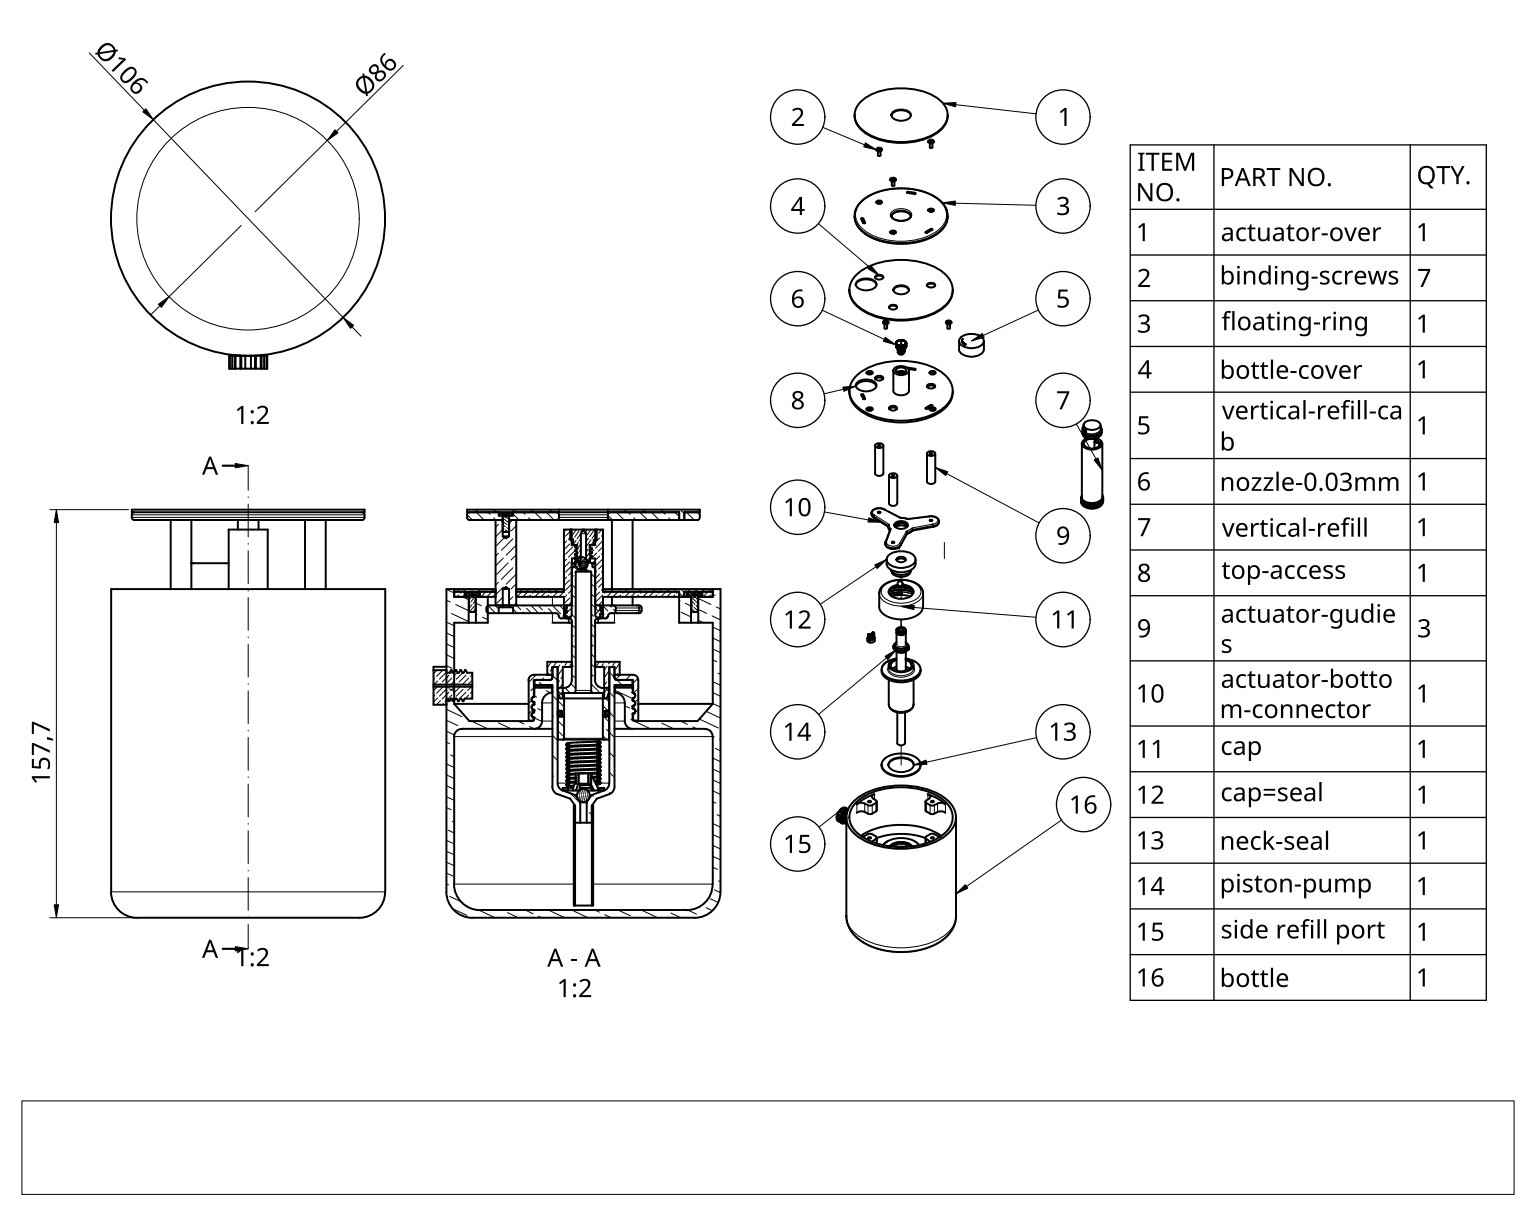
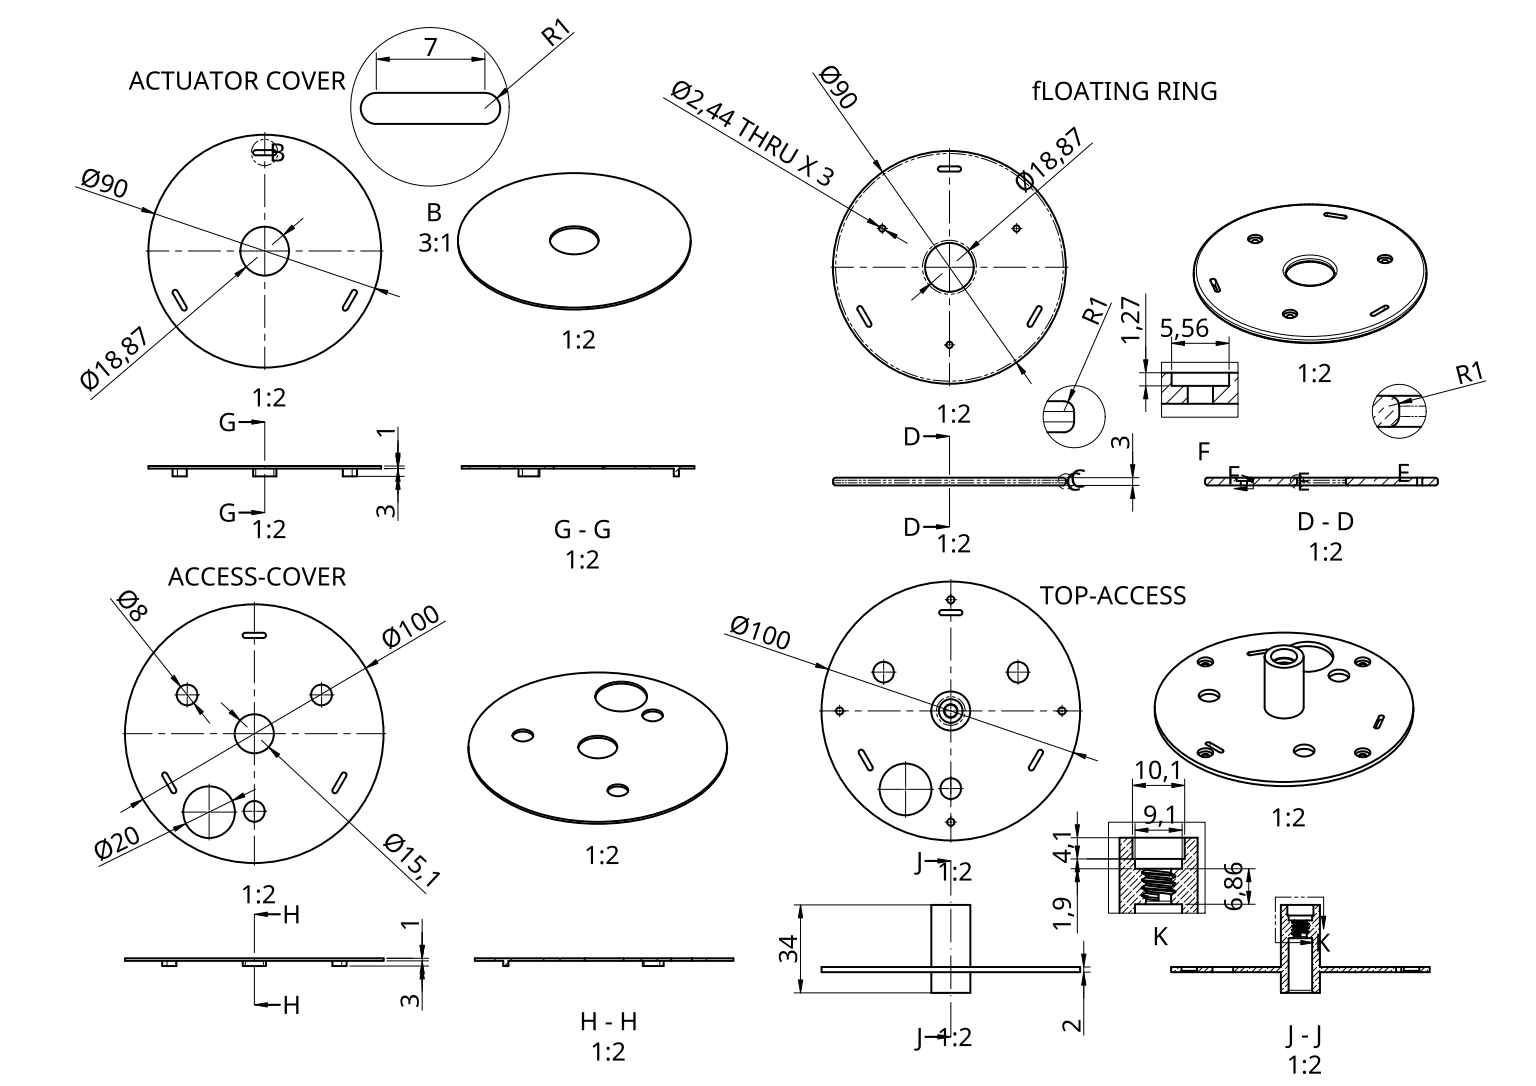
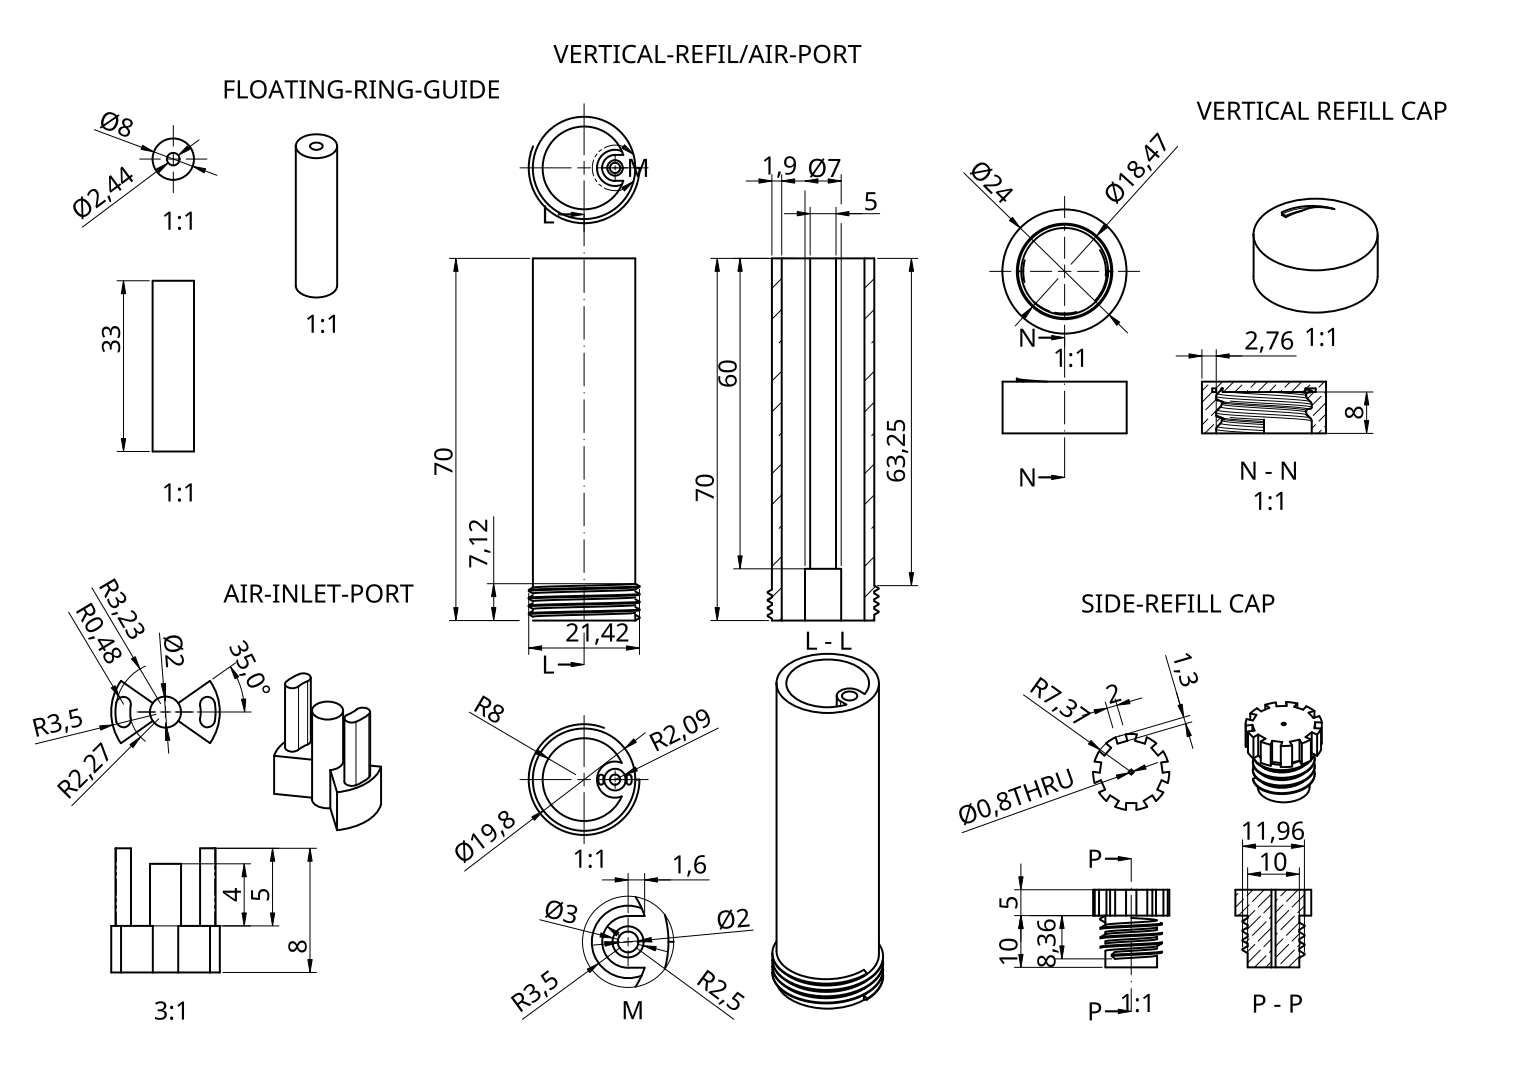
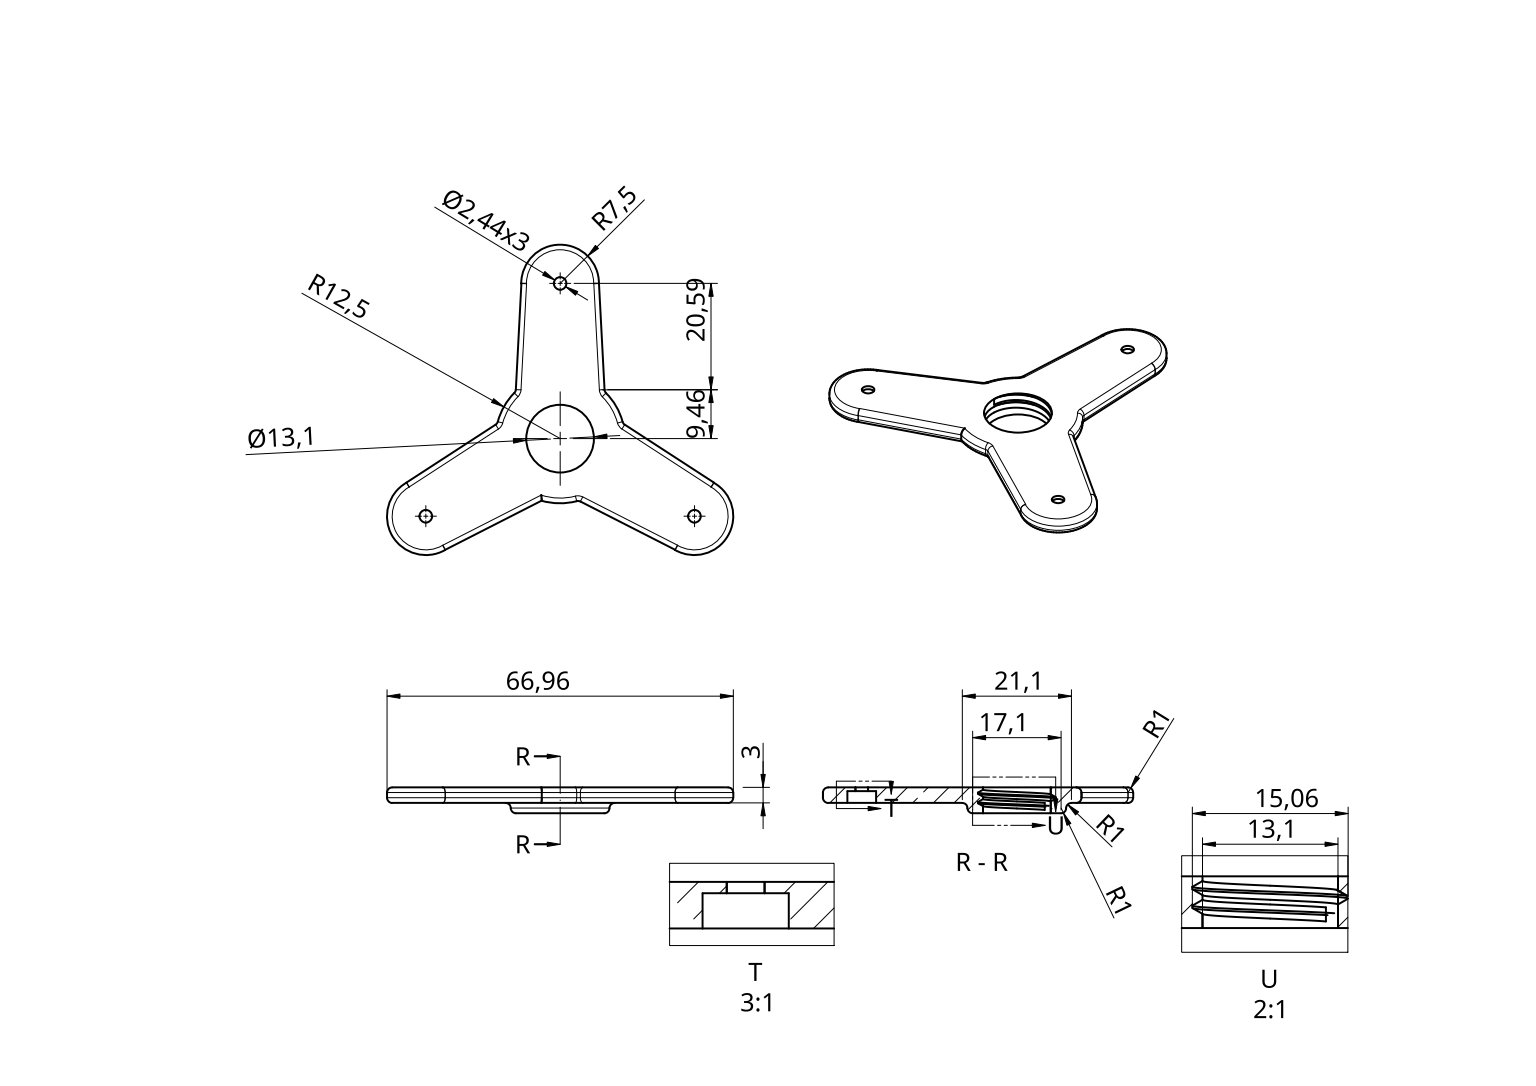
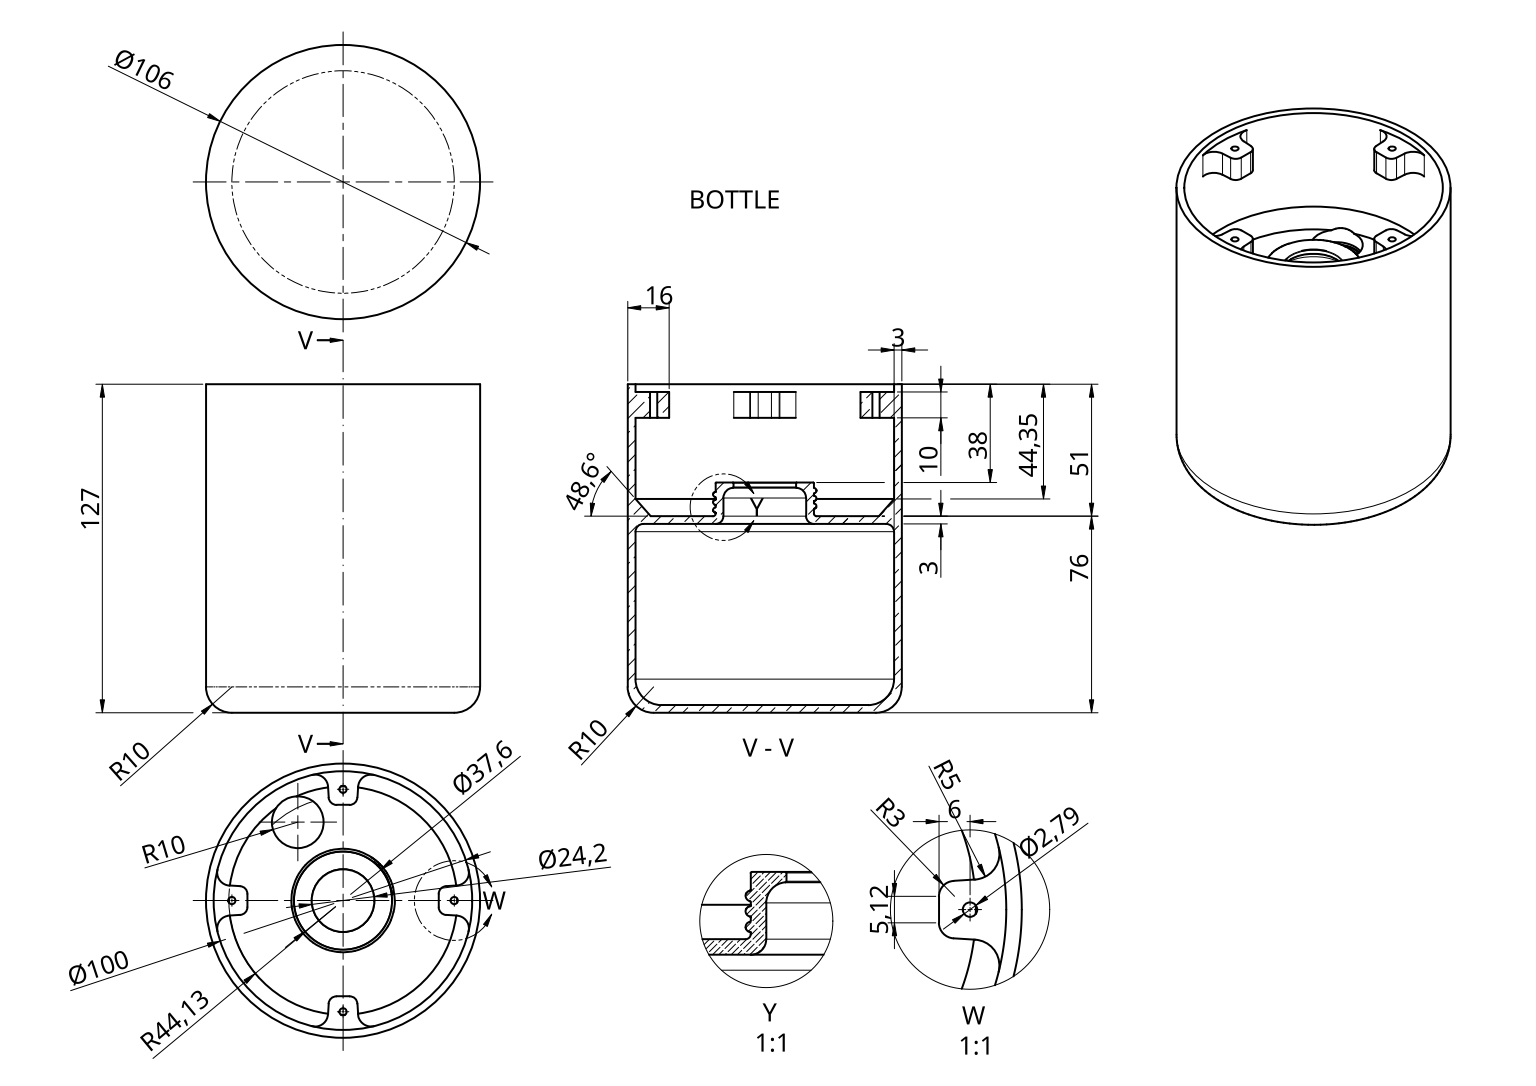
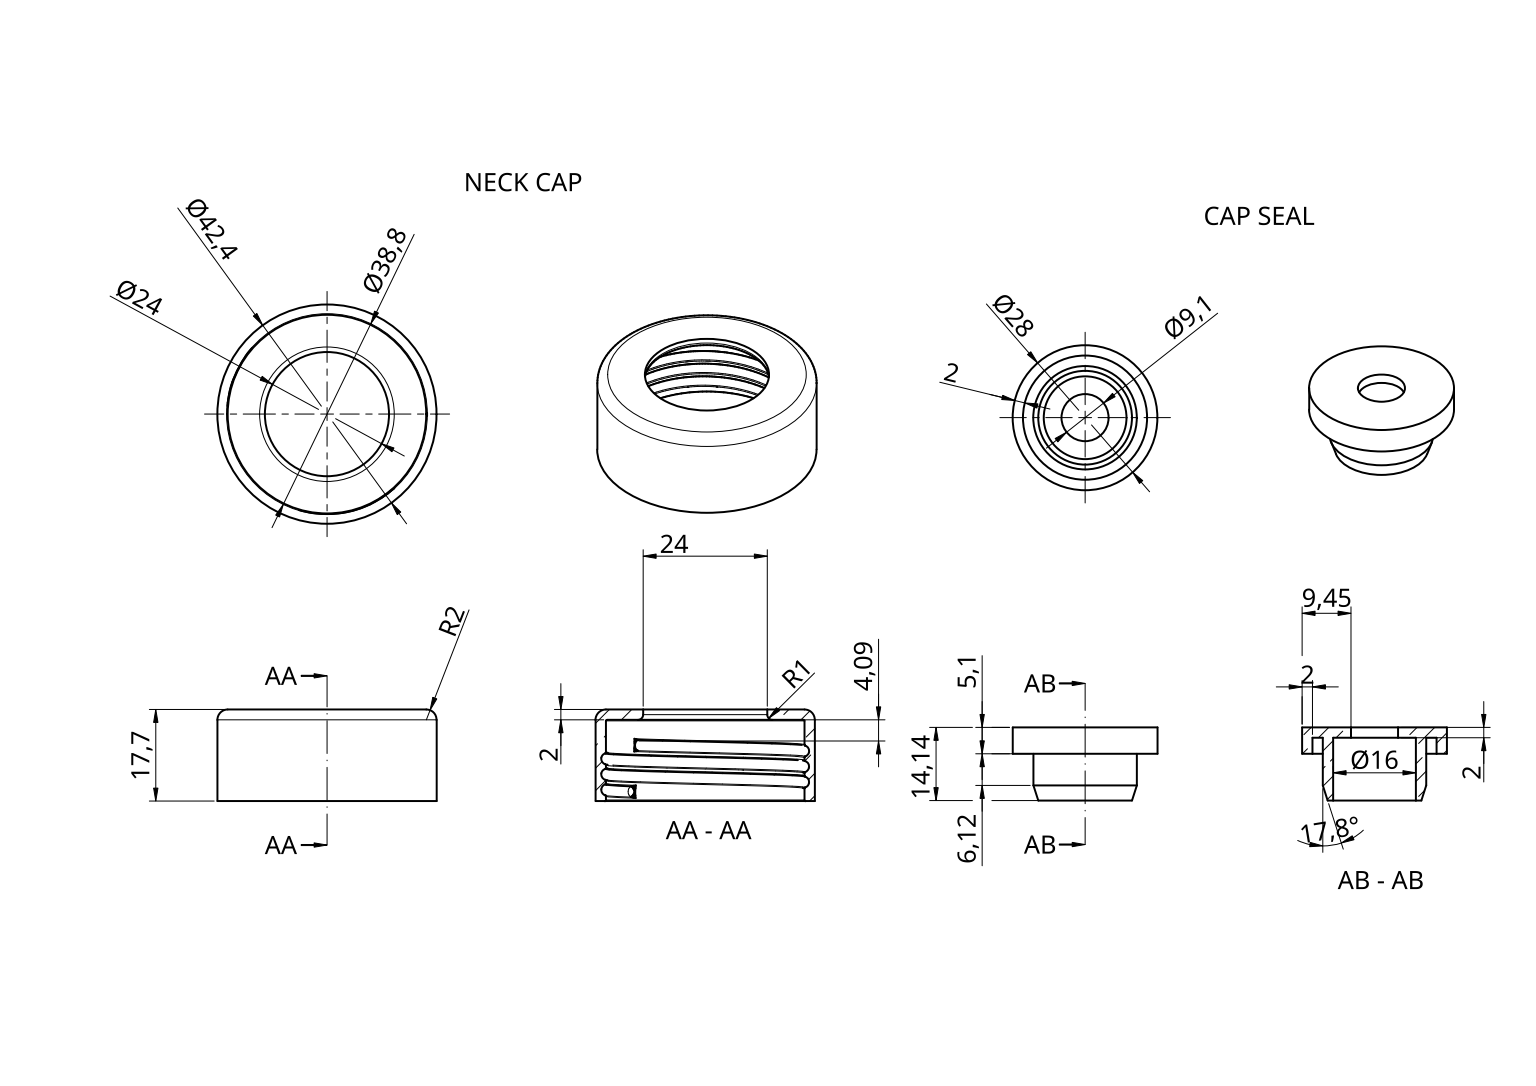
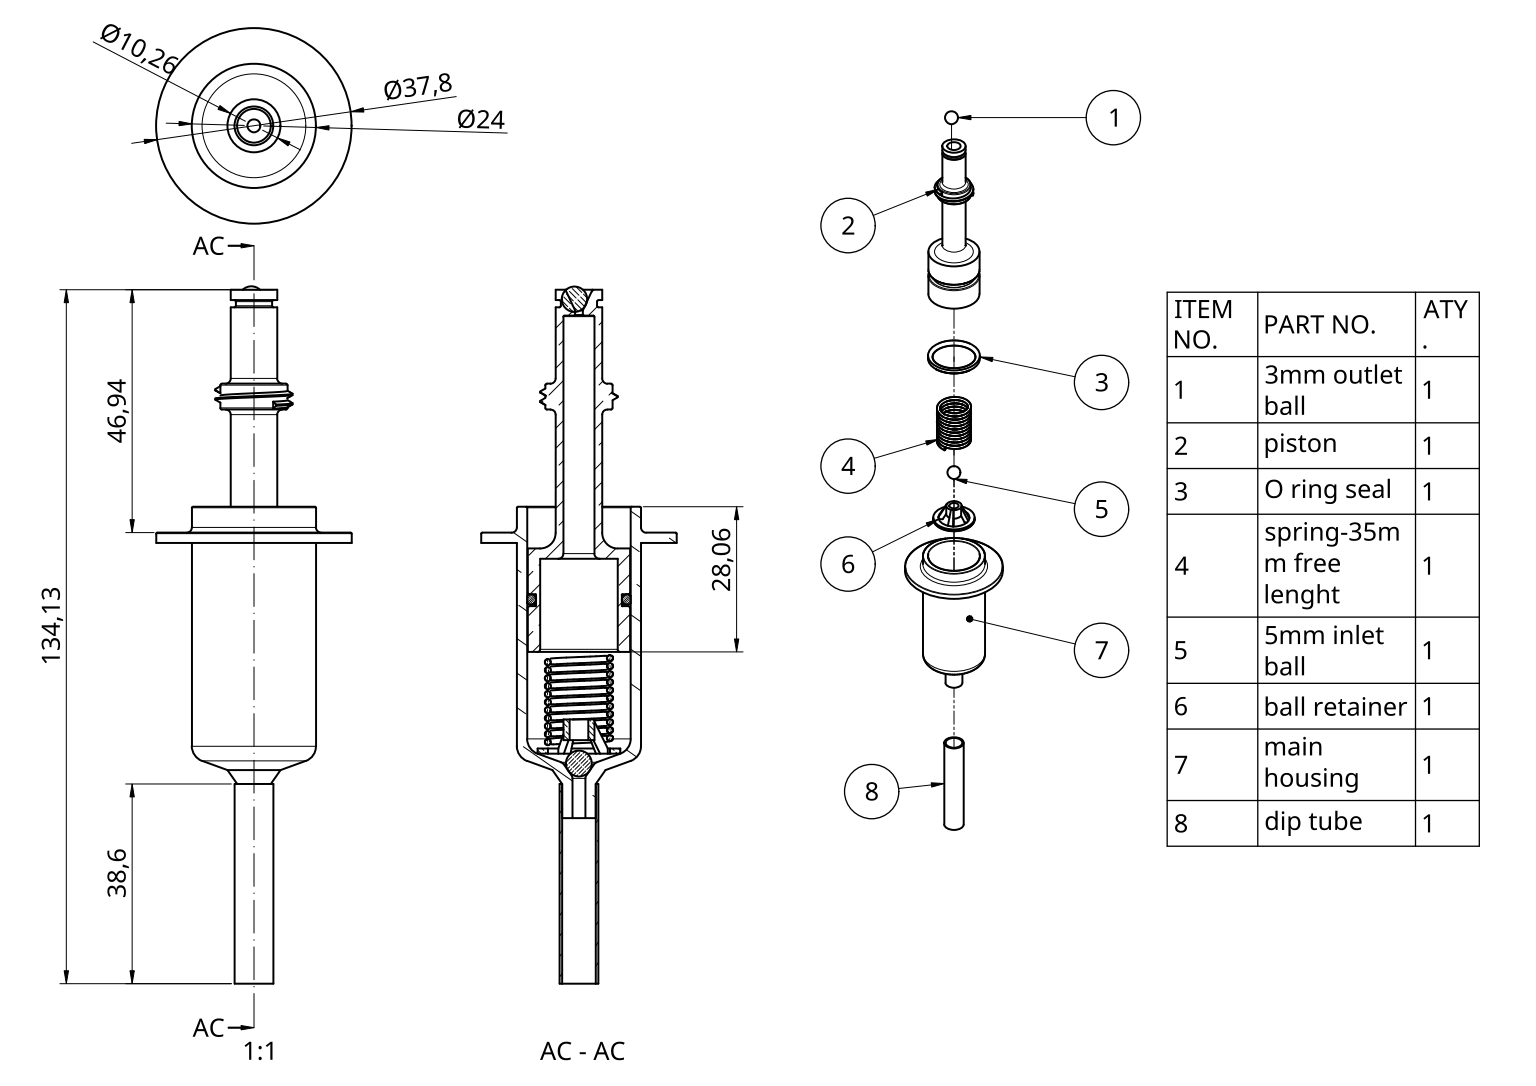
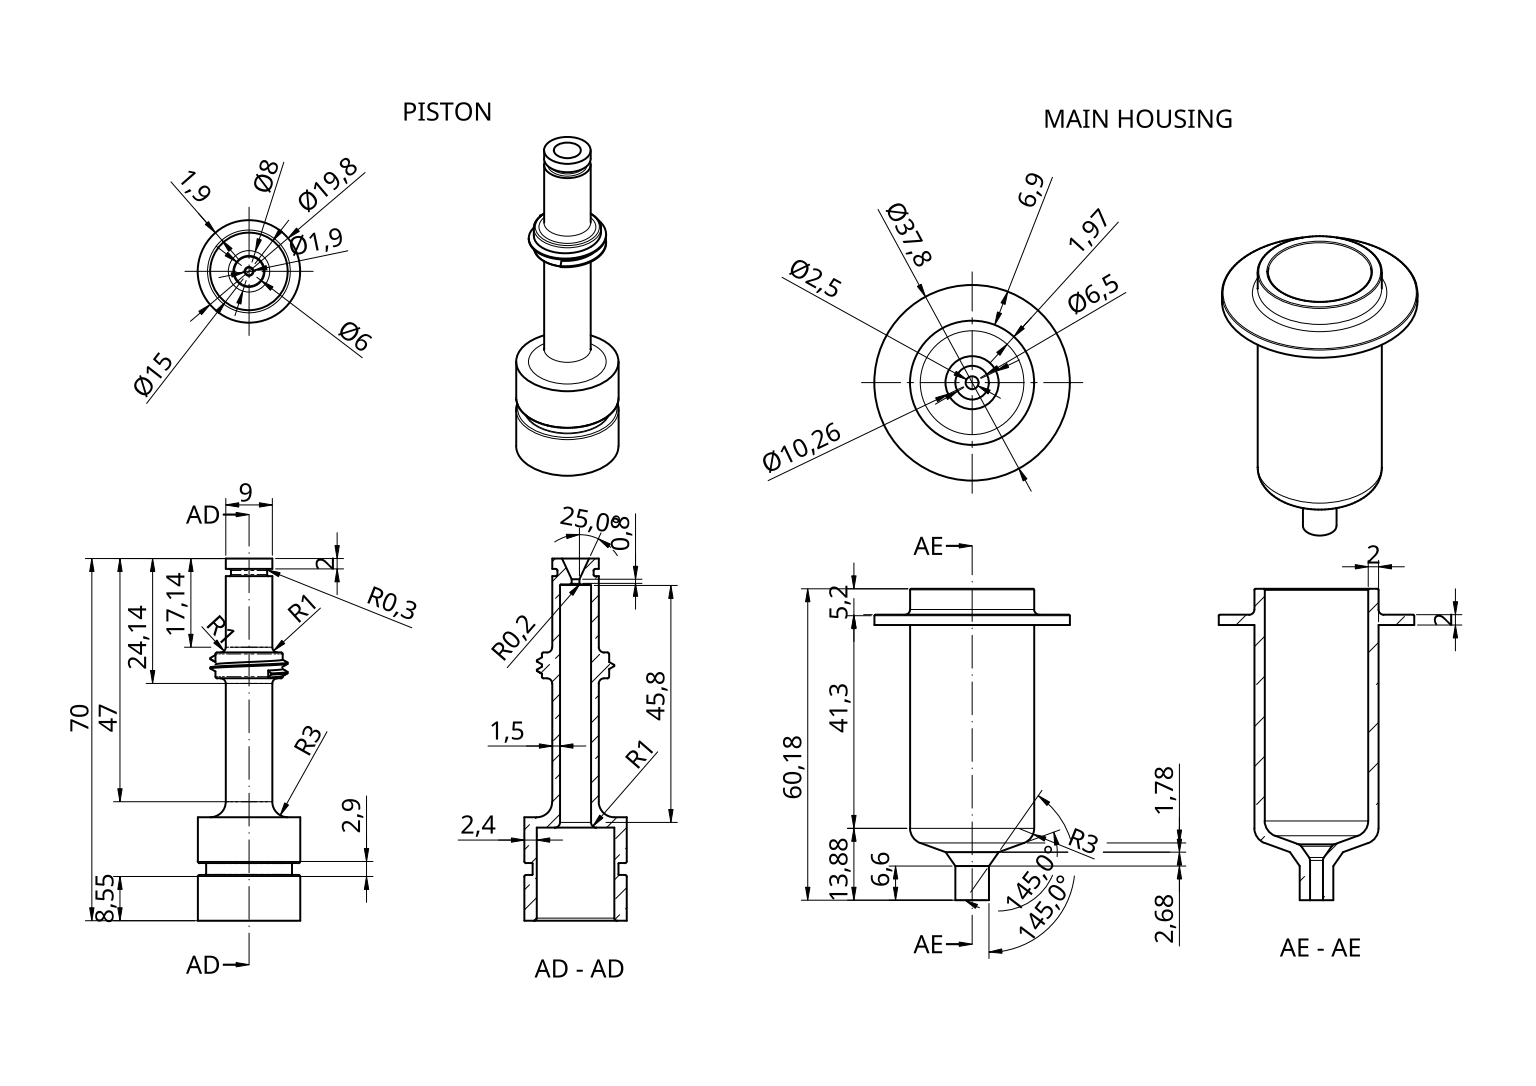
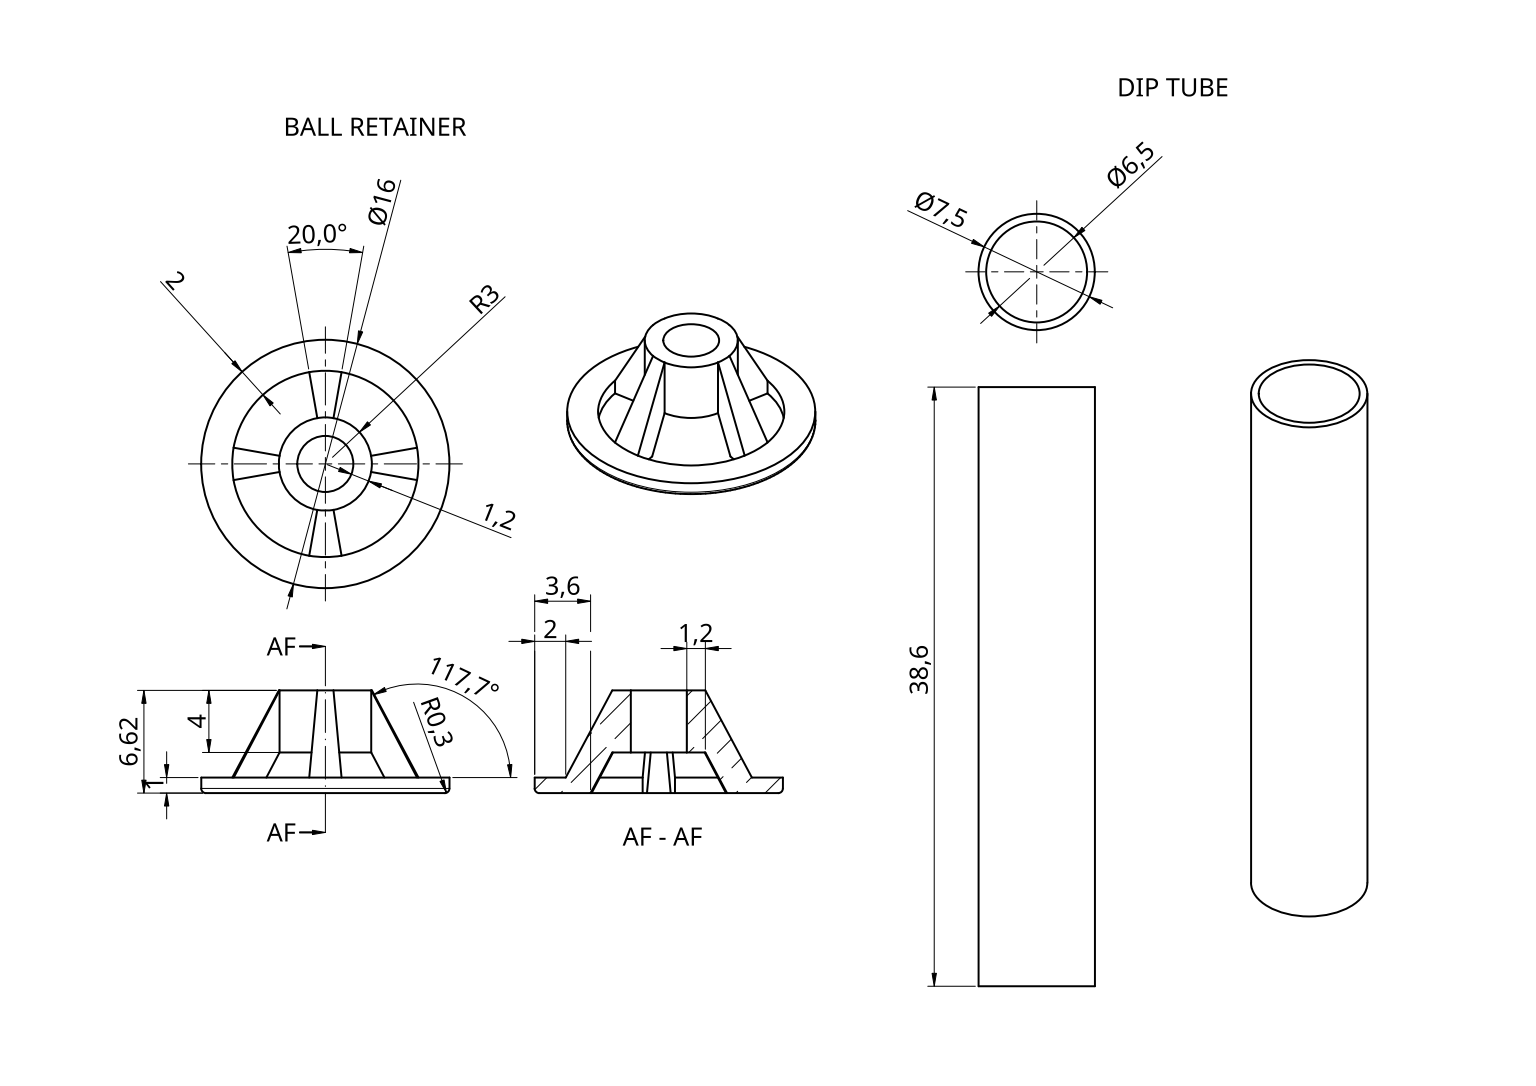
ISO-10303-21;
HEADER;
/* Generated by software containing ST-Developer
 * from STEP Tools, Inc. (www.steptools.com) 
 */
/* OPTION: using custom renumber hook */

FILE_DESCRIPTION(
/* description */ ('STEP AP242 Edition 2', 'CAx-IF Rec.Pracs.---Representation and Presentation of Product Manufa
cturing Information (PMI)---4.0---2014-10-13', 'CAx-IF Rec.Pracs.---3D Tessellated Geometry---0.4---2014-09-14', '2;1', 'CAx-IF Rec.Pracs.---User Defined Attributes---1.5---2016-08-15'),
/* implementation_level */ '2;1');

FILE_NAME(
/* name */ 'MAS-690',
/* time_stamp */ '2026-10-08T12:15:07Z',
/* author */ (''),
/* organization */ (''),
/* preprocessor_version */ 'ST-DEVELOPER v20',
/* originating_system */ 'ONSHAPE BY PTC INC, 1.221',
/* authorisation */ '  ');

FILE_SCHEMA (('AP242_MANAGED_MODEL_BASED_3D_ENGINEERING_MIM_LF { 1 0 10303 442 3 1 4 }'));
ENDSEC;

DATA;
#10=VERTEX_LOOP('',#7790);
#11=VERTEX_LOOP('',#7792);
#12=VERTEX_LOOP('',#8212);
#13=VERTEX_LOOP('',#8257);
#14=SPHERICAL_SURFACE('',#14256,0.00614054579032417);
#15=SPHERICAL_SURFACE('',#14380,0.001);
#16=SPHERICAL_SURFACE('',#14697,0.0015);
#17=SPHERICAL_SURFACE('',#14761,0.0025);
#18=SPHERICAL_SURFACE('',#15260,0.00100018366552404);
#19=SPHERICAL_SURFACE('',#15261,0.00100013782554506);
#20=SPHERICAL_SURFACE('',#15265,0.00100018686855117);
#21=CONICAL_SURFACE('',#13956,0.00075,0.436332312998577);
#22=CONICAL_SURFACE('',#14259,0.0026416,0.0872664625997183);
#23=CONICAL_SURFACE('',#14271,0.0012192,1.02974425867665);
#24=CONICAL_SURFACE('',#14272,0.0012192,1.02974425867665);
#25=CONICAL_SURFACE('',#14292,0.00906043638285393,0.310735335419369);
#26=CONICAL_SURFACE('',#14356,0.00512938524157182,1.22173047639604);
#27=CONICAL_SURFACE('',#14358,0.00325,0.610865238198018);
#28=CONICAL_SURFACE('',#14363,0.00312938524157182,0.610865238198019);
#29=CONICAL_SURFACE('',#14366,0.008,1.22173047639604);
#30=CONICAL_SURFACE('',#14962,0.05,0.723351005491207);
#31=CONICAL_SURFACE('',#15183,0.001,0.34906585039887);
#32=CONICAL_SURFACE('',#15246,0.003,0.49057568292852);
#33=CONICAL_SURFACE('',#15247,0.003,0.49057568292852);
#34=CONICAL_SURFACE('',#15248,0.003,0.49057568292852);
#35=CONICAL_SURFACE('',#15249,0.006,0.490575682928521);
#36=CONICAL_SURFACE('',#15250,0.006,0.490575682928521);
#37=CONICAL_SURFACE('',#15251,0.006,0.490575682928521);
#38=CONICAL_SURFACE('',#15253,0.006,0.490575682928521);
#39=CONICAL_SURFACE('',#15257,0.003,0.49057568292852);
#40=B_SPLINE_SURFACE_WITH_KNOTS('',3,3,((#20040,#20041,#20042,#20043,#20044,
#20045,#20046,#20047,#20048,#20049,#20050,#20051,#20052,#20053,#20054,#20055,
#20056,#20057,#20058,#20059,#20060,#20061,#20062,#20063,#20064,#20065,#20066,
#20067,#20068,#20069,#20070,#20071,#20072,#20073,#20074,#20075,#20076,#20077,
#20078,#20079,#20080,#20081,#20082,#20083,#20084,#20085,#20086,#20087,#20088,
#20089,#20090,#20091,#20092,#20093,#20094,#20095),(#20096,#20097,#20098,
#20099,#20100,#20101,#20102,#20103,#20104,#20105,#20106,#20107,#20108,#20109,
#20110,#20111,#20112,#20113,#20114,#20115,#20116,#20117,#20118,#20119,#20120,
#20121,#20122,#20123,#20124,#20125,#20126,#20127,#20128,#20129,#20130,#20131,
#20132,#20133,#20134,#20135,#20136,#20137,#20138,#20139,#20140,#20141,#20142,
#20143,#20144,#20145,#20146,#20147,#20148,#20149,#20150,#20151),(#20152,
#20153,#20154,#20155,#20156,#20157,#20158,#20159,#20160,#20161,#20162,#20163,
#20164,#20165,#20166,#20167,#20168,#20169,#20170,#20171,#20172,#20173,#20174,
#20175,#20176,#20177,#20178,#20179,#20180,#20181,#20182,#20183,#20184,#20185,
#20186,#20187,#20188,#20189,#20190,#20191,#20192,#20193,#20194,#20195,#20196,
#20197,#20198,#20199,#20200,#20201,#20202,#20203,#20204,#20205,#20206,#20207),
(#20208,#20209,#20210,#20211,#20212,#20213,#20214,#20215,#20216,#20217,
#20218,#20219,#20220,#20221,#20222,#20223,#20224,#20225,#20226,#20227,#20228,
#20229,#20230,#20231,#20232,#20233,#20234,#20235,#20236,#20237,#20238,#20239,
#20240,#20241,#20242,#20243,#20244,#20245,#20246,#20247,#20248,#20249,#20250,
#20251,#20252,#20253,#20254,#20255,#20256,#20257,#20258,#20259,#20260,#20261,
#20262,#20263)),.UNSPECIFIED.,.F.,.F.,.F.,(4,4),(4,2,2,2,2,2,2,2,2,2,2,
2,2,2,2,2,2,2,2,2,2,2,2,2,2,2,2,4),(0.,1.),(0.,0.05198235199969,0.077973527999535,
0.10396470399938,0.129955879999225,0.15594705599907,0.181938231998915,0.20792940799876,
0.233920583998605,0.25991175999845,0.285902935998295,0.31189411199814,0.337885287997985,
0.36387646399783,0.389867639997675,0.41585881599752,0.441849991997365,0.46784116799721,
0.493832343997055,0.5198235199969,0.57180587199659,0.62378822399628,0.67577057599597,
0.72775292799566,0.77973527999535,0.805726455995195,0.818722043995117,0.83171763199504),
 .UNSPECIFIED.);
#41=B_SPLINE_SURFACE_WITH_KNOTS('',3,3,((#20582,#20583,#20584,#20585,#20586,
#20587,#20588,#20589,#20590,#20591,#20592,#20593,#20594,#20595,#20596,#20597,
#20598,#20599,#20600,#20601,#20602,#20603,#20604,#20605,#20606,#20607,#20608,
#20609,#20610,#20611,#20612,#20613,#20614,#20615),(#20616,#20617,#20618,
#20619,#20620,#20621,#20622,#20623,#20624,#20625,#20626,#20627,#20628,#20629,
#20630,#20631,#20632,#20633,#20634,#20635,#20636,#20637,#20638,#20639,#20640,
#20641,#20642,#20643,#20644,#20645,#20646,#20647,#20648,#20649),(#20650,
#20651,#20652,#20653,#20654,#20655,#20656,#20657,#20658,#20659,#20660,#20661,
#20662,#20663,#20664,#20665,#20666,#20667,#20668,#20669,#20670,#20671,#20672,
#20673,#20674,#20675,#20676,#20677,#20678,#20679,#20680,#20681,#20682,#20683),
(#20684,#20685,#20686,#20687,#20688,#20689,#20690,#20691,#20692,#20693,
#20694,#20695,#20696,#20697,#20698,#20699,#20700,#20701,#20702,#20703,#20704,
#20705,#20706,#20707,#20708,#20709,#20710,#20711,#20712,#20713,#20714,#20715,
#20716,#20717),(#20718,#20719,#20720,#20721,#20722,#20723,#20724,#20725,
#20726,#20727,#20728,#20729,#20730,#20731,#20732,#20733,#20734,#20735,#20736,
#20737,#20738,#20739,#20740,#20741,#20742,#20743,#20744,#20745,#20746,#20747,
#20748,#20749,#20750,#20751),(#20752,#20753,#20754,#20755,#20756,#20757,
#20758,#20759,#20760,#20761,#20762,#20763,#20764,#20765,#20766,#20767,#20768,
#20769,#20770,#20771,#20772,#20773,#20774,#20775,#20776,#20777,#20778,#20779,
#20780,#20781,#20782,#20783,#20784,#20785),(#20786,#20787,#20788,#20789,
#20790,#20791,#20792,#20793,#20794,#20795,#20796,#20797,#20798,#20799,#20800,
#20801,#20802,#20803,#20804,#20805,#20806,#20807,#20808,#20809,#20810,#20811,
#20812,#20813,#20814,#20815,#20816,#20817,#20818,#20819),(#20820,#20821,
#20822,#20823,#20824,#20825,#20826,#20827,#20828,#20829,#20830,#20831,#20832,
#20833,#20834,#20835,#20836,#20837,#20838,#20839,#20840,#20841,#20842,#20843,
#20844,#20845,#20846,#20847,#20848,#20849,#20850,#20851,#20852,#20853),
(#20854,#20855,#20856,#20857,#20858,#20859,#20860,#20861,#20862,#20863,
#20864,#20865,#20866,#20867,#20868,#20869,#20870,#20871,#20872,#20873,#20874,
#20875,#20876,#20877,#20878,#20879,#20880,#20881,#20882,#20883,#20884,#20885,
#20886,#20887),(#20888,#20889,#20890,#20891,#20892,#20893,#20894,#20895,
#20896,#20897,#20898,#20899,#20900,#20901,#20902,#20903,#20904,#20905,#20906,
#20907,#20908,#20909,#20910,#20911,#20912,#20913,#20914,#20915,#20916,#20917,
#20918,#20919,#20920,#20921),(#20922,#20923,#20924,#20925,#20926,#20927,
#20928,#20929,#20930,#20931,#20932,#20933,#20934,#20935,#20936,#20937,#20938,
#20939,#20940,#20941,#20942,#20943,#20944,#20945,#20946,#20947,#20948,#20949,
#20950,#20951,#20952,#20953,#20954,#20955),(#20956,#20957,#20958,#20959,
#20960,#20961,#20962,#20963,#20964,#20965,#20966,#20967,#20968,#20969,#20970,
#20971,#20972,#20973,#20974,#20975,#20976,#20977,#20978,#20979,#20980,#20981,
#20982,#20983,#20984,#20985,#20986,#20987,#20988,#20989),(#20990,#20991,
#20992,#20993,#20994,#20995,#20996,#20997,#20998,#20999,#21000,#21001,#21002,
#21003,#21004,#21005,#21006,#21007,#21008,#21009,#21010,#21011,#21012,#21013,
#21014,#21015,#21016,#21017,#21018,#21019,#21020,#21021,#21022,#21023),
(#21024,#21025,#21026,#21027,#21028,#21029,#21030,#21031,#21032,#21033,
#21034,#21035,#21036,#21037,#21038,#21039,#21040,#21041,#21042,#21043,#21044,
#21045,#21046,#21047,#21048,#21049,#21050,#21051,#21052,#21053,#21054,#21055,
#21056,#21057)),.UNSPECIFIED.,.F.,.F.,.F.,(4,2,2,2,2,2,4),(4,2,2,2,2,2,
2,2,2,2,2,2,2,2,2,2,4),(0.496999950768087,0.5,0.625,0.75,0.875,1.,1.00300004881078),
(-0.00600030525376163,0.0450000000000826,0.110000000000075,0.175000000000067,
0.24000000000006,0.305000000000052,0.370000000000045,0.435000000000037,
0.500000000000029,0.565000000000022,0.630000000000014,0.695,0.76,0.824999999999991,
0.889999999999984,0.954999999999976,1.00600015524748),.UNSPECIFIED.);
#42=B_SPLINE_SURFACE_WITH_KNOTS('',3,3,((#21089,#21090,#21091,#21092,#21093,
#21094,#21095,#21096,#21097,#21098,#21099,#21100,#21101,#21102,#21103,#21104,
#21105,#21106,#21107,#21108,#21109,#21110,#21111,#21112,#21113,#21114,#21115,
#21116,#21117,#21118,#21119,#21120,#21121,#21122),(#21123,#21124,#21125,
#21126,#21127,#21128,#21129,#21130,#21131,#21132,#21133,#21134,#21135,#21136,
#21137,#21138,#21139,#21140,#21141,#21142,#21143,#21144,#21145,#21146,#21147,
#21148,#21149,#21150,#21151,#21152,#21153,#21154,#21155,#21156),(#21157,
#21158,#21159,#21160,#21161,#21162,#21163,#21164,#21165,#21166,#21167,#21168,
#21169,#21170,#21171,#21172,#21173,#21174,#21175,#21176,#21177,#21178,#21179,
#21180,#21181,#21182,#21183,#21184,#21185,#21186,#21187,#21188,#21189,#21190),
(#21191,#21192,#21193,#21194,#21195,#21196,#21197,#21198,#21199,#21200,
#21201,#21202,#21203,#21204,#21205,#21206,#21207,#21208,#21209,#21210,#21211,
#21212,#21213,#21214,#21215,#21216,#21217,#21218,#21219,#21220,#21221,#21222,
#21223,#21224),(#21225,#21226,#21227,#21228,#21229,#21230,#21231,#21232,
#21233,#21234,#21235,#21236,#21237,#21238,#21239,#21240,#21241,#21242,#21243,
#21244,#21245,#21246,#21247,#21248,#21249,#21250,#21251,#21252,#21253,#21254,
#21255,#21256,#21257,#21258),(#21259,#21260,#21261,#21262,#21263,#21264,
#21265,#21266,#21267,#21268,#21269,#21270,#21271,#21272,#21273,#21274,#21275,
#21276,#21277,#21278,#21279,#21280,#21281,#21282,#21283,#21284,#21285,#21286,
#21287,#21288,#21289,#21290,#21291,#21292),(#21293,#21294,#21295,#21296,
#21297,#21298,#21299,#21300,#21301,#21302,#21303,#21304,#21305,#21306,#21307,
#21308,#21309,#21310,#21311,#21312,#21313,#21314,#21315,#21316,#21317,#21318,
#21319,#21320,#21321,#21322,#21323,#21324,#21325,#21326),(#21327,#21328,
#21329,#21330,#21331,#21332,#21333,#21334,#21335,#21336,#21337,#21338,#21339,
#21340,#21341,#21342,#21343,#21344,#21345,#21346,#21347,#21348,#21349,#21350,
#21351,#21352,#21353,#21354,#21355,#21356,#21357,#21358,#21359,#21360),
(#21361,#21362,#21363,#21364,#21365,#21366,#21367,#21368,#21369,#21370,
#21371,#21372,#21373,#21374,#21375,#21376,#21377,#21378,#21379,#21380,#21381,
#21382,#21383,#21384,#21385,#21386,#21387,#21388,#21389,#21390,#21391,#21392,
#21393,#21394),(#21395,#21396,#21397,#21398,#21399,#21400,#21401,#21402,
#21403,#21404,#21405,#21406,#21407,#21408,#21409,#21410,#21411,#21412,#21413,
#21414,#21415,#21416,#21417,#21418,#21419,#21420,#21421,#21422,#21423,#21424,
#21425,#21426,#21427,#21428),(#21429,#21430,#21431,#21432,#21433,#21434,
#21435,#21436,#21437,#21438,#21439,#21440,#21441,#21442,#21443,#21444,#21445,
#21446,#21447,#21448,#21449,#21450,#21451,#21452,#21453,#21454,#21455,#21456,
#21457,#21458,#21459,#21460,#21461,#21462),(#21463,#21464,#21465,#21466,
#21467,#21468,#21469,#21470,#21471,#21472,#21473,#21474,#21475,#21476,#21477,
#21478,#21479,#21480,#21481,#21482,#21483,#21484,#21485,#21486,#21487,#21488,
#21489,#21490,#21491,#21492,#21493,#21494,#21495,#21496),(#21497,#21498,
#21499,#21500,#21501,#21502,#21503,#21504,#21505,#21506,#21507,#21508,#21509,
#21510,#21511,#21512,#21513,#21514,#21515,#21516,#21517,#21518,#21519,#21520,
#21521,#21522,#21523,#21524,#21525,#21526,#21527,#21528,#21529,#21530),
(#21531,#21532,#21533,#21534,#21535,#21536,#21537,#21538,#21539,#21540,
#21541,#21542,#21543,#21544,#21545,#21546,#21547,#21548,#21549,#21550,#21551,
#21552,#21553,#21554,#21555,#21556,#21557,#21558,#21559,#21560,#21561,#21562,
#21563,#21564)),.UNSPECIFIED.,.F.,.F.,.F.,(4,2,2,2,2,2,4),(4,2,2,2,2,2,
2,2,2,2,2,2,2,2,2,2,4),(-0.00024497105823581,0.,0.125,0.25,0.375,0.5,0.500244971058236),
(-1.90758107793014E-7,0.0450000000000825,0.110000000000075,0.175000000000067,
0.240000000000059,0.305000000000052,0.370000000000044,0.435000000000037,
0.500000000000029,0.565000000000021,0.630000000000014,0.695,0.76,0.824999999999991,
0.889999999999983,0.954999999999975,1.00000029951007),.UNSPECIFIED.);
#43=B_SPLINE_SURFACE_WITH_KNOTS('',3,3,((#21676,#21677,#21678,#21679,#21680,
#21681,#21682,#21683,#21684,#21685,#21686,#21687,#21688,#21689,#21690,#21691,
#21692,#21693,#21694,#21695,#21696,#21697,#21698,#21699,#21700,#21701,#21702,
#21703,#21704,#21705,#21706,#21707,#21708,#21709),(#21710,#21711,#21712,
#21713,#21714,#21715,#21716,#21717,#21718,#21719,#21720,#21721,#21722,#21723,
#21724,#21725,#21726,#21727,#21728,#21729,#21730,#21731,#21732,#21733,#21734,
#21735,#21736,#21737,#21738,#21739,#21740,#21741,#21742,#21743),(#21744,
#21745,#21746,#21747,#21748,#21749,#21750,#21751,#21752,#21753,#21754,#21755,
#21756,#21757,#21758,#21759,#21760,#21761,#21762,#21763,#21764,#21765,#21766,
#21767,#21768,#21769,#21770,#21771,#21772,#21773,#21774,#21775,#21776,#21777),
(#21778,#21779,#21780,#21781,#21782,#21783,#21784,#21785,#21786,#21787,
#21788,#21789,#21790,#21791,#21792,#21793,#21794,#21795,#21796,#21797,#21798,
#21799,#21800,#21801,#21802,#21803,#21804,#21805,#21806,#21807,#21808,#21809,
#21810,#21811),(#21812,#21813,#21814,#21815,#21816,#21817,#21818,#21819,
#21820,#21821,#21822,#21823,#21824,#21825,#21826,#21827,#21828,#21829,#21830,
#21831,#21832,#21833,#21834,#21835,#21836,#21837,#21838,#21839,#21840,#21841,
#21842,#21843,#21844,#21845),(#21846,#21847,#21848,#21849,#21850,#21851,
#21852,#21853,#21854,#21855,#21856,#21857,#21858,#21859,#21860,#21861,#21862,
#21863,#21864,#21865,#21866,#21867,#21868,#21869,#21870,#21871,#21872,#21873,
#21874,#21875,#21876,#21877,#21878,#21879),(#21880,#21881,#21882,#21883,
#21884,#21885,#21886,#21887,#21888,#21889,#21890,#21891,#21892,#21893,#21894,
#21895,#21896,#21897,#21898,#21899,#21900,#21901,#21902,#21903,#21904,#21905,
#21906,#21907,#21908,#21909,#21910,#21911,#21912,#21913),(#21914,#21915,
#21916,#21917,#21918,#21919,#21920,#21921,#21922,#21923,#21924,#21925,#21926,
#21927,#21928,#21929,#21930,#21931,#21932,#21933,#21934,#21935,#21936,#21937,
#21938,#21939,#21940,#21941,#21942,#21943,#21944,#21945,#21946,#21947),
(#21948,#21949,#21950,#21951,#21952,#21953,#21954,#21955,#21956,#21957,
#21958,#21959,#21960,#21961,#21962,#21963,#21964,#21965,#21966,#21967,#21968,
#21969,#21970,#21971,#21972,#21973,#21974,#21975,#21976,#21977,#21978,#21979,
#21980,#21981),(#21982,#21983,#21984,#21985,#21986,#21987,#21988,#21989,
#21990,#21991,#21992,#21993,#21994,#21995,#21996,#21997,#21998,#21999,#22000,
#22001,#22002,#22003,#22004,#22005,#22006,#22007,#22008,#22009,#22010,#22011,
#22012,#22013,#22014,#22015),(#22016,#22017,#22018,#22019,#22020,#22021,
#22022,#22023,#22024,#22025,#22026,#22027,#22028,#22029,#22030,#22031,#22032,
#22033,#22034,#22035,#22036,#22037,#22038,#22039,#22040,#22041,#22042,#22043,
#22044,#22045,#22046,#22047,#22048,#22049),(#22050,#22051,#22052,#22053,
#22054,#22055,#22056,#22057,#22058,#22059,#22060,#22061,#22062,#22063,#22064,
#22065,#22066,#22067,#22068,#22069,#22070,#22071,#22072,#22073,#22074,#22075,
#22076,#22077,#22078,#22079,#22080,#22081,#22082,#22083),(#22084,#22085,
#22086,#22087,#22088,#22089,#22090,#22091,#22092,#22093,#22094,#22095,#22096,
#22097,#22098,#22099,#22100,#22101,#22102,#22103,#22104,#22105,#22106,#22107,
#22108,#22109,#22110,#22111,#22112,#22113,#22114,#22115,#22116,#22117),
(#22118,#22119,#22120,#22121,#22122,#22123,#22124,#22125,#22126,#22127,
#22128,#22129,#22130,#22131,#22132,#22133,#22134,#22135,#22136,#22137,#22138,
#22139,#22140,#22141,#22142,#22143,#22144,#22145,#22146,#22147,#22148,#22149,
#22150,#22151),(#22152,#22153,#22154,#22155,#22156,#22157,#22158,#22159,
#22160,#22161,#22162,#22163,#22164,#22165,#22166,#22167,#22168,#22169,#22170,
#22171,#22172,#22173,#22174,#22175,#22176,#22177,#22178,#22179,#22180,#22181,
#22182,#22183,#22184,#22185),(#22186,#22187,#22188,#22189,#22190,#22191,
#22192,#22193,#22194,#22195,#22196,#22197,#22198,#22199,#22200,#22201,#22202,
#22203,#22204,#22205,#22206,#22207,#22208,#22209,#22210,#22211,#22212,#22213,
#22214,#22215,#22216,#22217,#22218,#22219)),.UNSPECIFIED.,.F.,.F.,.F.,(4,
2,2,2,2,2,2,4),(4,2,2,2,2,2,2,2,2,2,2,2,2,2,2,2,4),(0.499748503678476,0.5,
0.6,0.7,0.8,0.9,1.,1.00025149632152),(-1.92698650980853E-7,0.0450000000000825,
0.110000000000075,0.175000000000067,0.240000000000059,0.305000000000052,
0.370000000000044,0.435000000000037,0.500000000000029,0.565000000000021,
0.630000000000013,0.695,0.76,0.82499999999999,0.889999999999983,0.954999999999975,
1.00000029951007),.UNSPECIFIED.);
#44=B_SPLINE_SURFACE_WITH_KNOTS('',3,3,((#22251,#22252,#22253,#22254,#22255,
#22256,#22257,#22258,#22259,#22260,#22261,#22262,#22263,#22264,#22265,#22266,
#22267,#22268,#22269,#22270,#22271,#22272,#22273,#22274,#22275,#22276,#22277,
#22278,#22279,#22280,#22281,#22282,#22283,#22284),(#22285,#22286,#22287,
#22288,#22289,#22290,#22291,#22292,#22293,#22294,#22295,#22296,#22297,#22298,
#22299,#22300,#22301,#22302,#22303,#22304,#22305,#22306,#22307,#22308,#22309,
#22310,#22311,#22312,#22313,#22314,#22315,#22316,#22317,#22318),(#22319,
#22320,#22321,#22322,#22323,#22324,#22325,#22326,#22327,#22328,#22329,#22330,
#22331,#22332,#22333,#22334,#22335,#22336,#22337,#22338,#22339,#22340,#22341,
#22342,#22343,#22344,#22345,#22346,#22347,#22348,#22349,#22350,#22351,#22352),
(#22353,#22354,#22355,#22356,#22357,#22358,#22359,#22360,#22361,#22362,
#22363,#22364,#22365,#22366,#22367,#22368,#22369,#22370,#22371,#22372,#22373,
#22374,#22375,#22376,#22377,#22378,#22379,#22380,#22381,#22382,#22383,#22384,
#22385,#22386),(#22387,#22388,#22389,#22390,#22391,#22392,#22393,#22394,
#22395,#22396,#22397,#22398,#22399,#22400,#22401,#22402,#22403,#22404,#22405,
#22406,#22407,#22408,#22409,#22410,#22411,#22412,#22413,#22414,#22415,#22416,
#22417,#22418,#22419,#22420),(#22421,#22422,#22423,#22424,#22425,#22426,
#22427,#22428,#22429,#22430,#22431,#22432,#22433,#22434,#22435,#22436,#22437,
#22438,#22439,#22440,#22441,#22442,#22443,#22444,#22445,#22446,#22447,#22448,
#22449,#22450,#22451,#22452,#22453,#22454),(#22455,#22456,#22457,#22458,
#22459,#22460,#22461,#22462,#22463,#22464,#22465,#22466,#22467,#22468,#22469,
#22470,#22471,#22472,#22473,#22474,#22475,#22476,#22477,#22478,#22479,#22480,
#22481,#22482,#22483,#22484,#22485,#22486,#22487,#22488),(#22489,#22490,
#22491,#22492,#22493,#22494,#22495,#22496,#22497,#22498,#22499,#22500,#22501,
#22502,#22503,#22504,#22505,#22506,#22507,#22508,#22509,#22510,#22511,#22512,
#22513,#22514,#22515,#22516,#22517,#22518,#22519,#22520,#22521,#22522),
(#22523,#22524,#22525,#22526,#22527,#22528,#22529,#22530,#22531,#22532,
#22533,#22534,#22535,#22536,#22537,#22538,#22539,#22540,#22541,#22542,#22543,
#22544,#22545,#22546,#22547,#22548,#22549,#22550,#22551,#22552,#22553,#22554,
#22555,#22556),(#22557,#22558,#22559,#22560,#22561,#22562,#22563,#22564,
#22565,#22566,#22567,#22568,#22569,#22570,#22571,#22572,#22573,#22574,#22575,
#22576,#22577,#22578,#22579,#22580,#22581,#22582,#22583,#22584,#22585,#22586,
#22587,#22588,#22589,#22590),(#22591,#22592,#22593,#22594,#22595,#22596,
#22597,#22598,#22599,#22600,#22601,#22602,#22603,#22604,#22605,#22606,#22607,
#22608,#22609,#22610,#22611,#22612,#22613,#22614,#22615,#22616,#22617,#22618,
#22619,#22620,#22621,#22622,#22623,#22624),(#22625,#22626,#22627,#22628,
#22629,#22630,#22631,#22632,#22633,#22634,#22635,#22636,#22637,#22638,#22639,
#22640,#22641,#22642,#22643,#22644,#22645,#22646,#22647,#22648,#22649,#22650,
#22651,#22652,#22653,#22654,#22655,#22656,#22657,#22658),(#22659,#22660,
#22661,#22662,#22663,#22664,#22665,#22666,#22667,#22668,#22669,#22670,#22671,
#22672,#22673,#22674,#22675,#22676,#22677,#22678,#22679,#22680,#22681,#22682,
#22683,#22684,#22685,#22686,#22687,#22688,#22689,#22690,#22691,#22692),
(#22693,#22694,#22695,#22696,#22697,#22698,#22699,#22700,#22701,#22702,
#22703,#22704,#22705,#22706,#22707,#22708,#22709,#22710,#22711,#22712,#22713,
#22714,#22715,#22716,#22717,#22718,#22719,#22720,#22721,#22722,#22723,#22724,
#22725,#22726)),.UNSPECIFIED.,.F.,.F.,.F.,(4,2,2,2,2,2,4),(4,2,2,2,2,2,
2,2,2,2,2,2,2,2,2,2,4),(0.487638113642685,0.5,0.625,0.75,0.875,1.,1.01236188635731),
(9.7389676693069,10.1395200046188,10.5400723399307,10.9406246752426,11.3411770105545,
11.7417293458665,12.1422816811784,12.5428340164903,12.9433863518022,13.3439386871141,
13.744491022426,14.1450433577379,14.5455956930498,14.9461480283618,15.3467003636736,
15.7472526989856,16.1478050342975),.UNSPECIFIED.);
#45=B_SPLINE_SURFACE_WITH_KNOTS('',3,3,((#22758,#22759,#22760,#22761,#22762,
#22763,#22764,#22765,#22766,#22767,#22768,#22769,#22770,#22771,#22772,#22773,
#22774,#22775,#22776,#22777,#22778,#22779,#22780,#22781,#22782,#22783,#22784,
#22785,#22786,#22787,#22788,#22789,#22790,#22791),(#22792,#22793,#22794,
#22795,#22796,#22797,#22798,#22799,#22800,#22801,#22802,#22803,#22804,#22805,
#22806,#22807,#22808,#22809,#22810,#22811,#22812,#22813,#22814,#22815,#22816,
#22817,#22818,#22819,#22820,#22821,#22822,#22823,#22824,#22825),(#22826,
#22827,#22828,#22829,#22830,#22831,#22832,#22833,#22834,#22835,#22836,#22837,
#22838,#22839,#22840,#22841,#22842,#22843,#22844,#22845,#22846,#22847,#22848,
#22849,#22850,#22851,#22852,#22853,#22854,#22855,#22856,#22857,#22858,#22859),
(#22860,#22861,#22862,#22863,#22864,#22865,#22866,#22867,#22868,#22869,
#22870,#22871,#22872,#22873,#22874,#22875,#22876,#22877,#22878,#22879,#22880,
#22881,#22882,#22883,#22884,#22885,#22886,#22887,#22888,#22889,#22890,#22891,
#22892,#22893),(#22894,#22895,#22896,#22897,#22898,#22899,#22900,#22901,
#22902,#22903,#22904,#22905,#22906,#22907,#22908,#22909,#22910,#22911,#22912,
#22913,#22914,#22915,#22916,#22917,#22918,#22919,#22920,#22921,#22922,#22923,
#22924,#22925,#22926,#22927),(#22928,#22929,#22930,#22931,#22932,#22933,
#22934,#22935,#22936,#22937,#22938,#22939,#22940,#22941,#22942,#22943,#22944,
#22945,#22946,#22947,#22948,#22949,#22950,#22951,#22952,#22953,#22954,#22955,
#22956,#22957,#22958,#22959,#22960,#22961),(#22962,#22963,#22964,#22965,
#22966,#22967,#22968,#22969,#22970,#22971,#22972,#22973,#22974,#22975,#22976,
#22977,#22978,#22979,#22980,#22981,#22982,#22983,#22984,#22985,#22986,#22987,
#22988,#22989,#22990,#22991,#22992,#22993,#22994,#22995),(#22996,#22997,
#22998,#22999,#23000,#23001,#23002,#23003,#23004,#23005,#23006,#23007,#23008,
#23009,#23010,#23011,#23012,#23013,#23014,#23015,#23016,#23017,#23018,#23019,
#23020,#23021,#23022,#23023,#23024,#23025,#23026,#23027,#23028,#23029),
(#23030,#23031,#23032,#23033,#23034,#23035,#23036,#23037,#23038,#23039,
#23040,#23041,#23042,#23043,#23044,#23045,#23046,#23047,#23048,#23049,#23050,
#23051,#23052,#23053,#23054,#23055,#23056,#23057,#23058,#23059,#23060,#23061,
#23062,#23063),(#23064,#23065,#23066,#23067,#23068,#23069,#23070,#23071,
#23072,#23073,#23074,#23075,#23076,#23077,#23078,#23079,#23080,#23081,#23082,
#23083,#23084,#23085,#23086,#23087,#23088,#23089,#23090,#23091,#23092,#23093,
#23094,#23095,#23096,#23097),(#23098,#23099,#23100,#23101,#23102,#23103,
#23104,#23105,#23106,#23107,#23108,#23109,#23110,#23111,#23112,#23113,#23114,
#23115,#23116,#23117,#23118,#23119,#23120,#23121,#23122,#23123,#23124,#23125,
#23126,#23127,#23128,#23129,#23130,#23131),(#23132,#23133,#23134,#23135,
#23136,#23137,#23138,#23139,#23140,#23141,#23142,#23143,#23144,#23145,#23146,
#23147,#23148,#23149,#23150,#23151,#23152,#23153,#23154,#23155,#23156,#23157,
#23158,#23159,#23160,#23161,#23162,#23163,#23164,#23165),(#23166,#23167,
#23168,#23169,#23170,#23171,#23172,#23173,#23174,#23175,#23176,#23177,#23178,
#23179,#23180,#23181,#23182,#23183,#23184,#23185,#23186,#23187,#23188,#23189,
#23190,#23191,#23192,#23193,#23194,#23195,#23196,#23197,#23198,#23199),
(#23200,#23201,#23202,#23203,#23204,#23205,#23206,#23207,#23208,#23209,
#23210,#23211,#23212,#23213,#23214,#23215,#23216,#23217,#23218,#23219,#23220,
#23221,#23222,#23223,#23224,#23225,#23226,#23227,#23228,#23229,#23230,#23231,
#23232,#23233)),.UNSPECIFIED.,.F.,.F.,.F.,(4,2,2,2,2,2,4),(4,2,2,2,2,2,
2,2,2,2,2,2,2,2,2,2,4),(-0.0123618863573116,0.,0.125,0.25,0.375,0.5,0.512361886357312),
(9.7389676693069,10.1395200046188,10.5400723399307,10.9406246752426,11.3411770105545,
11.7417293458665,12.1422816811784,12.5428340164903,12.9433863518022,13.3439386871141,
13.744491022426,14.1450433577379,14.5455956930498,14.9461480283618,15.3467003636736,
15.7472526989856,16.1478050342975),.UNSPECIFIED.);
#46=B_SPLINE_SURFACE_WITH_KNOTS('',3,3,((#23241,#23242,#23243,#23244,#23245,
#23246,#23247,#23248,#23249,#23250,#23251,#23252,#23253,#23254,#23255,#23256,
#23257,#23258,#23259,#23260,#23261,#23262,#23263,#23264,#23265,#23266,#23267,
#23268,#23269,#23270,#23271,#23272,#23273,#23274),(#23275,#23276,#23277,
#23278,#23279,#23280,#23281,#23282,#23283,#23284,#23285,#23286,#23287,#23288,
#23289,#23290,#23291,#23292,#23293,#23294,#23295,#23296,#23297,#23298,#23299,
#23300,#23301,#23302,#23303,#23304,#23305,#23306,#23307,#23308),(#23309,
#23310,#23311,#23312,#23313,#23314,#23315,#23316,#23317,#23318,#23319,#23320,
#23321,#23322,#23323,#23324,#23325,#23326,#23327,#23328,#23329,#23330,#23331,
#23332,#23333,#23334,#23335,#23336,#23337,#23338,#23339,#23340,#23341,#23342),
(#23343,#23344,#23345,#23346,#23347,#23348,#23349,#23350,#23351,#23352,
#23353,#23354,#23355,#23356,#23357,#23358,#23359,#23360,#23361,#23362,#23363,
#23364,#23365,#23366,#23367,#23368,#23369,#23370,#23371,#23372,#23373,#23374,
#23375,#23376),(#23377,#23378,#23379,#23380,#23381,#23382,#23383,#23384,
#23385,#23386,#23387,#23388,#23389,#23390,#23391,#23392,#23393,#23394,#23395,
#23396,#23397,#23398,#23399,#23400,#23401,#23402,#23403,#23404,#23405,#23406,
#23407,#23408,#23409,#23410),(#23411,#23412,#23413,#23414,#23415,#23416,
#23417,#23418,#23419,#23420,#23421,#23422,#23423,#23424,#23425,#23426,#23427,
#23428,#23429,#23430,#23431,#23432,#23433,#23434,#23435,#23436,#23437,#23438,
#23439,#23440,#23441,#23442,#23443,#23444),(#23445,#23446,#23447,#23448,
#23449,#23450,#23451,#23452,#23453,#23454,#23455,#23456,#23457,#23458,#23459,
#23460,#23461,#23462,#23463,#23464,#23465,#23466,#23467,#23468,#23469,#23470,
#23471,#23472,#23473,#23474,#23475,#23476,#23477,#23478),(#23479,#23480,
#23481,#23482,#23483,#23484,#23485,#23486,#23487,#23488,#23489,#23490,#23491,
#23492,#23493,#23494,#23495,#23496,#23497,#23498,#23499,#23500,#23501,#23502,
#23503,#23504,#23505,#23506,#23507,#23508,#23509,#23510,#23511,#23512),
(#23513,#23514,#23515,#23516,#23517,#23518,#23519,#23520,#23521,#23522,
#23523,#23524,#23525,#23526,#23527,#23528,#23529,#23530,#23531,#23532,#23533,
#23534,#23535,#23536,#23537,#23538,#23539,#23540,#23541,#23542,#23543,#23544,
#23545,#23546),(#23547,#23548,#23549,#23550,#23551,#23552,#23553,#23554,
#23555,#23556,#23557,#23558,#23559,#23560,#23561,#23562,#23563,#23564,#23565,
#23566,#23567,#23568,#23569,#23570,#23571,#23572,#23573,#23574,#23575,#23576,
#23577,#23578,#23579,#23580),(#23581,#23582,#23583,#23584,#23585,#23586,
#23587,#23588,#23589,#23590,#23591,#23592,#23593,#23594,#23595,#23596,#23597,
#23598,#23599,#23600,#23601,#23602,#23603,#23604,#23605,#23606,#23607,#23608,
#23609,#23610,#23611,#23612,#23613,#23614),(#23615,#23616,#23617,#23618,
#23619,#23620,#23621,#23622,#23623,#23624,#23625,#23626,#23627,#23628,#23629,
#23630,#23631,#23632,#23633,#23634,#23635,#23636,#23637,#23638,#23639,#23640,
#23641,#23642,#23643,#23644,#23645,#23646,#23647,#23648),(#23649,#23650,
#23651,#23652,#23653,#23654,#23655,#23656,#23657,#23658,#23659,#23660,#23661,
#23662,#23663,#23664,#23665,#23666,#23667,#23668,#23669,#23670,#23671,#23672,
#23673,#23674,#23675,#23676,#23677,#23678,#23679,#23680,#23681,#23682),
(#23683,#23684,#23685,#23686,#23687,#23688,#23689,#23690,#23691,#23692,
#23693,#23694,#23695,#23696,#23697,#23698,#23699,#23700,#23701,#23702,#23703,
#23704,#23705,#23706,#23707,#23708,#23709,#23710,#23711,#23712,#23713,#23714,
#23715,#23716),(#23717,#23718,#23719,#23720,#23721,#23722,#23723,#23724,
#23725,#23726,#23727,#23728,#23729,#23730,#23731,#23732,#23733,#23734,#23735,
#23736,#23737,#23738,#23739,#23740,#23741,#23742,#23743,#23744,#23745,#23746,
#23747,#23748,#23749,#23750),(#23751,#23752,#23753,#23754,#23755,#23756,
#23757,#23758,#23759,#23760,#23761,#23762,#23763,#23764,#23765,#23766,#23767,
#23768,#23769,#23770,#23771,#23772,#23773,#23774,#23775,#23776,#23777,#23778,
#23779,#23780,#23781,#23782,#23783,#23784)),.UNSPECIFIED.,.F.,.F.,.F.,(4,
2,2,2,2,2,2,4),(4,2,2,2,2,2,2,2,2,2,2,2,2,2,2,2,4),(-0.00300004903652835,
0.,0.1,0.2,0.3,0.4,0.5,0.50300004884616),(-0.00600030454937093,0.0450000000000826,
0.110000000000075,0.175000000000067,0.240000000000059,0.305000000000052,
0.370000000000045,0.435000000000037,0.500000000000029,0.565000000000022,
0.630000000000014,0.695,0.76,0.824999999999991,0.889999999999984,0.954999999999976,
1.00600015484898),.UNSPECIFIED.);
#47=B_SPLINE_SURFACE_WITH_KNOTS('',3,3,((#23792,#23793,#23794,#23795,#23796,
#23797,#23798,#23799,#23800,#23801,#23802,#23803,#23804,#23805,#23806,#23807,
#23808,#23809,#23810,#23811,#23812,#23813,#23814,#23815,#23816,#23817,#23818,
#23819,#23820,#23821,#23822,#23823,#23824,#23825),(#23826,#23827,#23828,
#23829,#23830,#23831,#23832,#23833,#23834,#23835,#23836,#23837,#23838,#23839,
#23840,#23841,#23842,#23843,#23844,#23845,#23846,#23847,#23848,#23849,#23850,
#23851,#23852,#23853,#23854,#23855,#23856,#23857,#23858,#23859),(#23860,
#23861,#23862,#23863,#23864,#23865,#23866,#23867,#23868,#23869,#23870,#23871,
#23872,#23873,#23874,#23875,#23876,#23877,#23878,#23879,#23880,#23881,#23882,
#23883,#23884,#23885,#23886,#23887,#23888,#23889,#23890,#23891,#23892,#23893),
(#23894,#23895,#23896,#23897,#23898,#23899,#23900,#23901,#23902,#23903,
#23904,#23905,#23906,#23907,#23908,#23909,#23910,#23911,#23912,#23913,#23914,
#23915,#23916,#23917,#23918,#23919,#23920,#23921,#23922,#23923,#23924,#23925,
#23926,#23927),(#23928,#23929,#23930,#23931,#23932,#23933,#23934,#23935,
#23936,#23937,#23938,#23939,#23940,#23941,#23942,#23943,#23944,#23945,#23946,
#23947,#23948,#23949,#23950,#23951,#23952,#23953,#23954,#23955,#23956,#23957,
#23958,#23959,#23960,#23961),(#23962,#23963,#23964,#23965,#23966,#23967,
#23968,#23969,#23970,#23971,#23972,#23973,#23974,#23975,#23976,#23977,#23978,
#23979,#23980,#23981,#23982,#23983,#23984,#23985,#23986,#23987,#23988,#23989,
#23990,#23991,#23992,#23993,#23994,#23995),(#23996,#23997,#23998,#23999,
#24000,#24001,#24002,#24003,#24004,#24005,#24006,#24007,#24008,#24009,#24010,
#24011,#24012,#24013,#24014,#24015,#24016,#24017,#24018,#24019,#24020,#24021,
#24022,#24023,#24024,#24025,#24026,#24027,#24028,#24029),(#24030,#24031,
#24032,#24033,#24034,#24035,#24036,#24037,#24038,#24039,#24040,#24041,#24042,
#24043,#24044,#24045,#24046,#24047,#24048,#24049,#24050,#24051,#24052,#24053,
#24054,#24055,#24056,#24057,#24058,#24059,#24060,#24061,#24062,#24063),
(#24064,#24065,#24066,#24067,#24068,#24069,#24070,#24071,#24072,#24073,
#24074,#24075,#24076,#24077,#24078,#24079,#24080,#24081,#24082,#24083,#24084,
#24085,#24086,#24087,#24088,#24089,#24090,#24091,#24092,#24093,#24094,#24095,
#24096,#24097),(#24098,#24099,#24100,#24101,#24102,#24103,#24104,#24105,
#24106,#24107,#24108,#24109,#24110,#24111,#24112,#24113,#24114,#24115,#24116,
#24117,#24118,#24119,#24120,#24121,#24122,#24123,#24124,#24125,#24126,#24127,
#24128,#24129,#24130,#24131),(#24132,#24133,#24134,#24135,#24136,#24137,
#24138,#24139,#24140,#24141,#24142,#24143,#24144,#24145,#24146,#24147,#24148,
#24149,#24150,#24151,#24152,#24153,#24154,#24155,#24156,#24157,#24158,#24159,
#24160,#24161,#24162,#24163,#24164,#24165),(#24166,#24167,#24168,#24169,
#24170,#24171,#24172,#24173,#24174,#24175,#24176,#24177,#24178,#24179,#24180,
#24181,#24182,#24183,#24184,#24185,#24186,#24187,#24188,#24189,#24190,#24191,
#24192,#24193,#24194,#24195,#24196,#24197,#24198,#24199),(#24200,#24201,
#24202,#24203,#24204,#24205,#24206,#24207,#24208,#24209,#24210,#24211,#24212,
#24213,#24214,#24215,#24216,#24217,#24218,#24219,#24220,#24221,#24222,#24223,
#24224,#24225,#24226,#24227,#24228,#24229,#24230,#24231,#24232,#24233),
(#24234,#24235,#24236,#24237,#24238,#24239,#24240,#24241,#24242,#24243,
#24244,#24245,#24246,#24247,#24248,#24249,#24250,#24251,#24252,#24253,#24254,
#24255,#24256,#24257,#24258,#24259,#24260,#24261,#24262,#24263,#24264,#24265,
#24266,#24267),(#24268,#24269,#24270,#24271,#24272,#24273,#24274,#24275,
#24276,#24277,#24278,#24279,#24280,#24281,#24282,#24283,#24284,#24285,#24286,
#24287,#24288,#24289,#24290,#24291,#24292,#24293,#24294,#24295,#24296,#24297,
#24298,#24299,#24300,#24301),(#24302,#24303,#24304,#24305,#24306,#24307,
#24308,#24309,#24310,#24311,#24312,#24313,#24314,#24315,#24316,#24317,#24318,
#24319,#24320,#24321,#24322,#24323,#24324,#24325,#24326,#24327,#24328,#24329,
#24330,#24331,#24332,#24333,#24334,#24335)),.UNSPECIFIED.,.F.,.F.,.F.,(4,
2,2,2,2,2,2,4),(4,2,2,2,2,2,2,2,2,2,2,2,2,2,2,2,4),(0.48765503023554,0.5,
0.6,0.7,0.8,0.9,1.,1.01234496976446),(9.7389676693069,10.1395200046188,
10.5400723399307,10.9406246752427,11.3411770105546,11.7417293458665,12.1422816811784,
12.5428340164903,12.9433863518023,13.3439386871142,13.7444910224261,14.145043357738,
14.5455956930499,14.9461480283619,15.3467003636738,15.7472526989857,16.1478050342977),
 .UNSPECIFIED.);
#48=B_SPLINE_SURFACE_WITH_KNOTS('',3,3,((#24367,#24368,#24369,#24370,#24371,
#24372,#24373,#24374,#24375,#24376,#24377,#24378,#24379,#24380,#24381,#24382,
#24383,#24384,#24385,#24386,#24387,#24388,#24389,#24390,#24391,#24392,#24393,
#24394,#24395,#24396,#24397,#24398,#24399,#24400),(#24401,#24402,#24403,
#24404,#24405,#24406,#24407,#24408,#24409,#24410,#24411,#24412,#24413,#24414,
#24415,#24416,#24417,#24418,#24419,#24420,#24421,#24422,#24423,#24424,#24425,
#24426,#24427,#24428,#24429,#24430,#24431,#24432,#24433,#24434),(#24435,
#24436,#24437,#24438,#24439,#24440,#24441,#24442,#24443,#24444,#24445,#24446,
#24447,#24448,#24449,#24450,#24451,#24452,#24453,#24454,#24455,#24456,#24457,
#24458,#24459,#24460,#24461,#24462,#24463,#24464,#24465,#24466,#24467,#24468),
(#24469,#24470,#24471,#24472,#24473,#24474,#24475,#24476,#24477,#24478,
#24479,#24480,#24481,#24482,#24483,#24484,#24485,#24486,#24487,#24488,#24489,
#24490,#24491,#24492,#24493,#24494,#24495,#24496,#24497,#24498,#24499,#24500,
#24501,#24502),(#24503,#24504,#24505,#24506,#24507,#24508,#24509,#24510,
#24511,#24512,#24513,#24514,#24515,#24516,#24517,#24518,#24519,#24520,#24521,
#24522,#24523,#24524,#24525,#24526,#24527,#24528,#24529,#24530,#24531,#24532,
#24533,#24534,#24535,#24536),(#24537,#24538,#24539,#24540,#24541,#24542,
#24543,#24544,#24545,#24546,#24547,#24548,#24549,#24550,#24551,#24552,#24553,
#24554,#24555,#24556,#24557,#24558,#24559,#24560,#24561,#24562,#24563,#24564,
#24565,#24566,#24567,#24568,#24569,#24570),(#24571,#24572,#24573,#24574,
#24575,#24576,#24577,#24578,#24579,#24580,#24581,#24582,#24583,#24584,#24585,
#24586,#24587,#24588,#24589,#24590,#24591,#24592,#24593,#24594,#24595,#24596,
#24597,#24598,#24599,#24600,#24601,#24602,#24603,#24604),(#24605,#24606,
#24607,#24608,#24609,#24610,#24611,#24612,#24613,#24614,#24615,#24616,#24617,
#24618,#24619,#24620,#24621,#24622,#24623,#24624,#24625,#24626,#24627,#24628,
#24629,#24630,#24631,#24632,#24633,#24634,#24635,#24636,#24637,#24638),
(#24639,#24640,#24641,#24642,#24643,#24644,#24645,#24646,#24647,#24648,
#24649,#24650,#24651,#24652,#24653,#24654,#24655,#24656,#24657,#24658,#24659,
#24660,#24661,#24662,#24663,#24664,#24665,#24666,#24667,#24668,#24669,#24670,
#24671,#24672),(#24673,#24674,#24675,#24676,#24677,#24678,#24679,#24680,
#24681,#24682,#24683,#24684,#24685,#24686,#24687,#24688,#24689,#24690,#24691,
#24692,#24693,#24694,#24695,#24696,#24697,#24698,#24699,#24700,#24701,#24702,
#24703,#24704,#24705,#24706),(#24707,#24708,#24709,#24710,#24711,#24712,
#24713,#24714,#24715,#24716,#24717,#24718,#24719,#24720,#24721,#24722,#24723,
#24724,#24725,#24726,#24727,#24728,#24729,#24730,#24731,#24732,#24733,#24734,
#24735,#24736,#24737,#24738,#24739,#24740),(#24741,#24742,#24743,#24744,
#24745,#24746,#24747,#24748,#24749,#24750,#24751,#24752,#24753,#24754,#24755,
#24756,#24757,#24758,#24759,#24760,#24761,#24762,#24763,#24764,#24765,#24766,
#24767,#24768,#24769,#24770,#24771,#24772,#24773,#24774),(#24775,#24776,
#24777,#24778,#24779,#24780,#24781,#24782,#24783,#24784,#24785,#24786,#24787,
#24788,#24789,#24790,#24791,#24792,#24793,#24794,#24795,#24796,#24797,#24798,
#24799,#24800,#24801,#24802,#24803,#24804,#24805,#24806,#24807,#24808),
(#24809,#24810,#24811,#24812,#24813,#24814,#24815,#24816,#24817,#24818,
#24819,#24820,#24821,#24822,#24823,#24824,#24825,#24826,#24827,#24828,#24829,
#24830,#24831,#24832,#24833,#24834,#24835,#24836,#24837,#24838,#24839,#24840,
#24841,#24842)),.UNSPECIFIED.,.F.,.F.,.F.,(4,2,2,2,2,2,4),(4,2,2,2,2,2,
2,2,2,2,2,2,2,2,2,2,4),(0.496998870686259,0.5,0.625,0.75,0.875,1.,1.0030011270394),
(-0.00600170187786821,0.045,0.11,0.175,0.24,0.305,0.37,0.435,0.5,0.565,
0.63,0.695,0.76,0.825,0.89,0.955,1.00600177391382),.UNSPECIFIED.);
#49=B_SPLINE_SURFACE_WITH_KNOTS('',3,3,((#24890,#24891,#24892,#24893,#24894,
#24895,#24896,#24897,#24898,#24899,#24900,#24901,#24902,#24903,#24904,#24905,
#24906,#24907,#24908,#24909,#24910,#24911,#24912,#24913,#24914,#24915,#24916,
#24917,#24918,#24919,#24920,#24921,#24922,#24923),(#24924,#24925,#24926,
#24927,#24928,#24929,#24930,#24931,#24932,#24933,#24934,#24935,#24936,#24937,
#24938,#24939,#24940,#24941,#24942,#24943,#24944,#24945,#24946,#24947,#24948,
#24949,#24950,#24951,#24952,#24953,#24954,#24955,#24956,#24957),(#24958,
#24959,#24960,#24961,#24962,#24963,#24964,#24965,#24966,#24967,#24968,#24969,
#24970,#24971,#24972,#24973,#24974,#24975,#24976,#24977,#24978,#24979,#24980,
#24981,#24982,#24983,#24984,#24985,#24986,#24987,#24988,#24989,#24990,#24991),
(#24992,#24993,#24994,#24995,#24996,#24997,#24998,#24999,#25000,#25001,
#25002,#25003,#25004,#25005,#25006,#25007,#25008,#25009,#25010,#25011,#25012,
#25013,#25014,#25015,#25016,#25017,#25018,#25019,#25020,#25021,#25022,#25023,
#25024,#25025),(#25026,#25027,#25028,#25029,#25030,#25031,#25032,#25033,
#25034,#25035,#25036,#25037,#25038,#25039,#25040,#25041,#25042,#25043,#25044,
#25045,#25046,#25047,#25048,#25049,#25050,#25051,#25052,#25053,#25054,#25055,
#25056,#25057,#25058,#25059),(#25060,#25061,#25062,#25063,#25064,#25065,
#25066,#25067,#25068,#25069,#25070,#25071,#25072,#25073,#25074,#25075,#25076,
#25077,#25078,#25079,#25080,#25081,#25082,#25083,#25084,#25085,#25086,#25087,
#25088,#25089,#25090,#25091,#25092,#25093),(#25094,#25095,#25096,#25097,
#25098,#25099,#25100,#25101,#25102,#25103,#25104,#25105,#25106,#25107,#25108,
#25109,#25110,#25111,#25112,#25113,#25114,#25115,#25116,#25117,#25118,#25119,
#25120,#25121,#25122,#25123,#25124,#25125,#25126,#25127),(#25128,#25129,
#25130,#25131,#25132,#25133,#25134,#25135,#25136,#25137,#25138,#25139,#25140,
#25141,#25142,#25143,#25144,#25145,#25146,#25147,#25148,#25149,#25150,#25151,
#25152,#25153,#25154,#25155,#25156,#25157,#25158,#25159,#25160,#25161),
(#25162,#25163,#25164,#25165,#25166,#25167,#25168,#25169,#25170,#25171,
#25172,#25173,#25174,#25175,#25176,#25177,#25178,#25179,#25180,#25181,#25182,
#25183,#25184,#25185,#25186,#25187,#25188,#25189,#25190,#25191,#25192,#25193,
#25194,#25195),(#25196,#25197,#25198,#25199,#25200,#25201,#25202,#25203,
#25204,#25205,#25206,#25207,#25208,#25209,#25210,#25211,#25212,#25213,#25214,
#25215,#25216,#25217,#25218,#25219,#25220,#25221,#25222,#25223,#25224,#25225,
#25226,#25227,#25228,#25229),(#25230,#25231,#25232,#25233,#25234,#25235,
#25236,#25237,#25238,#25239,#25240,#25241,#25242,#25243,#25244,#25245,#25246,
#25247,#25248,#25249,#25250,#25251,#25252,#25253,#25254,#25255,#25256,#25257,
#25258,#25259,#25260,#25261,#25262,#25263),(#25264,#25265,#25266,#25267,
#25268,#25269,#25270,#25271,#25272,#25273,#25274,#25275,#25276,#25277,#25278,
#25279,#25280,#25281,#25282,#25283,#25284,#25285,#25286,#25287,#25288,#25289,
#25290,#25291,#25292,#25293,#25294,#25295,#25296,#25297),(#25298,#25299,
#25300,#25301,#25302,#25303,#25304,#25305,#25306,#25307,#25308,#25309,#25310,
#25311,#25312,#25313,#25314,#25315,#25316,#25317,#25318,#25319,#25320,#25321,
#25322,#25323,#25324,#25325,#25326,#25327,#25328,#25329,#25330,#25331),
(#25332,#25333,#25334,#25335,#25336,#25337,#25338,#25339,#25340,#25341,
#25342,#25343,#25344,#25345,#25346,#25347,#25348,#25349,#25350,#25351,#25352,
#25353,#25354,#25355,#25356,#25357,#25358,#25359,#25360,#25361,#25362,#25363,
#25364,#25365)),.UNSPECIFIED.,.F.,.F.,.F.,(4,2,2,2,2,2,4),(4,2,2,2,2,2,
2,2,2,2,2,2,2,2,2,2,4),(-0.0030068551580675,0.,0.125,0.25,0.375,0.5,0.503006855154615),
(-0.00600170280327224,0.045,0.11,0.175,0.24,0.305,0.37,0.435,0.5,0.565,
0.63,0.695,0.76,0.825,0.89,0.955,1.00000190754036),.UNSPECIFIED.);
#50=B_SPLINE_SURFACE_WITH_KNOTS('',3,3,((#25373,#25374,#25375,#25376,#25377,
#25378,#25379,#25380,#25381,#25382,#25383,#25384,#25385,#25386,#25387,#25388,
#25389,#25390,#25391,#25392,#25393,#25394,#25395,#25396,#25397,#25398,#25399,
#25400,#25401,#25402,#25403,#25404,#25405,#25406),(#25407,#25408,#25409,
#25410,#25411,#25412,#25413,#25414,#25415,#25416,#25417,#25418,#25419,#25420,
#25421,#25422,#25423,#25424,#25425,#25426,#25427,#25428,#25429,#25430,#25431,
#25432,#25433,#25434,#25435,#25436,#25437,#25438,#25439,#25440),(#25441,
#25442,#25443,#25444,#25445,#25446,#25447,#25448,#25449,#25450,#25451,#25452,
#25453,#25454,#25455,#25456,#25457,#25458,#25459,#25460,#25461,#25462,#25463,
#25464,#25465,#25466,#25467,#25468,#25469,#25470,#25471,#25472,#25473,#25474),
(#25475,#25476,#25477,#25478,#25479,#25480,#25481,#25482,#25483,#25484,
#25485,#25486,#25487,#25488,#25489,#25490,#25491,#25492,#25493,#25494,#25495,
#25496,#25497,#25498,#25499,#25500,#25501,#25502,#25503,#25504,#25505,#25506,
#25507,#25508),(#25509,#25510,#25511,#25512,#25513,#25514,#25515,#25516,
#25517,#25518,#25519,#25520,#25521,#25522,#25523,#25524,#25525,#25526,#25527,
#25528,#25529,#25530,#25531,#25532,#25533,#25534,#25535,#25536,#25537,#25538,
#25539,#25540,#25541,#25542),(#25543,#25544,#25545,#25546,#25547,#25548,
#25549,#25550,#25551,#25552,#25553,#25554,#25555,#25556,#25557,#25558,#25559,
#25560,#25561,#25562,#25563,#25564,#25565,#25566,#25567,#25568,#25569,#25570,
#25571,#25572,#25573,#25574,#25575,#25576),(#25577,#25578,#25579,#25580,
#25581,#25582,#25583,#25584,#25585,#25586,#25587,#25588,#25589,#25590,#25591,
#25592,#25593,#25594,#25595,#25596,#25597,#25598,#25599,#25600,#25601,#25602,
#25603,#25604,#25605,#25606,#25607,#25608,#25609,#25610),(#25611,#25612,
#25613,#25614,#25615,#25616,#25617,#25618,#25619,#25620,#25621,#25622,#25623,
#25624,#25625,#25626,#25627,#25628,#25629,#25630,#25631,#25632,#25633,#25634,
#25635,#25636,#25637,#25638,#25639,#25640,#25641,#25642,#25643,#25644),
(#25645,#25646,#25647,#25648,#25649,#25650,#25651,#25652,#25653,#25654,
#25655,#25656,#25657,#25658,#25659,#25660,#25661,#25662,#25663,#25664,#25665,
#25666,#25667,#25668,#25669,#25670,#25671,#25672,#25673,#25674,#25675,#25676,
#25677,#25678),(#25679,#25680,#25681,#25682,#25683,#25684,#25685,#25686,
#25687,#25688,#25689,#25690,#25691,#25692,#25693,#25694,#25695,#25696,#25697,
#25698,#25699,#25700,#25701,#25702,#25703,#25704,#25705,#25706,#25707,#25708,
#25709,#25710,#25711,#25712),(#25713,#25714,#25715,#25716,#25717,#25718,
#25719,#25720,#25721,#25722,#25723,#25724,#25725,#25726,#25727,#25728,#25729,
#25730,#25731,#25732,#25733,#25734,#25735,#25736,#25737,#25738,#25739,#25740,
#25741,#25742,#25743,#25744,#25745,#25746),(#25747,#25748,#25749,#25750,
#25751,#25752,#25753,#25754,#25755,#25756,#25757,#25758,#25759,#25760,#25761,
#25762,#25763,#25764,#25765,#25766,#25767,#25768,#25769,#25770,#25771,#25772,
#25773,#25774,#25775,#25776,#25777,#25778,#25779,#25780),(#25781,#25782,
#25783,#25784,#25785,#25786,#25787,#25788,#25789,#25790,#25791,#25792,#25793,
#25794,#25795,#25796,#25797,#25798,#25799,#25800,#25801,#25802,#25803,#25804,
#25805,#25806,#25807,#25808,#25809,#25810,#25811,#25812,#25813,#25814),
(#25815,#25816,#25817,#25818,#25819,#25820,#25821,#25822,#25823,#25824,
#25825,#25826,#25827,#25828,#25829,#25830,#25831,#25832,#25833,#25834,#25835,
#25836,#25837,#25838,#25839,#25840,#25841,#25842,#25843,#25844,#25845,#25846,
#25847,#25848),(#25849,#25850,#25851,#25852,#25853,#25854,#25855,#25856,
#25857,#25858,#25859,#25860,#25861,#25862,#25863,#25864,#25865,#25866,#25867,
#25868,#25869,#25870,#25871,#25872,#25873,#25874,#25875,#25876,#25877,#25878,
#25879,#25880,#25881,#25882),(#25883,#25884,#25885,#25886,#25887,#25888,
#25889,#25890,#25891,#25892,#25893,#25894,#25895,#25896,#25897,#25898,#25899,
#25900,#25901,#25902,#25903,#25904,#25905,#25906,#25907,#25908,#25909,#25910,
#25911,#25912,#25913,#25914,#25915,#25916)),.UNSPECIFIED.,.F.,.F.,.F.,(4,
2,2,2,2,2,2,4),(4,2,2,2,2,2,2,2,2,2,2,2,2,2,2,2,4),(-0.0123449697644626,
0.,0.1,0.2,0.3,0.4,0.5,0.512344969764463),(9.7389676693069,10.1395200046188,
10.5400723399307,10.9406246752427,11.3411770105546,11.7417293458665,12.1422816811784,
12.5428340164903,12.9433863518023,13.3439386871142,13.7444910224261,14.145043357738,
14.5455956930499,14.9461480283619,15.3467003636738,15.7472526989857,16.1478050342977),
 .UNSPECIFIED.);
#51=B_SPLINE_SURFACE_WITH_KNOTS('',3,3,((#25924,#25925,#25926,#25927,#25928,
#25929,#25930,#25931,#25932,#25933,#25934,#25935,#25936,#25937,#25938,#25939,
#25940,#25941,#25942,#25943,#25944,#25945,#25946,#25947,#25948,#25949,#25950,
#25951,#25952,#25953,#25954,#25955,#25956,#25957),(#25958,#25959,#25960,
#25961,#25962,#25963,#25964,#25965,#25966,#25967,#25968,#25969,#25970,#25971,
#25972,#25973,#25974,#25975,#25976,#25977,#25978,#25979,#25980,#25981,#25982,
#25983,#25984,#25985,#25986,#25987,#25988,#25989,#25990,#25991),(#25992,
#25993,#25994,#25995,#25996,#25997,#25998,#25999,#26000,#26001,#26002,#26003,
#26004,#26005,#26006,#26007,#26008,#26009,#26010,#26011,#26012,#26013,#26014,
#26015,#26016,#26017,#26018,#26019,#26020,#26021,#26022,#26023,#26024,#26025),
(#26026,#26027,#26028,#26029,#26030,#26031,#26032,#26033,#26034,#26035,
#26036,#26037,#26038,#26039,#26040,#26041,#26042,#26043,#26044,#26045,#26046,
#26047,#26048,#26049,#26050,#26051,#26052,#26053,#26054,#26055,#26056,#26057,
#26058,#26059),(#26060,#26061,#26062,#26063,#26064,#26065,#26066,#26067,
#26068,#26069,#26070,#26071,#26072,#26073,#26074,#26075,#26076,#26077,#26078,
#26079,#26080,#26081,#26082,#26083,#26084,#26085,#26086,#26087,#26088,#26089,
#26090,#26091,#26092,#26093),(#26094,#26095,#26096,#26097,#26098,#26099,
#26100,#26101,#26102,#26103,#26104,#26105,#26106,#26107,#26108,#26109,#26110,
#26111,#26112,#26113,#26114,#26115,#26116,#26117,#26118,#26119,#26120,#26121,
#26122,#26123,#26124,#26125,#26126,#26127),(#26128,#26129,#26130,#26131,
#26132,#26133,#26134,#26135,#26136,#26137,#26138,#26139,#26140,#26141,#26142,
#26143,#26144,#26145,#26146,#26147,#26148,#26149,#26150,#26151,#26152,#26153,
#26154,#26155,#26156,#26157,#26158,#26159,#26160,#26161),(#26162,#26163,
#26164,#26165,#26166,#26167,#26168,#26169,#26170,#26171,#26172,#26173,#26174,
#26175,#26176,#26177,#26178,#26179,#26180,#26181,#26182,#26183,#26184,#26185,
#26186,#26187,#26188,#26189,#26190,#26191,#26192,#26193,#26194,#26195),
(#26196,#26197,#26198,#26199,#26200,#26201,#26202,#26203,#26204,#26205,
#26206,#26207,#26208,#26209,#26210,#26211,#26212,#26213,#26214,#26215,#26216,
#26217,#26218,#26219,#26220,#26221,#26222,#26223,#26224,#26225,#26226,#26227,
#26228,#26229),(#26230,#26231,#26232,#26233,#26234,#26235,#26236,#26237,
#26238,#26239,#26240,#26241,#26242,#26243,#26244,#26245,#26246,#26247,#26248,
#26249,#26250,#26251,#26252,#26253,#26254,#26255,#26256,#26257,#26258,#26259,
#26260,#26261,#26262,#26263),(#26264,#26265,#26266,#26267,#26268,#26269,
#26270,#26271,#26272,#26273,#26274,#26275,#26276,#26277,#26278,#26279,#26280,
#26281,#26282,#26283,#26284,#26285,#26286,#26287,#26288,#26289,#26290,#26291,
#26292,#26293,#26294,#26295,#26296,#26297),(#26298,#26299,#26300,#26301,
#26302,#26303,#26304,#26305,#26306,#26307,#26308,#26309,#26310,#26311,#26312,
#26313,#26314,#26315,#26316,#26317,#26318,#26319,#26320,#26321,#26322,#26323,
#26324,#26325,#26326,#26327,#26328,#26329,#26330,#26331),(#26332,#26333,
#26334,#26335,#26336,#26337,#26338,#26339,#26340,#26341,#26342,#26343,#26344,
#26345,#26346,#26347,#26348,#26349,#26350,#26351,#26352,#26353,#26354,#26355,
#26356,#26357,#26358,#26359,#26360,#26361,#26362,#26363,#26364,#26365),
(#26366,#26367,#26368,#26369,#26370,#26371,#26372,#26373,#26374,#26375,
#26376,#26377,#26378,#26379,#26380,#26381,#26382,#26383,#26384,#26385,#26386,
#26387,#26388,#26389,#26390,#26391,#26392,#26393,#26394,#26395,#26396,#26397,
#26398,#26399),(#26400,#26401,#26402,#26403,#26404,#26405,#26406,#26407,
#26408,#26409,#26410,#26411,#26412,#26413,#26414,#26415,#26416,#26417,#26418,
#26419,#26420,#26421,#26422,#26423,#26424,#26425,#26426,#26427,#26428,#26429,
#26430,#26431,#26432,#26433),(#26434,#26435,#26436,#26437,#26438,#26439,
#26440,#26441,#26442,#26443,#26444,#26445,#26446,#26447,#26448,#26449,#26450,
#26451,#26452,#26453,#26454,#26455,#26456,#26457,#26458,#26459,#26460,#26461,
#26462,#26463,#26464,#26465,#26466,#26467)),.UNSPECIFIED.,.F.,.F.,.F.,(4,
2,2,2,2,2,2,4),(4,2,2,2,2,2,2,2,2,2,2,2,2,2,2,2,4),(0.496997718705871,0.5000000000048,
0.6,0.7,0.8,0.9,0.999999999995041,1.00300228129556),(-0.00600176935748849,
0.0449995022183333,0.109999536098761,0.174999569979189,0.239999603859616,
0.304999637740044,0.369999671620471,0.434999705500899,0.499999739381326,
0.564999773261754,0.629999807142181,0.694999841022609,0.759999874903037,
0.824999908783464,0.889999942663892,0.954999976544319,1.0000018983327),
 .UNSPECIFIED.);
#52=B_SPLINE_SURFACE_WITH_KNOTS('',3,3,((#26506,#26507,#26508,#26509,#26510,
#26511,#26512,#26513,#26514,#26515,#26516,#26517,#26518,#26519,#26520,#26521,
#26522,#26523,#26524,#26525,#26526,#26527,#26528,#26529,#26530,#26531,#26532,
#26533,#26534,#26535,#26536,#26537,#26538,#26539),(#26540,#26541,#26542,
#26543,#26544,#26545,#26546,#26547,#26548,#26549,#26550,#26551,#26552,#26553,
#26554,#26555,#26556,#26557,#26558,#26559,#26560,#26561,#26562,#26563,#26564,
#26565,#26566,#26567,#26568,#26569,#26570,#26571,#26572,#26573),(#26574,
#26575,#26576,#26577,#26578,#26579,#26580,#26581,#26582,#26583,#26584,#26585,
#26586,#26587,#26588,#26589,#26590,#26591,#26592,#26593,#26594,#26595,#26596,
#26597,#26598,#26599,#26600,#26601,#26602,#26603,#26604,#26605,#26606,#26607),
(#26608,#26609,#26610,#26611,#26612,#26613,#26614,#26615,#26616,#26617,
#26618,#26619,#26620,#26621,#26622,#26623,#26624,#26625,#26626,#26627,#26628,
#26629,#26630,#26631,#26632,#26633,#26634,#26635,#26636,#26637,#26638,#26639,
#26640,#26641),(#26642,#26643,#26644,#26645,#26646,#26647,#26648,#26649,
#26650,#26651,#26652,#26653,#26654,#26655,#26656,#26657,#26658,#26659,#26660,
#26661,#26662,#26663,#26664,#26665,#26666,#26667,#26668,#26669,#26670,#26671,
#26672,#26673,#26674,#26675),(#26676,#26677,#26678,#26679,#26680,#26681,
#26682,#26683,#26684,#26685,#26686,#26687,#26688,#26689,#26690,#26691,#26692,
#26693,#26694,#26695,#26696,#26697,#26698,#26699,#26700,#26701,#26702,#26703,
#26704,#26705,#26706,#26707,#26708,#26709),(#26710,#26711,#26712,#26713,
#26714,#26715,#26716,#26717,#26718,#26719,#26720,#26721,#26722,#26723,#26724,
#26725,#26726,#26727,#26728,#26729,#26730,#26731,#26732,#26733,#26734,#26735,
#26736,#26737,#26738,#26739,#26740,#26741,#26742,#26743),(#26744,#26745,
#26746,#26747,#26748,#26749,#26750,#26751,#26752,#26753,#26754,#26755,#26756,
#26757,#26758,#26759,#26760,#26761,#26762,#26763,#26764,#26765,#26766,#26767,
#26768,#26769,#26770,#26771,#26772,#26773,#26774,#26775,#26776,#26777),
(#26778,#26779,#26780,#26781,#26782,#26783,#26784,#26785,#26786,#26787,
#26788,#26789,#26790,#26791,#26792,#26793,#26794,#26795,#26796,#26797,#26798,
#26799,#26800,#26801,#26802,#26803,#26804,#26805,#26806,#26807,#26808,#26809,
#26810,#26811),(#26812,#26813,#26814,#26815,#26816,#26817,#26818,#26819,
#26820,#26821,#26822,#26823,#26824,#26825,#26826,#26827,#26828,#26829,#26830,
#26831,#26832,#26833,#26834,#26835,#26836,#26837,#26838,#26839,#26840,#26841,
#26842,#26843,#26844,#26845),(#26846,#26847,#26848,#26849,#26850,#26851,
#26852,#26853,#26854,#26855,#26856,#26857,#26858,#26859,#26860,#26861,#26862,
#26863,#26864,#26865,#26866,#26867,#26868,#26869,#26870,#26871,#26872,#26873,
#26874,#26875,#26876,#26877,#26878,#26879),(#26880,#26881,#26882,#26883,
#26884,#26885,#26886,#26887,#26888,#26889,#26890,#26891,#26892,#26893,#26894,
#26895,#26896,#26897,#26898,#26899,#26900,#26901,#26902,#26903,#26904,#26905,
#26906,#26907,#26908,#26909,#26910,#26911,#26912,#26913),(#26914,#26915,
#26916,#26917,#26918,#26919,#26920,#26921,#26922,#26923,#26924,#26925,#26926,
#26927,#26928,#26929,#26930,#26931,#26932,#26933,#26934,#26935,#26936,#26937,
#26938,#26939,#26940,#26941,#26942,#26943,#26944,#26945,#26946,#26947),
(#26948,#26949,#26950,#26951,#26952,#26953,#26954,#26955,#26956,#26957,
#26958,#26959,#26960,#26961,#26962,#26963,#26964,#26965,#26966,#26967,#26968,
#26969,#26970,#26971,#26972,#26973,#26974,#26975,#26976,#26977,#26978,#26979,
#26980,#26981),(#26982,#26983,#26984,#26985,#26986,#26987,#26988,#26989,
#26990,#26991,#26992,#26993,#26994,#26995,#26996,#26997,#26998,#26999,#27000,
#27001,#27002,#27003,#27004,#27005,#27006,#27007,#27008,#27009,#27010,#27011,
#27012,#27013,#27014,#27015),(#27016,#27017,#27018,#27019,#27020,#27021,
#27022,#27023,#27024,#27025,#27026,#27027,#27028,#27029,#27030,#27031,#27032,
#27033,#27034,#27035,#27036,#27037,#27038,#27039,#27040,#27041,#27042,#27043,
#27044,#27045,#27046,#27047,#27048,#27049)),.UNSPECIFIED.,.F.,.F.,.F.,(4,
2,2,2,2,2,2,4),(4,2,2,2,2,2,2,2,2,2,2,2,2,2,2,2,4),(-0.00300112884876056,
0.,0.1,0.2,0.3,0.4,0.500000000011615,0.503001344659739),(-0.00600176891874219,
0.0449987955440709,0.109998877522747,0.174998959501422,0.239999041480098,
0.304999123458774,0.36999920543745,0.434999287416126,0.499999369394802,
0.564999451373477,0.629999533352153,0.694999615330829,0.759999697309505,
0.824999779288181,0.889999861266856,0.954999943245532,1.00600178762734),
 .UNSPECIFIED.);
#53=B_SPLINE_SURFACE_WITH_KNOTS('',3,3,((#31219,#31220,#31221,#31222,#31223,
#31224,#31225,#31226,#31227,#31228,#31229,#31230,#31231,#31232,#31233,#31234,
#31235,#31236,#31237,#31238,#31239,#31240,#31241,#31242,#31243,#31244,#31245,
#31246,#31247,#31248,#31249,#31250,#31251,#31252,#31253,#31254,#31255,#31256,
#31257,#31258,#31259,#31260,#31261,#31262,#31263,#31264,#31265,#31266,#31267,
#31268,#31269,#31270,#31271,#31272,#31273,#31274,#31275,#31276),(#31277,
#31278,#31279,#31280,#31281,#31282,#31283,#31284,#31285,#31286,#31287,#31288,
#31289,#31290,#31291,#31292,#31293,#31294,#31295,#31296,#31297,#31298,#31299,
#31300,#31301,#31302,#31303,#31304,#31305,#31306,#31307,#31308,#31309,#31310,
#31311,#31312,#31313,#31314,#31315,#31316,#31317,#31318,#31319,#31320,#31321,
#31322,#31323,#31324,#31325,#31326,#31327,#31328,#31329,#31330,#31331,#31332,
#31333,#31334),(#31335,#31336,#31337,#31338,#31339,#31340,#31341,#31342,
#31343,#31344,#31345,#31346,#31347,#31348,#31349,#31350,#31351,#31352,#31353,
#31354,#31355,#31356,#31357,#31358,#31359,#31360,#31361,#31362,#31363,#31364,
#31365,#31366,#31367,#31368,#31369,#31370,#31371,#31372,#31373,#31374,#31375,
#31376,#31377,#31378,#31379,#31380,#31381,#31382,#31383,#31384,#31385,#31386,
#31387,#31388,#31389,#31390,#31391,#31392),(#31393,#31394,#31395,#31396,
#31397,#31398,#31399,#31400,#31401,#31402,#31403,#31404,#31405,#31406,#31407,
#31408,#31409,#31410,#31411,#31412,#31413,#31414,#31415,#31416,#31417,#31418,
#31419,#31420,#31421,#31422,#31423,#31424,#31425,#31426,#31427,#31428,#31429,
#31430,#31431,#31432,#31433,#31434,#31435,#31436,#31437,#31438,#31439,#31440,
#31441,#31442,#31443,#31444,#31445,#31446,#31447,#31448,#31449,#31450)),
 .UNSPECIFIED.,.F.,.F.,.F.,(4,4),(4,2,2,2,2,2,2,2,2,2,2,2,2,2,2,2,2,2,2,
2,2,2,2,2,2,2,2,2,4),(0.,1.),(0.,0.0259911760203312,0.0519823520406625,
0.0779735280609937,0.103964704081325,0.129955880101656,0.155947056121987,
0.181938232142319,0.20792940816265,0.233920584182981,0.259911760203312,
0.285902936223644,0.311894112243975,0.337885288264306,0.363876464284637,
0.389867640304969,0.4158588163253,0.441849992345631,0.467841168365962,0.493832344386293,
0.519823520406625,0.571805872447287,0.62378822448795,0.675770576528612,
0.727752928569275,0.779735280609937,0.805726456630268,0.818722044640434,
0.8317176326506),.UNSPECIFIED.);
#54=B_SPLINE_SURFACE_WITH_KNOTS('',3,3,((#33420,#33421,#33422,#33423,#33424,
#33425),(#33426,#33427,#33428,#33429,#33430,#33431),(#33432,#33433,#33434,
#33435,#33436,#33437),(#33438,#33439,#33440,#33441,#33442,#33443)),
 .UNSPECIFIED.,.F.,.F.,.F.,(4,4),(4,2,4),(-0.00600752213313948,1.),(0.796322545918902,
0.814827939626118,0.833333333333333),.UNSPECIFIED.);
#55=B_SPLINE_SURFACE_WITH_KNOTS('',3,3,((#40363,#40364,#40365,#40366,#40367,
#40368,#40369,#40370,#40371,#40372,#40373,#40374,#40375,#40376,#40377,#40378,
#40379,#40380,#40381,#40382,#40383,#40384,#40385,#40386,#40387,#40388,#40389,
#40390,#40391,#40392,#40393,#40394,#40395,#40396,#40397,#40398,#40399,#40400,
#40401,#40402,#40403,#40404,#40405,#40406,#40407,#40408,#40409,#40410,#40411,
#40412,#40413,#40414,#40415,#40416,#40417,#40418,#40419,#40420,#40421,#40422,
#40423,#40424,#40425,#40426,#40427,#40428,#40429,#40430,#40431,#40432,#40433,
#40434,#40435,#40436,#40437,#40438,#40439,#40440,#40441,#40442,#40443,#40444,
#40445,#40446,#40447,#40448,#40449,#40450,#40451,#40452,#40453,#40454,#40455,
#40456,#40457,#40458,#40459,#40460,#40461,#40462,#40463,#40464,#40465,#40466,
#40467,#40468,#40469,#40470,#40471,#40472,#40473,#40474,#40475,#40476),
(#40477,#40478,#40479,#40480,#40481,#40482,#40483,#40484,#40485,#40486,
#40487,#40488,#40489,#40490,#40491,#40492,#40493,#40494,#40495,#40496,#40497,
#40498,#40499,#40500,#40501,#40502,#40503,#40504,#40505,#40506,#40507,#40508,
#40509,#40510,#40511,#40512,#40513,#40514,#40515,#40516,#40517,#40518,#40519,
#40520,#40521,#40522,#40523,#40524,#40525,#40526,#40527,#40528,#40529,#40530,
#40531,#40532,#40533,#40534,#40535,#40536,#40537,#40538,#40539,#40540,#40541,
#40542,#40543,#40544,#40545,#40546,#40547,#40548,#40549,#40550,#40551,#40552,
#40553,#40554,#40555,#40556,#40557,#40558,#40559,#40560,#40561,#40562,#40563,
#40564,#40565,#40566,#40567,#40568,#40569,#40570,#40571,#40572,#40573,#40574,
#40575,#40576,#40577,#40578,#40579,#40580,#40581,#40582,#40583,#40584,#40585,
#40586,#40587,#40588,#40589,#40590),(#40591,#40592,#40593,#40594,#40595,
#40596,#40597,#40598,#40599,#40600,#40601,#40602,#40603,#40604,#40605,#40606,
#40607,#40608,#40609,#40610,#40611,#40612,#40613,#40614,#40615,#40616,#40617,
#40618,#40619,#40620,#40621,#40622,#40623,#40624,#40625,#40626,#40627,#40628,
#40629,#40630,#40631,#40632,#40633,#40634,#40635,#40636,#40637,#40638,#40639,
#40640,#40641,#40642,#40643,#40644,#40645,#40646,#40647,#40648,#40649,#40650,
#40651,#40652,#40653,#40654,#40655,#40656,#40657,#40658,#40659,#40660,#40661,
#40662,#40663,#40664,#40665,#40666,#40667,#40668,#40669,#40670,#40671,#40672,
#40673,#40674,#40675,#40676,#40677,#40678,#40679,#40680,#40681,#40682,#40683,
#40684,#40685,#40686,#40687,#40688,#40689,#40690,#40691,#40692,#40693,#40694,
#40695,#40696,#40697,#40698,#40699,#40700,#40701,#40702,#40703,#40704),
(#40705,#40706,#40707,#40708,#40709,#40710,#40711,#40712,#40713,#40714,
#40715,#40716,#40717,#40718,#40719,#40720,#40721,#40722,#40723,#40724,#40725,
#40726,#40727,#40728,#40729,#40730,#40731,#40732,#40733,#40734,#40735,#40736,
#40737,#40738,#40739,#40740,#40741,#40742,#40743,#40744,#40745,#40746,#40747,
#40748,#40749,#40750,#40751,#40752,#40753,#40754,#40755,#40756,#40757,#40758,
#40759,#40760,#40761,#40762,#40763,#40764,#40765,#40766,#40767,#40768,#40769,
#40770,#40771,#40772,#40773,#40774,#40775,#40776,#40777,#40778,#40779,#40780,
#40781,#40782,#40783,#40784,#40785,#40786,#40787,#40788,#40789,#40790,#40791,
#40792,#40793,#40794,#40795,#40796,#40797,#40798,#40799,#40800,#40801,#40802,
#40803,#40804,#40805,#40806,#40807,#40808,#40809,#40810,#40811,#40812,#40813,
#40814,#40815,#40816,#40817,#40818)),.UNSPECIFIED.,.F.,.F.,.F.,(4,4),(4,
2,2,2,2,2,2,2,2,2,2,2,2,2,2,2,2,2,2,2,2,2,2,2,2,2,2,2,2,2,2,2,2,2,2,2,2,
2,2,2,2,2,2,2,2,2,2,2,2,2,2,2,2,2,2,2,4),(0.,1.),(0.,0.0151615249539755,
0.0303230499079509,0.0454845748619264,0.0606460998159018,0.0909691497238527,
0.106130674677828,0.121292199631804,0.136453724585779,0.151615249539755,
0.16677677449373,0.181938299447705,0.197099824401681,0.212261349355656,
0.242584399263607,0.257745924217583,0.272907449171558,0.303230499079509,
0.318392024033485,0.33355354898746,0.363876598895411,0.379038123849386,
0.394199648803362,0.409361173757337,0.424522698711313,0.439684223665288,
0.454845748619264,0.470007273573239,0.485168798527215,0.515491848435166,
0.530653373389141,0.545814898343116,0.560976423297092,0.576137948251067,
0.591299473205043,0.606460998159018,0.621622523112994,0.636784048066969,
0.66710709797492,0.682268622928896,0.697430147882871,0.727753197790822,
0.742914722744797,0.758076247698773,0.788399297606724,0.803560822560699,
0.818722347514675,0.83388387246865,0.849045397422626,0.864206922376601,
0.879368447330577,0.894529972284552,0.909691497238527,0.940014547146478,
0.955176072100454,0.962756834577442,0.970337597054429),.UNSPECIFIED.);
#56=B_SPLINE_SURFACE_WITH_KNOTS('',3,3,((#42010,#42011,#42012,#42013,#42014,
#42015),(#42016,#42017,#42018,#42019,#42020,#42021),(#42022,#42023,#42024,
#42025,#42026,#42027),(#42028,#42029,#42030,#42031,#42032,#42033),(#42034,
#42035,#42036,#42037,#42038,#42039),(#42040,#42041,#42042,#42043,#42044,
#42045),(#42046,#42047,#42048,#42049,#42050,#42051),(#42052,#42053,#42054,
#42055,#42056,#42057),(#42058,#42059,#42060,#42061,#42062,#42063),(#42064,
#42065,#42066,#42067,#42068,#42069)),.UNSPECIFIED.,.F.,.F.,.F.,(4,2,2,2,
4),(4,2,4),(0.000203480753469605,0.000266460935110171,0.000329441116750738,
0.000392421298391305,0.000455401480031871),(0.,0.503069799613008,1.00613959922602),
 .UNSPECIFIED.);
#57=B_SPLINE_SURFACE_WITH_KNOTS('',3,3,((#42215,#42216,#42217,#42218,#42219,
#42220),(#42221,#42222,#42223,#42224,#42225,#42226),(#42227,#42228,#42229,
#42230,#42231,#42232),(#42233,#42234,#42235,#42236,#42237,#42238),(#42239,
#42240,#42241,#42242,#42243,#42244),(#42245,#42246,#42247,#42248,#42249,
#42250)),.UNSPECIFIED.,.F.,.F.,.F.,(4,2,4),(4,2,4),(0.000210081613475223,
0.000328789525150644,0.000447497436826065),(-0.000133121398971735,0.499933439300514,
1.),.UNSPECIFIED.);
#58=B_SPLINE_SURFACE_WITH_KNOTS('',3,3,((#42325,#42326,#42327,#42328),(#42329,
#42330,#42331,#42332),(#42333,#42334,#42335,#42336),(#42337,#42338,#42339,
#42340),(#42341,#42342,#42343,#42344),(#42345,#42346,#42347,#42348),(#42349,
#42350,#42351,#42352),(#42353,#42354,#42355,#42356),(#42357,#42358,#42359,
#42360),(#42361,#42362,#42363,#42364),(#42365,#42366,#42367,#42368),(#42369,
#42370,#42371,#42372),(#42373,#42374,#42375,#42376),(#42377,#42378,#42379,
#42380),(#42381,#42382,#42383,#42384),(#42385,#42386,#42387,#42388),(#42389,
#42390,#42391,#42392),(#42393,#42394,#42395,#42396),(#42397,#42398,#42399,
#42400),(#42401,#42402,#42403,#42404),(#42405,#42406,#42407,#42408),(#42409,
#42410,#42411,#42412),(#42413,#42414,#42415,#42416),(#42417,#42418,#42419,
#42420),(#42421,#42422,#42423,#42424),(#42425,#42426,#42427,#42428),(#42429,
#42430,#42431,#42432),(#42433,#42434,#42435,#42436),(#42437,#42438,#42439,
#42440),(#42441,#42442,#42443,#42444),(#42445,#42446,#42447,#42448),(#42449,
#42450,#42451,#42452),(#42453,#42454,#42455,#42456),(#42457,#42458,#42459,
#42460),(#42461,#42462,#42463,#42464),(#42465,#42466,#42467,#42468),(#42469,
#42470,#42471,#42472),(#42473,#42474,#42475,#42476),(#42477,#42478,#42479,
#42480),(#42481,#42482,#42483,#42484),(#42485,#42486,#42487,#42488),(#42489,
#42490,#42491,#42492),(#42493,#42494,#42495,#42496),(#42497,#42498,#42499,
#42500),(#42501,#42502,#42503,#42504),(#42505,#42506,#42507,#42508),(#42509,
#42510,#42511,#42512),(#42513,#42514,#42515,#42516),(#42517,#42518,#42519,
#42520),(#42521,#42522,#42523,#42524),(#42525,#42526,#42527,#42528),(#42529,
#42530,#42531,#42532),(#42533,#42534,#42535,#42536),(#42537,#42538,#42539,
#42540),(#42541,#42542,#42543,#42544),(#42545,#42546,#42547,#42548),(#42549,
#42550,#42551,#42552),(#42553,#42554,#42555,#42556),(#42557,#42558,#42559,
#42560),(#42561,#42562,#42563,#42564),(#42565,#42566,#42567,#42568),(#42569,
#42570,#42571,#42572),(#42573,#42574,#42575,#42576),(#42577,#42578,#42579,
#42580),(#42581,#42582,#42583,#42584),(#42585,#42586,#42587,#42588),(#42589,
#42590,#42591,#42592),(#42593,#42594,#42595,#42596),(#42597,#42598,#42599,
#42600),(#42601,#42602,#42603,#42604),(#42605,#42606,#42607,#42608),(#42609,
#42610,#42611,#42612),(#42613,#42614,#42615,#42616),(#42617,#42618,#42619,
#42620),(#42621,#42622,#42623,#42624),(#42625,#42626,#42627,#42628),(#42629,
#42630,#42631,#42632),(#42633,#42634,#42635,#42636),(#42637,#42638,#42639,
#42640),(#42641,#42642,#42643,#42644),(#42645,#42646,#42647,#42648),(#42649,
#42650,#42651,#42652),(#42653,#42654,#42655,#42656),(#42657,#42658,#42659,
#42660),(#42661,#42662,#42663,#42664),(#42665,#42666,#42667,#42668),(#42669,
#42670,#42671,#42672),(#42673,#42674,#42675,#42676),(#42677,#42678,#42679,
#42680),(#42681,#42682,#42683,#42684),(#42685,#42686,#42687,#42688),(#42689,
#42690,#42691,#42692),(#42693,#42694,#42695,#42696),(#42697,#42698,#42699,
#42700),(#42701,#42702,#42703,#42704),(#42705,#42706,#42707,#42708),(#42709,
#42710,#42711,#42712),(#42713,#42714,#42715,#42716),(#42717,#42718,#42719,
#42720),(#42721,#42722,#42723,#42724),(#42725,#42726,#42727,#42728),(#42729,
#42730,#42731,#42732),(#42733,#42734,#42735,#42736),(#42737,#42738,#42739,
#42740),(#42741,#42742,#42743,#42744),(#42745,#42746,#42747,#42748),(#42749,
#42750,#42751,#42752),(#42753,#42754,#42755,#42756),(#42757,#42758,#42759,
#42760),(#42761,#42762,#42763,#42764),(#42765,#42766,#42767,#42768),(#42769,
#42770,#42771,#42772),(#42773,#42774,#42775,#42776),(#42777,#42778,#42779,
#42780),(#42781,#42782,#42783,#42784),(#42785,#42786,#42787,#42788),(#42789,
#42790,#42791,#42792),(#42793,#42794,#42795,#42796),(#42797,#42798,#42799,
#42800),(#42801,#42802,#42803,#42804),(#42805,#42806,#42807,#42808),(#42809,
#42810,#42811,#42812),(#42813,#42814,#42815,#42816),(#42817,#42818,#42819,
#42820),(#42821,#42822,#42823,#42824),(#42825,#42826,#42827,#42828),(#42829,
#42830,#42831,#42832),(#42833,#42834,#42835,#42836),(#42837,#42838,#42839,
#42840),(#42841,#42842,#42843,#42844),(#42845,#42846,#42847,#42848),(#42849,
#42850,#42851,#42852)),.UNSPECIFIED.,.F.,.F.,.F.,(4,2,2,2,2,2,2,2,2,2,2,
2,2,2,2,2,2,2,2,2,2,2,2,2,2,2,2,2,2,2,2,2,2,2,2,2,2,2,2,2,2,2,2,2,2,2,2,
2,2,2,2,2,2,2,2,2,2,2,2,2,2,2,2,2,2,4),(4,4),(0.202786906914899,0.208519922794762,
0.214252938674625,0.219985954554488,0.225718970434351,0.231451986314214,
0.237185002194077,0.24291801807394,0.248651033953804,0.254384049833667,
0.26011706571353,0.265850081593393,0.271583097473256,0.277316113353119,
0.283049129232982,0.288782145112846,0.294515160992709,0.300248176872572,
0.305981192752435,0.311714208632298,0.317447224512161,0.323180240392024,
0.328913256271887,0.334646272151751,0.340379288031614,0.346112303911477,
0.35184531979134,0.357578335671203,0.363311351551066,0.369044367430929,
0.374777383310793,0.380510399190656,0.386243415070519,0.391976430950382,
0.397709446830245,0.403442462710108,0.409175478589971,0.414908494469834,
0.420641510349698,0.426374526229561,0.432107542109424,0.437840557989287,
0.44357357386915,0.449306589749013,0.455039605628876,0.460772621508739,
0.466505637388603,0.472238653268466,0.477971669148329,0.483704685028192,
0.489437700908055,0.495170716787918,0.500903732667781,0.506636748547645,
0.512369764427508,0.518102780307371,0.523835796187234,0.529568812067097,
0.53530182794696,0.541034843826823,0.546767859706687,0.55250087558655,0.558233891466413,
0.563966907346276,0.566833415286207,0.569699923226139),(0.,1.00016823335214),
 .UNSPECIFIED.);
#59=B_SPLINE_SURFACE_WITH_KNOTS('',3,3,((#43571,#43572,#43573,#43574),(#43575,
#43576,#43577,#43578),(#43579,#43580,#43581,#43582),(#43583,#43584,#43585,
#43586),(#43587,#43588,#43589,#43590),(#43591,#43592,#43593,#43594),(#43595,
#43596,#43597,#43598),(#43599,#43600,#43601,#43602),(#43603,#43604,#43605,
#43606),(#43607,#43608,#43609,#43610),(#43611,#43612,#43613,#43614),(#43615,
#43616,#43617,#43618),(#43619,#43620,#43621,#43622),(#43623,#43624,#43625,
#43626),(#43627,#43628,#43629,#43630),(#43631,#43632,#43633,#43634),(#43635,
#43636,#43637,#43638),(#43639,#43640,#43641,#43642),(#43643,#43644,#43645,
#43646),(#43647,#43648,#43649,#43650),(#43651,#43652,#43653,#43654),(#43655,
#43656,#43657,#43658),(#43659,#43660,#43661,#43662),(#43663,#43664,#43665,
#43666),(#43667,#43668,#43669,#43670),(#43671,#43672,#43673,#43674),(#43675,
#43676,#43677,#43678),(#43679,#43680,#43681,#43682),(#43683,#43684,#43685,
#43686),(#43687,#43688,#43689,#43690),(#43691,#43692,#43693,#43694),(#43695,
#43696,#43697,#43698),(#43699,#43700,#43701,#43702),(#43703,#43704,#43705,
#43706),(#43707,#43708,#43709,#43710),(#43711,#43712,#43713,#43714),(#43715,
#43716,#43717,#43718),(#43719,#43720,#43721,#43722),(#43723,#43724,#43725,
#43726),(#43727,#43728,#43729,#43730),(#43731,#43732,#43733,#43734),(#43735,
#43736,#43737,#43738),(#43739,#43740,#43741,#43742),(#43743,#43744,#43745,
#43746),(#43747,#43748,#43749,#43750),(#43751,#43752,#43753,#43754),(#43755,
#43756,#43757,#43758),(#43759,#43760,#43761,#43762),(#43763,#43764,#43765,
#43766),(#43767,#43768,#43769,#43770),(#43771,#43772,#43773,#43774),(#43775,
#43776,#43777,#43778),(#43779,#43780,#43781,#43782),(#43783,#43784,#43785,
#43786),(#43787,#43788,#43789,#43790),(#43791,#43792,#43793,#43794),(#43795,
#43796,#43797,#43798),(#43799,#43800,#43801,#43802),(#43803,#43804,#43805,
#43806),(#43807,#43808,#43809,#43810),(#43811,#43812,#43813,#43814),(#43815,
#43816,#43817,#43818),(#43819,#43820,#43821,#43822),(#43823,#43824,#43825,
#43826),(#43827,#43828,#43829,#43830),(#43831,#43832,#43833,#43834),(#43835,
#43836,#43837,#43838),(#43839,#43840,#43841,#43842),(#43843,#43844,#43845,
#43846),(#43847,#43848,#43849,#43850),(#43851,#43852,#43853,#43854),(#43855,
#43856,#43857,#43858),(#43859,#43860,#43861,#43862),(#43863,#43864,#43865,
#43866),(#43867,#43868,#43869,#43870),(#43871,#43872,#43873,#43874),(#43875,
#43876,#43877,#43878),(#43879,#43880,#43881,#43882),(#43883,#43884,#43885,
#43886),(#43887,#43888,#43889,#43890),(#43891,#43892,#43893,#43894),(#43895,
#43896,#43897,#43898),(#43899,#43900,#43901,#43902),(#43903,#43904,#43905,
#43906),(#43907,#43908,#43909,#43910),(#43911,#43912,#43913,#43914),(#43915,
#43916,#43917,#43918),(#43919,#43920,#43921,#43922),(#43923,#43924,#43925,
#43926),(#43927,#43928,#43929,#43930),(#43931,#43932,#43933,#43934),(#43935,
#43936,#43937,#43938),(#43939,#43940,#43941,#43942),(#43943,#43944,#43945,
#43946),(#43947,#43948,#43949,#43950),(#43951,#43952,#43953,#43954),(#43955,
#43956,#43957,#43958),(#43959,#43960,#43961,#43962),(#43963,#43964,#43965,
#43966),(#43967,#43968,#43969,#43970),(#43971,#43972,#43973,#43974),(#43975,
#43976,#43977,#43978),(#43979,#43980,#43981,#43982),(#43983,#43984,#43985,
#43986),(#43987,#43988,#43989,#43990),(#43991,#43992,#43993,#43994),(#43995,
#43996,#43997,#43998),(#43999,#44000,#44001,#44002),(#44003,#44004,#44005,
#44006),(#44007,#44008,#44009,#44010),(#44011,#44012,#44013,#44014),(#44015,
#44016,#44017,#44018),(#44019,#44020,#44021,#44022),(#44023,#44024,#44025,
#44026),(#44027,#44028,#44029,#44030),(#44031,#44032,#44033,#44034),(#44035,
#44036,#44037,#44038),(#44039,#44040,#44041,#44042),(#44043,#44044,#44045,
#44046),(#44047,#44048,#44049,#44050),(#44051,#44052,#44053,#44054),(#44055,
#44056,#44057,#44058),(#44059,#44060,#44061,#44062),(#44063,#44064,#44065,
#44066),(#44067,#44068,#44069,#44070),(#44071,#44072,#44073,#44074),(#44075,
#44076,#44077,#44078),(#44079,#44080,#44081,#44082),(#44083,#44084,#44085,
#44086),(#44087,#44088,#44089,#44090),(#44091,#44092,#44093,#44094),(#44095,
#44096,#44097,#44098)),.UNSPECIFIED.,.F.,.F.,.F.,(4,2,2,2,2,2,2,2,2,2,2,
2,2,2,2,2,2,2,2,2,2,2,2,2,2,2,2,2,2,2,2,2,2,2,2,2,2,2,2,2,2,2,2,2,2,2,2,
2,2,2,2,2,2,2,2,2,2,2,2,2,2,2,2,2,2,4),(4,4),(0.202786898606437,0.208519914194954,
0.214252929783471,0.219985945371988,0.225718960960504,0.231451976549021,
0.237184992137538,0.242918007726055,0.248651023314571,0.254384038903088,
0.260117054491605,0.265850070080122,0.271583085668638,0.277316101257155,
0.283049116845672,0.288782132434189,0.294515148022705,0.300248163611222,
0.305981179199739,0.311714194788256,0.317447210376772,0.323180225965289,
0.328913241553806,0.334646257142323,0.340379272730839,0.346112288319356,
0.351845303907873,0.35757831949639,0.363311335084906,0.369044350673423,
0.37477736626194,0.380510381850457,0.386243397438973,0.39197641302749,0.397709428616007,
0.403442444204524,0.40917545979304,0.414908475381557,0.420641490970074,
0.42637450655859,0.432107522147107,0.437840537735624,0.443573553324141,
0.449306568912657,0.455039584501174,0.460772600089691,0.466505615678208,
0.472238631266724,0.477971646855241,0.483704662443758,0.489437678032275,
0.495170693620791,0.500903709209308,0.506636724797825,0.512369740386342,
0.518102755974858,0.523835771563375,0.529568787151892,0.535301802740409,
0.541034818328925,0.546767833917442,0.552500849505959,0.558233865094476,
0.563966880682992,0.566833388477251,0.569699896271509),(0.,1.00014725118256),
 .UNSPECIFIED.);
#60=COLOUR_RGB('', 0.66274510, 0.83137255, 0.94901961);
#61=COLOUR_RGB('', 0.31764706, 0.68627451, 0.89019608);
#62=COLOUR_RGB('', 0.09019608, 0.27058824, 0.51372549);
#63=COLOUR_RGB('', 0.08235294, 0.09019608, 0.10196078);
#64=COLOUR_RGB('', 0.31764706, 0.68627451, 0.89019608);
#65=CONTEXT_DEPENDENT_SHAPE_REPRESENTATION(#133,#45525);
#66=CONTEXT_DEPENDENT_SHAPE_REPRESENTATION(#134,#45527);
#67=CONTEXT_DEPENDENT_SHAPE_REPRESENTATION(#135,#45529);
#68=CONTEXT_DEPENDENT_SHAPE_REPRESENTATION(#136,#45531);
#69=CONTEXT_DEPENDENT_SHAPE_REPRESENTATION(#137,#45533);
#70=CONTEXT_DEPENDENT_SHAPE_REPRESENTATION(#138,#45535);
#71=CONTEXT_DEPENDENT_SHAPE_REPRESENTATION(#139,#45537);
#72=CONTEXT_DEPENDENT_SHAPE_REPRESENTATION(#140,#45538);
#73=CONTEXT_DEPENDENT_SHAPE_REPRESENTATION(#141,#45540);
#74=CONTEXT_DEPENDENT_SHAPE_REPRESENTATION(#142,#45541);
#75=CONTEXT_DEPENDENT_SHAPE_REPRESENTATION(#143,#45543);
#76=CONTEXT_DEPENDENT_SHAPE_REPRESENTATION(#144,#45545);
#77=CONTEXT_DEPENDENT_SHAPE_REPRESENTATION(#145,#45547);
#78=CONTEXT_DEPENDENT_SHAPE_REPRESENTATION(#146,#45549);
#79=CONTEXT_DEPENDENT_SHAPE_REPRESENTATION(#147,#45551);
#80=CONTEXT_DEPENDENT_SHAPE_REPRESENTATION(#148,#45553);
#81=CONTEXT_DEPENDENT_SHAPE_REPRESENTATION(#149,#45554);
#82=CONTEXT_DEPENDENT_SHAPE_REPRESENTATION(#150,#45556);
#83=CONTEXT_DEPENDENT_SHAPE_REPRESENTATION(#151,#45558);
#84=CONTEXT_DEPENDENT_SHAPE_REPRESENTATION(#152,#45560);
#85=CONTEXT_DEPENDENT_SHAPE_REPRESENTATION(#153,#45562);
#86=CONTEXT_DEPENDENT_SHAPE_REPRESENTATION(#154,#45563);
#87=CONTEXT_DEPENDENT_SHAPE_REPRESENTATION(#155,#45564);
#88=CONTEXT_DEPENDENT_SHAPE_REPRESENTATION(#156,#45566);
#89=CONTEXT_DEPENDENT_SHAPE_REPRESENTATION(#157,#45568);
#90=CONTEXT_DEPENDENT_SHAPE_REPRESENTATION(#158,#45570);
#91=CONTEXT_DEPENDENT_SHAPE_REPRESENTATION(#159,#45571);
#92=CONTEXT_DEPENDENT_SHAPE_REPRESENTATION(#160,#45573);
#93=CONTEXT_DEPENDENT_SHAPE_REPRESENTATION(#161,#45575);
#94=CONTEXT_DEPENDENT_SHAPE_REPRESENTATION(#162,#45576);
#95=CONTEXT_DEPENDENT_SHAPE_REPRESENTATION(#163,#45578);
#96=CONTEXT_DEPENDENT_SHAPE_REPRESENTATION(#164,#45580);
#97=CONTEXT_DEPENDENT_SHAPE_REPRESENTATION(#165,#45582);
#98=CONTEXT_DEPENDENT_SHAPE_REPRESENTATION(#166,#45584);
#99=NEXT_ASSEMBLY_USAGE_OCCURRENCE('NAUO1','Top_acces_nozzle_supporter',
'Top_acces_nozzle_supporter',#45585,#45586,'');
#100=NEXT_ASSEMBLY_USAGE_OCCURRENCE('NAUO2','piston','piston',#45585,#45587,
'');
#101=NEXT_ASSEMBLY_USAGE_OCCURRENCE('NAUO3','75632s_.prt','75632s_.prt',
#45585,#45588,'');
#102=NEXT_ASSEMBLY_USAGE_OCCURRENCE('NAUO4','refill_cap','refill_cap',#45585,
#45589,'');
#103=NEXT_ASSEMBLY_USAGE_OCCURRENCE('NAUO5','spring','spring',#45585,#45590,
'');
#104=NEXT_ASSEMBLY_USAGE_OCCURRENCE('NAUO6',
'floating_ring_bottom_connector','floating_ring_bottom_connector',#45585,
#45591,'');
#105=NEXT_ASSEMBLY_USAGE_OCCURRENCE('NAUO7',
'binding head screw_ai_CR-BHMS 0.099-48x0.25x0.25-N',
'binding head screw_ai_CR-BHMS 0.099-48x0.25x0.25-N',#45585,#45592,'');
#106=NEXT_ASSEMBLY_USAGE_OCCURRENCE('NAUO8',
'binding head screw_ai_CR-BHMS 0.099-48x0.25x0.25-N',
'binding head screw_ai_CR-BHMS 0.099-48x0.25x0.25-N',#45585,#45592,'');
#107=NEXT_ASSEMBLY_USAGE_OCCURRENCE('NAUO9','Floating_ring_guide',
'Floating_ring_guide',#45585,#45593,'');
#108=NEXT_ASSEMBLY_USAGE_OCCURRENCE('NAUO10',
'binding head screw_ai_CR-BHMS 0.099-48x0.25x0.25-N',
'binding head screw_ai_CR-BHMS 0.099-48x0.25x0.25-N',#45585,#45592,'');
#109=NEXT_ASSEMBLY_USAGE_OCCURRENCE('NAUO11','Bottle_Nech_Seal',
'Bottle_Nech_Seal',#45585,#45594,'');
#110=NEXT_ASSEMBLY_USAGE_OCCURRENCE('NAUO12','refill_cap','refill_cap',
#45585,#45595,'');
#111=NEXT_ASSEMBLY_USAGE_OCCURRENCE('NAUO13','main_housing',
'main_housing',#45585,#45596,'');
#112=NEXT_ASSEMBLY_USAGE_OCCURRENCE('NAUO14','Nozzle cap','Nozzle cap',
#45585,#45597,'');
#113=NEXT_ASSEMBLY_USAGE_OCCURRENCE('NAUO15','dip','dip',#45585,#45598,
'');
#114=NEXT_ASSEMBLY_USAGE_OCCURRENCE('NAUO16','Neck_flat_seal',
'Neck_flat_seal',#45585,#45599,'');
#115=NEXT_ASSEMBLY_USAGE_OCCURRENCE('NAUO17',
'binding head screw_ai_CR-BHMS 0.099-48x0.25x0.25-N',
'binding head screw_ai_CR-BHMS 0.099-48x0.25x0.25-N',#45585,#45592,'');
#116=NEXT_ASSEMBLY_USAGE_OCCURRENCE('NAUO18','refill_port',
'refill_port',#45585,#45600,'');
#117=NEXT_ASSEMBLY_USAGE_OCCURRENCE('NAUO19','ball_outlet_valve',
'ball_outlet_valve',#45585,#45601,'');
#118=NEXT_ASSEMBLY_USAGE_OCCURRENCE('NAUO20','Floating_ring',
'Floating_ring',#45585,#45602,'');
#119=NEXT_ASSEMBLY_USAGE_OCCURRENCE('NAUO21','ball','ball',#45585,#45603,
'');
#120=NEXT_ASSEMBLY_USAGE_OCCURRENCE('NAUO22',
'binding head screw_ai_CR-BHMS 0.099-48x0.25x0.25-N',
'binding head screw_ai_CR-BHMS 0.099-48x0.25x0.25-N',#45585,#45592,'');
#121=NEXT_ASSEMBLY_USAGE_OCCURRENCE('NAUO23','Floating_ring_guide',
'Floating_ring_guide',#45585,#45593,'');
#122=NEXT_ASSEMBLY_USAGE_OCCURRENCE('NAUO24','screw_cover',
'screw_cover',#45585,#45604,'');
#123=NEXT_ASSEMBLY_USAGE_OCCURRENCE('NAUO25','refill+port_air_seal',
'refill+port_air_seal',#45585,#45605,'');
#124=NEXT_ASSEMBLY_USAGE_OCCURRENCE('NAUO26','Bottle','Bottle',#45585,#45606,
'');
#125=NEXT_ASSEMBLY_USAGE_OCCURRENCE('NAUO27','Floating_ring_guide',
'Floating_ring_guide',#45585,#45593,'');
#126=NEXT_ASSEMBLY_USAGE_OCCURRENCE('NAUO28','bottle_premium_cover',
'bottle_premium_cover',#45585,#45607,'');
#127=NEXT_ASSEMBLY_USAGE_OCCURRENCE('NAUO29','refill_screw',
'refill_screw',#45585,#45608,'');
#128=NEXT_ASSEMBLY_USAGE_OCCURRENCE('NAUO30',
'binding head screw_ai_CR-BHMS 0.099-48x0.25x0.25-N',
'binding head screw_ai_CR-BHMS 0.099-48x0.25x0.25-N',#45585,#45592,'');
#129=NEXT_ASSEMBLY_USAGE_OCCURRENCE('NAUO31','refill_port',
'refill_port',#45585,#45609,'');
#130=NEXT_ASSEMBLY_USAGE_OCCURRENCE('NAUO32','ball_retainer',
'ball_retainer',#45585,#45610,'');
#131=NEXT_ASSEMBLY_USAGE_OCCURRENCE('NAUO33','Bottle_Cap','Bottle_Cap',
#45585,#45611,'');
#132=NEXT_ASSEMBLY_USAGE_OCCURRENCE('NAUO34','o_ring','o_ring',#45585,#45612,
'');
#133=(
REPRESENTATION_RELATIONSHIP(' ',' ',#13775,#13774)
REPRESENTATION_RELATIONSHIP_WITH_TRANSFORMATION(#167)
SHAPE_REPRESENTATION_RELATIONSHIP()
);
#134=(
REPRESENTATION_RELATIONSHIP(' ',' ',#13776,#13774)
REPRESENTATION_RELATIONSHIP_WITH_TRANSFORMATION(#168)
SHAPE_REPRESENTATION_RELATIONSHIP()
);
#135=(
REPRESENTATION_RELATIONSHIP(' ',' ',#13777,#13774)
REPRESENTATION_RELATIONSHIP_WITH_TRANSFORMATION(#169)
SHAPE_REPRESENTATION_RELATIONSHIP()
);
#136=(
REPRESENTATION_RELATIONSHIP(' ',' ',#13778,#13774)
REPRESENTATION_RELATIONSHIP_WITH_TRANSFORMATION(#170)
SHAPE_REPRESENTATION_RELATIONSHIP()
);
#137=(
REPRESENTATION_RELATIONSHIP(' ',' ',#13779,#13774)
REPRESENTATION_RELATIONSHIP_WITH_TRANSFORMATION(#171)
SHAPE_REPRESENTATION_RELATIONSHIP()
);
#138=(
REPRESENTATION_RELATIONSHIP(' ',' ',#13780,#13774)
REPRESENTATION_RELATIONSHIP_WITH_TRANSFORMATION(#172)
SHAPE_REPRESENTATION_RELATIONSHIP()
);
#139=(
REPRESENTATION_RELATIONSHIP(' ',' ',#13781,#13774)
REPRESENTATION_RELATIONSHIP_WITH_TRANSFORMATION(#173)
SHAPE_REPRESENTATION_RELATIONSHIP()
);
#140=(
REPRESENTATION_RELATIONSHIP(' ',' ',#13781,#13774)
REPRESENTATION_RELATIONSHIP_WITH_TRANSFORMATION(#174)
SHAPE_REPRESENTATION_RELATIONSHIP()
);
#141=(
REPRESENTATION_RELATIONSHIP(' ',' ',#13782,#13774)
REPRESENTATION_RELATIONSHIP_WITH_TRANSFORMATION(#175)
SHAPE_REPRESENTATION_RELATIONSHIP()
);
#142=(
REPRESENTATION_RELATIONSHIP(' ',' ',#13781,#13774)
REPRESENTATION_RELATIONSHIP_WITH_TRANSFORMATION(#176)
SHAPE_REPRESENTATION_RELATIONSHIP()
);
#143=(
REPRESENTATION_RELATIONSHIP(' ',' ',#13783,#13774)
REPRESENTATION_RELATIONSHIP_WITH_TRANSFORMATION(#177)
SHAPE_REPRESENTATION_RELATIONSHIP()
);
#144=(
REPRESENTATION_RELATIONSHIP(' ',' ',#13784,#13774)
REPRESENTATION_RELATIONSHIP_WITH_TRANSFORMATION(#178)
SHAPE_REPRESENTATION_RELATIONSHIP()
);
#145=(
REPRESENTATION_RELATIONSHIP(' ',' ',#13785,#13774)
REPRESENTATION_RELATIONSHIP_WITH_TRANSFORMATION(#179)
SHAPE_REPRESENTATION_RELATIONSHIP()
);
#146=(
REPRESENTATION_RELATIONSHIP(' ',' ',#13786,#13774)
REPRESENTATION_RELATIONSHIP_WITH_TRANSFORMATION(#180)
SHAPE_REPRESENTATION_RELATIONSHIP()
);
#147=(
REPRESENTATION_RELATIONSHIP(' ',' ',#13787,#13774)
REPRESENTATION_RELATIONSHIP_WITH_TRANSFORMATION(#181)
SHAPE_REPRESENTATION_RELATIONSHIP()
);
#148=(
REPRESENTATION_RELATIONSHIP(' ',' ',#13788,#13774)
REPRESENTATION_RELATIONSHIP_WITH_TRANSFORMATION(#182)
SHAPE_REPRESENTATION_RELATIONSHIP()
);
#149=(
REPRESENTATION_RELATIONSHIP(' ',' ',#13781,#13774)
REPRESENTATION_RELATIONSHIP_WITH_TRANSFORMATION(#183)
SHAPE_REPRESENTATION_RELATIONSHIP()
);
#150=(
REPRESENTATION_RELATIONSHIP(' ',' ',#13789,#13774)
REPRESENTATION_RELATIONSHIP_WITH_TRANSFORMATION(#184)
SHAPE_REPRESENTATION_RELATIONSHIP()
);
#151=(
REPRESENTATION_RELATIONSHIP(' ',' ',#13790,#13774)
REPRESENTATION_RELATIONSHIP_WITH_TRANSFORMATION(#185)
SHAPE_REPRESENTATION_RELATIONSHIP()
);
#152=(
REPRESENTATION_RELATIONSHIP(' ',' ',#13791,#13774)
REPRESENTATION_RELATIONSHIP_WITH_TRANSFORMATION(#186)
SHAPE_REPRESENTATION_RELATIONSHIP()
);
#153=(
REPRESENTATION_RELATIONSHIP(' ',' ',#13792,#13774)
REPRESENTATION_RELATIONSHIP_WITH_TRANSFORMATION(#187)
SHAPE_REPRESENTATION_RELATIONSHIP()
);
#154=(
REPRESENTATION_RELATIONSHIP(' ',' ',#13781,#13774)
REPRESENTATION_RELATIONSHIP_WITH_TRANSFORMATION(#188)
SHAPE_REPRESENTATION_RELATIONSHIP()
);
#155=(
REPRESENTATION_RELATIONSHIP(' ',' ',#13782,#13774)
REPRESENTATION_RELATIONSHIP_WITH_TRANSFORMATION(#189)
SHAPE_REPRESENTATION_RELATIONSHIP()
);
#156=(
REPRESENTATION_RELATIONSHIP(' ',' ',#13793,#13774)
REPRESENTATION_RELATIONSHIP_WITH_TRANSFORMATION(#190)
SHAPE_REPRESENTATION_RELATIONSHIP()
);
#157=(
REPRESENTATION_RELATIONSHIP(' ',' ',#13794,#13774)
REPRESENTATION_RELATIONSHIP_WITH_TRANSFORMATION(#191)
SHAPE_REPRESENTATION_RELATIONSHIP()
);
#158=(
REPRESENTATION_RELATIONSHIP(' ',' ',#13795,#13774)
REPRESENTATION_RELATIONSHIP_WITH_TRANSFORMATION(#192)
SHAPE_REPRESENTATION_RELATIONSHIP()
);
#159=(
REPRESENTATION_RELATIONSHIP(' ',' ',#13782,#13774)
REPRESENTATION_RELATIONSHIP_WITH_TRANSFORMATION(#193)
SHAPE_REPRESENTATION_RELATIONSHIP()
);
#160=(
REPRESENTATION_RELATIONSHIP(' ',' ',#13796,#13774)
REPRESENTATION_RELATIONSHIP_WITH_TRANSFORMATION(#194)
SHAPE_REPRESENTATION_RELATIONSHIP()
);
#161=(
REPRESENTATION_RELATIONSHIP(' ',' ',#13797,#13774)
REPRESENTATION_RELATIONSHIP_WITH_TRANSFORMATION(#195)
SHAPE_REPRESENTATION_RELATIONSHIP()
);
#162=(
REPRESENTATION_RELATIONSHIP(' ',' ',#13781,#13774)
REPRESENTATION_RELATIONSHIP_WITH_TRANSFORMATION(#196)
SHAPE_REPRESENTATION_RELATIONSHIP()
);
#163=(
REPRESENTATION_RELATIONSHIP(' ',' ',#13798,#13774)
REPRESENTATION_RELATIONSHIP_WITH_TRANSFORMATION(#197)
SHAPE_REPRESENTATION_RELATIONSHIP()
);
#164=(
REPRESENTATION_RELATIONSHIP(' ',' ',#13799,#13774)
REPRESENTATION_RELATIONSHIP_WITH_TRANSFORMATION(#198)
SHAPE_REPRESENTATION_RELATIONSHIP()
);
#165=(
REPRESENTATION_RELATIONSHIP(' ',' ',#13800,#13774)
REPRESENTATION_RELATIONSHIP_WITH_TRANSFORMATION(#199)
SHAPE_REPRESENTATION_RELATIONSHIP()
);
#166=(
REPRESENTATION_RELATIONSHIP(' ',' ',#13801,#13774)
REPRESENTATION_RELATIONSHIP_WITH_TRANSFORMATION(#200)
SHAPE_REPRESENTATION_RELATIONSHIP()
);
#167=ITEM_DEFINED_TRANSFORMATION(' ',' ',#13802,#13903);
#168=ITEM_DEFINED_TRANSFORMATION(' ',' ',#13802,#13985);
#169=ITEM_DEFINED_TRANSFORMATION(' ',' ',#13802,#13990);
#170=ITEM_DEFINED_TRANSFORMATION(' ',' ',#13802,#14003);
#171=ITEM_DEFINED_TRANSFORMATION(' ',' ',#13802,#14008);
#172=ITEM_DEFINED_TRANSFORMATION(' ',' ',#13802,#14225);
#173=ITEM_DEFINED_TRANSFORMATION(' ',' ',#13802,#14260);
#174=ITEM_DEFINED_TRANSFORMATION(' ',' ',#13802,#14261);
#175=ITEM_DEFINED_TRANSFORMATION(' ',' ',#13802,#14275);
#176=ITEM_DEFINED_TRANSFORMATION(' ',' ',#13802,#14276);
#177=ITEM_DEFINED_TRANSFORMATION(' ',' ',#13802,#14299);
#178=ITEM_DEFINED_TRANSFORMATION(' ',' ',#13802,#14334);
#179=ITEM_DEFINED_TRANSFORMATION(' ',' ',#13802,#14379);
#180=ITEM_DEFINED_TRANSFORMATION(' ',' ',#13802,#14641);
#181=ITEM_DEFINED_TRANSFORMATION(' ',' ',#13802,#14650);
#182=ITEM_DEFINED_TRANSFORMATION(' ',' ',#13802,#14659);
#183=ITEM_DEFINED_TRANSFORMATION(' ',' ',#13802,#14660);
#184=ITEM_DEFINED_TRANSFORMATION(' ',' ',#13802,#14696);
#185=ITEM_DEFINED_TRANSFORMATION(' ',' ',#13802,#14698);
#186=ITEM_DEFINED_TRANSFORMATION(' ',' ',#13802,#14760);
#187=ITEM_DEFINED_TRANSFORMATION(' ',' ',#13802,#14762);
#188=ITEM_DEFINED_TRANSFORMATION(' ',' ',#13802,#14763);
#189=ITEM_DEFINED_TRANSFORMATION(' ',' ',#13802,#14764);
#190=ITEM_DEFINED_TRANSFORMATION(' ',' ',#13802,#14800);
#191=ITEM_DEFINED_TRANSFORMATION(' ',' ',#13802,#14847);
#192=ITEM_DEFINED_TRANSFORMATION(' ',' ',#13802,#14999);
#193=ITEM_DEFINED_TRANSFORMATION(' ',' ',#13802,#15000);
#194=ITEM_DEFINED_TRANSFORMATION(' ',' ',#13802,#15048);
#195=ITEM_DEFINED_TRANSFORMATION(' ',' ',#13802,#15126);
#196=ITEM_DEFINED_TRANSFORMATION(' ',' ',#13802,#15127);
#197=ITEM_DEFINED_TRANSFORMATION(' ',' ',#13802,#15189);
#198=ITEM_DEFINED_TRANSFORMATION(' ',' ',#13802,#15258);
#199=ITEM_DEFINED_TRANSFORMATION(' ',' ',#13802,#15289);
#200=ITEM_DEFINED_TRANSFORMATION(' ',' ',#13802,#15294);
#201=SHAPE_REPRESENTATION_RELATIONSHIP('','',#13775,#228);
#202=SHAPE_REPRESENTATION_RELATIONSHIP('','',#13776,#229);
#203=SHAPE_REPRESENTATION_RELATIONSHIP('','',#13777,#230);
#204=SHAPE_REPRESENTATION_RELATIONSHIP('','',#13778,#231);
#205=SHAPE_REPRESENTATION_RELATIONSHIP('','',#13779,#232);
#206=SHAPE_REPRESENTATION_RELATIONSHIP('','',#13780,#233);
#207=SHAPE_REPRESENTATION_RELATIONSHIP('','',#13781,#234);
#208=SHAPE_REPRESENTATION_RELATIONSHIP('','',#13782,#235);
#209=SHAPE_REPRESENTATION_RELATIONSHIP('','',#13783,#236);
#210=SHAPE_REPRESENTATION_RELATIONSHIP('','',#13784,#237);
#211=SHAPE_REPRESENTATION_RELATIONSHIP('','',#13785,#238);
#212=SHAPE_REPRESENTATION_RELATIONSHIP('','',#13786,#239);
#213=SHAPE_REPRESENTATION_RELATIONSHIP('','',#13787,#240);
#214=SHAPE_REPRESENTATION_RELATIONSHIP('','',#13788,#241);
#215=SHAPE_REPRESENTATION_RELATIONSHIP('','',#13789,#242);
#216=SHAPE_REPRESENTATION_RELATIONSHIP('','',#13790,#243);
#217=SHAPE_REPRESENTATION_RELATIONSHIP('','',#13791,#244);
#218=SHAPE_REPRESENTATION_RELATIONSHIP('','',#13792,#245);
#219=SHAPE_REPRESENTATION_RELATIONSHIP('','',#13793,#246);
#220=SHAPE_REPRESENTATION_RELATIONSHIP('','',#13794,#247);
#221=SHAPE_REPRESENTATION_RELATIONSHIP('','',#13795,#248);
#222=SHAPE_REPRESENTATION_RELATIONSHIP('','',#13796,#249);
#223=SHAPE_REPRESENTATION_RELATIONSHIP('','',#13797,#250);
#224=SHAPE_REPRESENTATION_RELATIONSHIP('','',#13798,#251);
#225=SHAPE_REPRESENTATION_RELATIONSHIP('','',#13799,#252);
#226=SHAPE_REPRESENTATION_RELATIONSHIP('','',#13800,#253);
#227=SHAPE_REPRESENTATION_RELATIONSHIP('','',#13801,#254);
#228=ADVANCED_BREP_SHAPE_REPRESENTATION('',(#13719),#45465);
#229=ADVANCED_BREP_SHAPE_REPRESENTATION('',(#13720),#45466);
#230=ADVANCED_BREP_SHAPE_REPRESENTATION('',(#13721),#45467);
#231=ADVANCED_BREP_SHAPE_REPRESENTATION('',(#13722),#45468);
#232=ADVANCED_BREP_SHAPE_REPRESENTATION('',(#13723),#45469);
#233=ADVANCED_BREP_SHAPE_REPRESENTATION('',(#13724),#45470);
#234=ADVANCED_BREP_SHAPE_REPRESENTATION('',(#13725),#45471);
#235=ADVANCED_BREP_SHAPE_REPRESENTATION('',(#13726),#45472);
#236=ADVANCED_BREP_SHAPE_REPRESENTATION('',(#13727),#45473);
#237=ADVANCED_BREP_SHAPE_REPRESENTATION('',(#13728),#45474);
#238=ADVANCED_BREP_SHAPE_REPRESENTATION('',(#13729),#45475);
#239=ADVANCED_BREP_SHAPE_REPRESENTATION('',(#13730),#45476);
#240=ADVANCED_BREP_SHAPE_REPRESENTATION('',(#13731),#45477);
#241=ADVANCED_BREP_SHAPE_REPRESENTATION('',(#13732),#45478);
#242=ADVANCED_BREP_SHAPE_REPRESENTATION('',(#13733),#45479);
#243=ADVANCED_BREP_SHAPE_REPRESENTATION('',(#13734),#45480);
#244=ADVANCED_BREP_SHAPE_REPRESENTATION('',(#13735),#45481);
#245=ADVANCED_BREP_SHAPE_REPRESENTATION('',(#13736),#45482);
#246=ADVANCED_BREP_SHAPE_REPRESENTATION('',(#13737),#45483);
#247=ADVANCED_BREP_SHAPE_REPRESENTATION('',(#13738),#45484);
#248=ADVANCED_BREP_SHAPE_REPRESENTATION('',(#13739),#45485);
#249=ADVANCED_BREP_SHAPE_REPRESENTATION('',(#13740),#45486);
#250=ADVANCED_BREP_SHAPE_REPRESENTATION('',(#13741),#45487);
#251=ADVANCED_BREP_SHAPE_REPRESENTATION('',(#13742),#45488);
#252=ADVANCED_BREP_SHAPE_REPRESENTATION('',(#13743),#45489);
#253=ADVANCED_BREP_SHAPE_REPRESENTATION('',(#13744),#45490);
#254=ADVANCED_BREP_SHAPE_REPRESENTATION('',(#13745),#45491);
#255=TOROIDAL_SURFACE('',#13902,0.00555,0.001);
#256=TOROIDAL_SURFACE('',#13949,0.004,0.001);
#257=TOROIDAL_SURFACE('',#13961,0.0075,0.003);
#258=TOROIDAL_SURFACE('',#13969,0.0084,0.0001);
#259=TOROIDAL_SURFACE('',#13970,0.0084,0.0001);
#260=TOROIDAL_SURFACE('',#13971,0.0028,0.0002);
#261=TOROIDAL_SURFACE('',#13972,0.00095,0.0002);
#262=TOROIDAL_SURFACE('',#13973,0.0055,0.001);
#263=TOROIDAL_SURFACE('',#13974,0.0055,0.001);
#264=TOROIDAL_SURFACE('',#13975,0.0062,0.0003);
#265=TOROIDAL_SURFACE('',#13976,0.0062,0.0003);
#266=TOROIDAL_SURFACE('',#13977,0.0096,0.0003);
#267=TOROIDAL_SURFACE('',#13978,0.0096,0.0003);
#268=TOROIDAL_SURFACE('',#13979,0.008,0.0005);
#269=TOROIDAL_SURFACE('',#13983,0.0038,0.0003);
#270=TOROIDAL_SURFACE('',#13984,0.0038,0.0003);
#271=TOROIDAL_SURFACE('',#14011,0.0115,0.001);
#272=TOROIDAL_SURFACE('',#14015,0.002,0.001);
#273=TOROIDAL_SURFACE('',#14019,0.002,0.001);
#274=TOROIDAL_SURFACE('',#14029,0.002,0.001);
#275=TOROIDAL_SURFACE('',#14033,0.002,0.001);
#276=TOROIDAL_SURFACE('',#14038,0.002,0.001);
#277=TOROIDAL_SURFACE('',#14042,0.002,0.001);
#278=TOROIDAL_SURFACE('',#14051,0.0065,0.001);
#279=TOROIDAL_SURFACE('',#14059,0.0115,0.001);
#280=TOROIDAL_SURFACE('',#14062,0.002,0.001);
#281=TOROIDAL_SURFACE('',#14066,0.002,0.001);
#282=TOROIDAL_SURFACE('',#14070,0.002,0.001);
#283=TOROIDAL_SURFACE('',#14074,0.002,0.001);
#284=TOROIDAL_SURFACE('',#14081,0.0115,0.001);
#285=TOROIDAL_SURFACE('',#14089,0.0065,0.001);
#286=TOROIDAL_SURFACE('',#14093,0.002,0.001);
#287=TOROIDAL_SURFACE('',#14096,0.002,0.001);
#288=TOROIDAL_SURFACE('',#14100,0.002,0.001);
#289=TOROIDAL_SURFACE('',#14104,0.002,0.001);
#290=TOROIDAL_SURFACE('',#14107,0.0115,0.001);
#291=TOROIDAL_SURFACE('',#14115,0.0115,0.001);
#292=TOROIDAL_SURFACE('',#14123,0.002,0.001);
#293=TOROIDAL_SURFACE('',#14126,0.002,0.001);
#294=TOROIDAL_SURFACE('',#14130,0.002,0.001);
#295=TOROIDAL_SURFACE('',#14134,0.002,0.001);
#296=TOROIDAL_SURFACE('',#14141,0.0065,0.001);
#297=TOROIDAL_SURFACE('',#14149,0.0115,0.001);
#298=TOROIDAL_SURFACE('',#14153,0.002,0.001);
#299=TOROIDAL_SURFACE('',#14156,0.002,0.001);
#300=TOROIDAL_SURFACE('',#14159,0.002,0.001);
#301=TOROIDAL_SURFACE('',#14162,0.0065,0.001);
#302=TOROIDAL_SURFACE('',#14170,0.002,0.001);
#303=TOROIDAL_SURFACE('',#14220,0.0065,0.001);
#304=TOROIDAL_SURFACE('',#14221,0.0065,0.001);
#305=TOROIDAL_SURFACE('',#14222,0.01055,0.001);
#306=TOROIDAL_SURFACE('',#14224,0.00855,0.001);
#307=TOROIDAL_SURFACE('',#14354,0.009,0.003);
#308=TOROIDAL_SURFACE('',#14369,0.00696039327083855,0.00303960672916145);
#309=TOROIDAL_SURFACE('',#14373,0.013,0.001);
#310=TOROIDAL_SURFACE('',#14374,0.0187,0.0002);
#311=TOROIDAL_SURFACE('',#14375,0.0118,0.0002);
#312=TOROIDAL_SURFACE('',#14376,0.0102,0.0002);
#313=TOROIDAL_SURFACE('',#14377,0.0037676893301498,0.001);
#314=TOROIDAL_SURFACE('',#14378,0.00225,0.001);
#315=TOROIDAL_SURFACE('',#14639,0.002,0.001);
#316=TOROIDAL_SURFACE('',#14640,0.00125,0.001);
#317=TOROIDAL_SURFACE('',#14756,0.0104331778036387,0.001);
#318=TOROIDAL_SURFACE('',#14757,0.044,0.001);
#319=TOROIDAL_SURFACE('',#14758,0.044,0.001);
#320=TOROIDAL_SURFACE('',#14759,0.0104331778036387,0.001);
#321=TOROIDAL_SURFACE('',#14977,0.04,0.01);
#322=TOROIDAL_SURFACE('',#14978,0.02,0.001);
#323=TOROIDAL_SURFACE('',#14979,0.0188,0.0002);
#324=TOROIDAL_SURFACE('',#14980,0.0123,0.0002);
#325=TOROIDAL_SURFACE('',#14982,0.0123,0.0002);
#326=TOROIDAL_SURFACE('',#14985,0.012,0.001);
#327=TOROIDAL_SURFACE('',#14986,0.012,0.004);
#328=TOROIDAL_SURFACE('',#14987,0.019,0.003);
#329=TOROIDAL_SURFACE('',#14988,0.047,0.003);
#330=TOROIDAL_SURFACE('',#14989,0.043,0.01);
#331=TOROIDAL_SURFACE('',#15256,0.0077,0.0003);
#332=TOROIDAL_SURFACE('',#15285,0.0194,0.0002);
#333=TOROIDAL_SURFACE('',#15286,0.019,0.0002);
#334=TOROIDAL_SURFACE('',#15287,0.0130000000000245,0.001);
#335=TOROIDAL_SURFACE('',#15288,0.0192,0.002);
#336=TOROIDAL_SURFACE('',#15293,0.0093,0.001);
#337=CIRCLE('',#13807,0.00455);
#338=CIRCLE('',#13808,0.00241485272203757);
#339=CIRCLE('',#13809,0.00241485272203757);
#340=CIRCLE('',#13810,0.00262);
#341=CIRCLE('',#13812,0.00262);
#342=CIRCLE('',#13813,0.00455);
#343=CIRCLE('',#13815,0.00455);
#344=CIRCLE('',#13816,0.00505);
#345=CIRCLE('',#13820,0.001);
#346=CIRCLE('',#13821,0.001);
#347=CIRCLE('',#13825,0.001);
#348=CIRCLE('',#13826,0.001);
#349=CIRCLE('',#13830,0.001);
#350=CIRCLE('',#13831,0.001);
#351=CIRCLE('',#13833,0.00297688);
#352=CIRCLE('',#13834,0.001397);
#353=CIRCLE('',#13836,0.00297688);
#354=CIRCLE('',#13837,0.001397);
#355=CIRCLE('',#13839,0.00297688);
#356=CIRCLE('',#13840,0.001397);
#357=CIRCLE('',#13842,0.00297688);
#358=CIRCLE('',#13843,0.001397);
#359=CIRCLE('',#13845,0.00400000000000387);
#360=CIRCLE('',#13846,0.00400000000000265);
#361=CIRCLE('',#13847,0.004);
#362=CIRCLE('',#13848,0.00755);
#363=CIRCLE('',#13849,0.05);
#364=CIRCLE('',#13850,0.001397);
#365=CIRCLE('',#13851,0.001397);
#366=CIRCLE('',#13852,0.001397);
#367=CIRCLE('',#13853,0.001397);
#368=CIRCLE('',#13854,0.001);
#369=CIRCLE('',#13855,0.001);
#370=CIRCLE('',#13856,0.001);
#371=CIRCLE('',#13857,0.01);
#372=CIRCLE('',#13859,0.00400000000000387);
#373=CIRCLE('',#13860,0.004);
#374=CIRCLE('',#13861,0.05);
#375=CIRCLE('',#13862,0.00755);
#376=CIRCLE('',#13863,0.00400000000000265);
#377=CIRCLE('',#13864,0.00297688);
#378=CIRCLE('',#13865,0.00297688);
#379=CIRCLE('',#13866,0.00297688);
#380=CIRCLE('',#13867,0.00297688);
#381=CIRCLE('',#13868,0.001);
#382=CIRCLE('',#13869,0.001);
#383=CIRCLE('',#13870,0.001);
#384=CIRCLE('',#13871,0.01);
#385=CIRCLE('',#13873,0.00755);
#386=CIRCLE('',#13874,0.00505);
#387=CIRCLE('',#13876,0.00755);
#388=CIRCLE('',#13877,0.00555);
#389=CIRCLE('',#13879,0.00455);
#390=CIRCLE('',#13901,0.00241485272203757);
#391=CIRCLE('',#13905,0.0045);
#392=CIRCLE('',#13906,0.0038);
#393=CIRCLE('',#13908,0.0045);
#394=CIRCLE('',#13909,0.0038);
#395=CIRCLE('',#13910,0.00651286233460729);
#396=CIRCLE('',#13913,0.0003);
#397=CIRCLE('',#13916,0.0084);
#398=CIRCLE('',#13917,0.0096);
#399=CIRCLE('',#13919,0.0084);
#400=CIRCLE('',#13920,0.0096);
#401=CIRCLE('',#13922,0.0075);
#402=CIRCLE('',#13923,0.0099);
#403=CIRCLE('',#13925,0.0055);
#404=CIRCLE('',#13926,0.0062);
#405=CIRCLE('',#13928,0.0055);
#406=CIRCLE('',#13929,0.0062);
#407=CIRCLE('',#13931,0.00261523063261997);
#408=CIRCLE('',#13932,0.0045);
#409=CIRCLE('',#13934,0.00095);
#410=CIRCLE('',#13935,0.0028);
#411=CIRCLE('',#13937,0.0075);
#412=CIRCLE('',#13938,0.004);
#413=CIRCLE('',#13940,0.0099);
#414=CIRCLE('',#13941,0.008);
#415=CIRCLE('',#13943,0.0045);
#416=CIRCLE('',#13945,0.0065);
#417=CIRCLE('',#13946,0.0065);
#418=CIRCLE('',#13948,0.0075);
#419=CIRCLE('',#13950,0.003);
#420=CIRCLE('',#13952,0.003);
#421=CIRCLE('',#13954,0.00075);
#422=CIRCLE('',#13955,0.00075);
#423=CIRCLE('',#13959,0.0045);
#424=CIRCLE('',#13960,0.0045);
#425=CIRCLE('',#13963,0.0099);
#426=CIRCLE('',#13965,0.0083);
#427=CIRCLE('',#13966,0.0083);
#428=CIRCLE('',#13968,0.0099);
#429=CIRCLE('',#13981,0.0035);
#430=CIRCLE('',#13982,0.0035);
#431=CIRCLE('',#13991,0.000254000000000004);
#432=CIRCLE('',#13992,0.000254000000000037);
#433=CIRCLE('',#13994,0.009236);
#434=CIRCLE('',#13995,0.00076200000000009);
#435=CIRCLE('',#13996,0.0007619999999999);
#436=CIRCLE('',#13999,0.0081692);
#437=CIRCLE('',#14001,0.0081692);
#438=CIRCLE('',#14005,0.000595);
#439=CIRCLE('',#14007,0.000594999999999988);
#440=CIRCLE('',#14010,0.001);
#441=CIRCLE('',#14012,0.001);
#442=CIRCLE('',#14013,0.0125);
#443=CIRCLE('',#14014,0.0115);
#444=CIRCLE('',#14016,0.001);
#445=CIRCLE('',#14017,0.002);
#446=CIRCLE('',#14018,0.001);
#447=CIRCLE('',#14020,0.001);
#448=CIRCLE('',#14021,0.001);
#449=CIRCLE('',#14022,0.002);
#450=CIRCLE('',#14024,0.001);
#451=CIRCLE('',#14026,0.001);
#452=CIRCLE('',#14028,0.001);
#453=CIRCLE('',#14030,0.002);
#454=CIRCLE('',#14031,0.001);
#455=CIRCLE('',#14032,0.001);
#456=CIRCLE('',#14034,0.001);
#457=CIRCLE('',#14035,0.002);
#458=CIRCLE('',#14036,0.001);
#459=CIRCLE('',#14037,0.001);
#460=CIRCLE('',#14039,0.001);
#461=CIRCLE('',#14040,0.001);
#462=CIRCLE('',#14041,0.002);
#463=CIRCLE('',#14043,0.002);
#464=CIRCLE('',#14044,0.001);
#465=CIRCLE('',#14045,0.001);
#466=CIRCLE('',#14048,0.001);
#467=CIRCLE('',#14050,0.001);
#468=CIRCLE('',#14052,0.001);
#469=CIRCLE('',#14053,0.0075);
#470=CIRCLE('',#14054,0.0065);
#471=CIRCLE('',#14056,0.001);
#472=CIRCLE('',#14058,0.001);
#473=CIRCLE('',#14060,0.0115);
#474=CIRCLE('',#14061,0.0125);
#475=CIRCLE('',#14063,0.002);
#476=CIRCLE('',#14064,0.001);
#477=CIRCLE('',#14065,0.001);
#478=CIRCLE('',#14067,0.001);
#479=CIRCLE('',#14068,0.002);
#480=CIRCLE('',#14069,0.001);
#481=CIRCLE('',#14071,0.001);
#482=CIRCLE('',#14072,0.001);
#483=CIRCLE('',#14073,0.002);
#484=CIRCLE('',#14075,0.001);
#485=CIRCLE('',#14076,0.002);
#486=CIRCLE('',#14078,0.001);
#487=CIRCLE('',#14080,0.001);
#488=CIRCLE('',#14082,0.001);
#489=CIRCLE('',#14083,0.0115);
#490=CIRCLE('',#14084,0.0125);
#491=CIRCLE('',#14086,0.001);
#492=CIRCLE('',#14088,0.001);
#493=CIRCLE('',#14090,0.001);
#494=CIRCLE('',#14091,0.0065);
#495=CIRCLE('',#14092,0.0075);
#496=CIRCLE('',#14094,0.002);
#497=CIRCLE('',#14095,0.001);
#498=CIRCLE('',#14097,0.001);
#499=CIRCLE('',#14098,0.002);
#500=CIRCLE('',#14099,0.001);
#501=CIRCLE('',#14101,0.001);
#502=CIRCLE('',#14102,0.001);
#503=CIRCLE('',#14103,0.002);
#504=CIRCLE('',#14105,0.001);
#505=CIRCLE('',#14106,0.002);
#506=CIRCLE('',#14108,0.001);
#507=CIRCLE('',#14109,0.0125);
#508=CIRCLE('',#14110,0.0115);
#509=CIRCLE('',#14112,0.001);
#510=CIRCLE('',#14114,0.001);
#511=CIRCLE('',#14116,0.001);
#512=CIRCLE('',#14117,0.0125);
#513=CIRCLE('',#14118,0.0115);
#514=CIRCLE('',#14120,0.001);
#515=CIRCLE('',#14122,0.001);
#516=CIRCLE('',#14124,0.002);
#517=CIRCLE('',#14125,0.001);
#518=CIRCLE('',#14127,0.001);
#519=CIRCLE('',#14128,0.002);
#520=CIRCLE('',#14129,0.001);
#521=CIRCLE('',#14131,0.001);
#522=CIRCLE('',#14132,0.001);
#523=CIRCLE('',#14133,0.002);
#524=CIRCLE('',#14135,0.001);
#525=CIRCLE('',#14136,0.002);
#526=CIRCLE('',#14138,0.001);
#527=CIRCLE('',#14140,0.001);
#528=CIRCLE('',#14142,0.001);
#529=CIRCLE('',#14143,0.0065);
#530=CIRCLE('',#14144,0.0075);
#531=CIRCLE('',#14146,0.001);
#532=CIRCLE('',#14148,0.001);
#533=CIRCLE('',#14150,0.001);
#534=CIRCLE('',#14151,0.0115);
#535=CIRCLE('',#14152,0.0125);
#536=CIRCLE('',#14154,0.002);
#537=CIRCLE('',#14155,0.001);
#538=CIRCLE('',#14157,0.001);
#539=CIRCLE('',#14158,0.002);
#540=CIRCLE('',#14160,0.001);
#541=CIRCLE('',#14161,0.002);
#542=CIRCLE('',#14163,0.001);
#543=CIRCLE('',#14164,0.0075);
#544=CIRCLE('',#14165,0.0065);
#545=CIRCLE('',#14167,0.001);
#546=CIRCLE('',#14169,0.001);
#547=CIRCLE('',#14171,0.002);
#548=CIRCLE('',#14173,0.00277876);
#549=CIRCLE('',#14174,0.0012192);
#550=CIRCLE('',#14176,0.00277876);
#551=CIRCLE('',#14177,0.0012192);
#552=CIRCLE('',#14179,0.00277876);
#553=CIRCLE('',#14180,0.0012192);
#554=CIRCLE('',#14185,0.00655);
#555=CIRCLE('',#14186,0.00855);
#556=CIRCLE('',#14188,0.00277876);
#557=CIRCLE('',#14189,0.00277876);
#558=CIRCLE('',#14190,0.00277876);
#559=CIRCLE('',#14191,0.0065);
#560=CIRCLE('',#14192,0.01055);
#561=CIRCLE('',#14196,0.0075);
#562=CIRCLE('',#14197,0.0075);
#563=CIRCLE('',#14207,0.0065);
#564=CIRCLE('',#14208,0.0012192);
#565=CIRCLE('',#14209,0.0012192);
#566=CIRCLE('',#14210,0.0012192);
#567=CIRCLE('',#14211,0.00655);
#568=CIRCLE('',#14223,0.00955);
#569=CIRCLE('',#14227,0.00564195203204444);
#570=CIRCLE('',#14229,0.00613648743432167);
#571=CIRCLE('',#14231,0.00613648743432167);
#572=CIRCLE('',#14233,0.00564195203204444);
#573=CIRCLE('',#14235,0.00613648743432167);
#574=CIRCLE('',#14237,0.00613648743432167);
#575=CIRCLE('',#14239,0.00564195203204444);
#576=CIRCLE('',#14241,0.00564195203204444);
#577=CIRCLE('',#14244,0.0012573);
#578=CIRCLE('',#14245,0.0026416);
#579=CIRCLE('',#14247,0.0012573);
#580=CIRCLE('',#14249,0.00613648743432167);
#581=CIRCLE('',#14251,0.00613648743432167);
#582=CIRCLE('',#14253,0.00613648743432167);
#583=CIRCLE('',#14255,0.00613648743432167);
#584=CIRCLE('',#14257,0.00255937815401834);
#585=CIRCLE('',#14263,0.004);
#586=CIRCLE('',#14264,0.0012192);
#587=CIRCLE('',#14266,0.004);
#588=CIRCLE('',#14267,0.0012192);
#589=CIRCLE('',#14270,0.0012192);
#590=CIRCLE('',#14273,0.0012192);
#591=CIRCLE('',#14278,0.0045499999999755);
#592=CIRCLE('',#14279,0.0080000000000245);
#593=CIRCLE('',#14281,0.0140000000000245);
#594=CIRCLE('',#14282,0.0045499999999755);
#595=CIRCLE('',#14284,0.0120000000000245);
#596=CIRCLE('',#14285,0.0140000000000245);
#597=CIRCLE('',#14287,0.0100000000000245);
#598=CIRCLE('',#14288,0.0120000000000245);
#599=CIRCLE('',#14290,0.0080000000000245);
#600=CIRCLE('',#14291,0.00906043638285393);
#601=CIRCLE('',#14293,0.0100000000000245);
#602=CIRCLE('',#14300,0.000762);
#603=CIRCLE('',#14301,0.000762000000000046);
#604=CIRCLE('',#14302,0.000762000000000038);
#605=CIRCLE('',#14304,0.0081692);
#606=CIRCLE('',#14306,0.000254);
#607=CIRCLE('',#14307,0.000254000000000014);
#608=CIRCLE('',#14309,0.009236);
#609=CIRCLE('',#14310,0.009236);
#610=CIRCLE('',#14313,0.000253999999999972);
#611=CIRCLE('',#14314,0.00840975562057229);
#612=CIRCLE('',#14316,0.009236);
#613=CIRCLE('',#14318,0.009236);
#614=CIRCLE('',#14319,0.012);
#615=CIRCLE('',#14321,0.012);
#616=CIRCLE('',#14323,0.009236);
#617=CIRCLE('',#14324,0.01);
#618=CIRCLE('',#14326,0.008);
#619=CIRCLE('',#14328,0.01);
#620=CIRCLE('',#14329,0.008);
#621=CIRCLE('',#14336,0.00125);
#622=CIRCLE('',#14337,0.00325);
#623=CIRCLE('',#14339,0.012);
#624=CIRCLE('',#14340,0.0189);
#625=CIRCLE('',#14342,0.013);
#626=CIRCLE('',#14343,0.0187);
#627=CIRCLE('',#14345,0.0102);
#628=CIRCLE('',#14346,0.0118);
#629=CIRCLE('',#14348,0.012);
#630=CIRCLE('',#14349,0.012);
#631=CIRCLE('',#14351,0.0189);
#632=CIRCLE('',#14353,0.012);
#633=CIRCLE('',#14355,0.010026060429977);
#634=CIRCLE('',#14357,0.00512938524157182);
#635=CIRCLE('',#14359,0.00325);
#636=CIRCLE('',#14362,0.00125);
#637=CIRCLE('',#14364,0.00294853728586081);
#638=CIRCLE('',#14365,0.00143084795571101);
#639=CIRCLE('',#14367,0.008);
#640=CIRCLE('',#14368,0.00342566918682414);
#641=CIRCLE('',#14370,0.01);
#642=CIRCLE('',#14372,0.01);
#643=CIRCLE('',#14381,0.001);
#644=CIRCLE('',#14382,0.000625);
#645=CIRCLE('',#14387,0.0025);
#646=CIRCLE('',#14388,0.002);
#647=CIRCLE('',#14390,0.0045);
#648=CIRCLE('',#14391,0.0045);
#649=CIRCLE('',#14392,0.0045);
#650=CIRCLE('',#14393,0.0045);
#651=CIRCLE('',#14394,0.0045);
#652=CIRCLE('',#14395,0.0045);
#653=CIRCLE('',#14396,0.0045);
#654=CIRCLE('',#14397,0.0045);
#655=CIRCLE('',#14398,0.0045);
#656=CIRCLE('',#14399,0.0045);
#657=CIRCLE('',#14400,0.0045);
#658=CIRCLE('',#14401,0.0045);
#659=CIRCLE('',#14402,0.0045);
#660=CIRCLE('',#14403,0.0045);
#661=CIRCLE('',#14404,0.0045);
#662=CIRCLE('',#14405,0.0045);
#663=CIRCLE('',#14406,0.0045);
#664=CIRCLE('',#14407,0.0045);
#665=CIRCLE('',#14408,0.0045);
#666=CIRCLE('',#14409,0.0045);
#667=CIRCLE('',#14410,0.0045);
#668=CIRCLE('',#14411,0.0045);
#669=CIRCLE('',#14412,0.0045);
#670=CIRCLE('',#14413,0.0045);
#671=CIRCLE('',#14414,0.0045);
#672=CIRCLE('',#14415,0.0045);
#673=CIRCLE('',#14416,0.0045);
#674=CIRCLE('',#14417,0.0045);
#675=CIRCLE('',#14418,0.0045);
#676=CIRCLE('',#14419,0.0045);
#677=CIRCLE('',#14420,0.0045);
#678=CIRCLE('',#14421,0.0045);
#679=CIRCLE('',#14422,0.0045);
#680=CIRCLE('',#14423,0.0045);
#681=CIRCLE('',#14424,0.0045);
#682=CIRCLE('',#14425,0.0045);
#683=CIRCLE('',#14426,0.0045);
#684=CIRCLE('',#14427,0.0045);
#685=CIRCLE('',#14428,0.0045);
#686=CIRCLE('',#14429,0.0045);
#687=CIRCLE('',#14430,0.0045);
#688=CIRCLE('',#14431,0.0045);
#689=CIRCLE('',#14432,0.0045);
#690=CIRCLE('',#14433,0.0045);
#691=CIRCLE('',#14434,0.0045);
#692=CIRCLE('',#14435,0.0045);
#693=CIRCLE('',#14436,0.0045);
#694=CIRCLE('',#14437,0.00025);
#695=CIRCLE('',#14439,0.0045);
#696=CIRCLE('',#14440,0.0045);
#697=CIRCLE('',#14441,0.0045);
#698=CIRCLE('',#14442,0.0045);
#699=CIRCLE('',#14443,0.0045);
#700=CIRCLE('',#14444,0.0045);
#701=CIRCLE('',#14445,0.0045);
#702=CIRCLE('',#14446,0.0045);
#703=CIRCLE('',#14447,0.0045);
#704=CIRCLE('',#14448,0.0045);
#705=CIRCLE('',#14449,0.0045);
#706=CIRCLE('',#14450,0.0045);
#707=CIRCLE('',#14451,0.0045);
#708=CIRCLE('',#14452,0.0045);
#709=CIRCLE('',#14453,0.0045);
#710=CIRCLE('',#14454,0.0045);
#711=CIRCLE('',#14455,0.0045);
#712=CIRCLE('',#14456,0.0045);
#713=CIRCLE('',#14457,0.0045);
#714=CIRCLE('',#14458,0.0045);
#715=CIRCLE('',#14459,0.0045);
#716=CIRCLE('',#14460,0.0045);
#717=CIRCLE('',#14461,0.0045);
#718=CIRCLE('',#14462,0.0045);
#719=CIRCLE('',#14463,0.0045);
#720=CIRCLE('',#14464,0.0045);
#721=CIRCLE('',#14465,0.0045);
#722=CIRCLE('',#14466,0.0045);
#723=CIRCLE('',#14467,0.0045);
#724=CIRCLE('',#14468,0.0045);
#725=CIRCLE('',#14469,0.0045);
#726=CIRCLE('',#14470,0.0045);
#727=CIRCLE('',#14471,0.0045);
#728=CIRCLE('',#14472,0.0045);
#729=CIRCLE('',#14473,0.0045);
#730=CIRCLE('',#14474,0.0045);
#731=CIRCLE('',#14475,0.0045);
#732=CIRCLE('',#14476,0.0045);
#733=CIRCLE('',#14477,0.0045);
#734=CIRCLE('',#14478,0.0045);
#735=CIRCLE('',#14479,0.0045);
#736=CIRCLE('',#14480,0.0045);
#737=CIRCLE('',#14481,0.0045);
#738=CIRCLE('',#14482,0.0045);
#739=CIRCLE('',#14483,0.0045);
#740=CIRCLE('',#14484,0.0045);
#741=CIRCLE('',#14485,0.0045);
#742=CIRCLE('',#14486,0.004);
#743=CIRCLE('',#14631,0.0025);
#744=CIRCLE('',#14632,0.004);
#745=CIRCLE('',#14636,0.00025);
#746=CIRCLE('',#14638,0.001);
#747=CIRCLE('',#14643,0.00325);
#748=CIRCLE('',#14644,0.00375);
#749=CIRCLE('',#14646,0.00375);
#750=CIRCLE('',#14647,0.00325);
#751=CIRCLE('',#14652,0.0123);
#752=CIRCLE('',#14653,0.0188);
#753=CIRCLE('',#14655,0.0123);
#754=CIRCLE('',#14656,0.0188);
#755=CIRCLE('',#14662,0.000477030566374308);
#756=CIRCLE('',#14663,0.00322703056637436);
#757=CIRCLE('',#14664,0.000477030566374308);
#758=CIRCLE('',#14665,0.00227296943362574);
#759=CIRCLE('',#14667,0.000477030566374308);
#760=CIRCLE('',#14669,0.000477030566374308);
#761=CIRCLE('',#14671,0.000477030566374308);
#762=CIRCLE('',#14672,0.00227296943362564);
#763=CIRCLE('',#14673,0.000477030566374308);
#764=CIRCLE('',#14674,0.00322703056637426);
#765=CIRCLE('',#14676,0.00322703056637426);
#766=CIRCLE('',#14678,0.00227296943362564);
#767=CIRCLE('',#14680,0.0035);
#768=CIRCLE('',#14682,0.001);
#769=CIRCLE('',#14684,0.00322703056637436);
#770=CIRCLE('',#14685,0.00227296943362574);
#771=CIRCLE('',#14686,0.0035);
#772=CIRCLE('',#14687,0.001);
#773=CIRCLE('',#14688,0.000477030566374308);
#774=CIRCLE('',#14689,0.000477030566374308);
#775=CIRCLE('',#14701,0.001);
#776=CIRCLE('',#14702,0.001);
#777=CIRCLE('',#14707,0.001);
#778=CIRCLE('',#14708,0.001);
#779=CIRCLE('',#14712,0.001);
#780=CIRCLE('',#14713,0.001);
#781=CIRCLE('',#14715,0.00277876);
#782=CIRCLE('',#14716,0.0012192);
#783=CIRCLE('',#14718,0.00277876);
#784=CIRCLE('',#14719,0.0012192);
#785=CIRCLE('',#14721,0.00277876);
#786=CIRCLE('',#14722,0.0012192);
#787=CIRCLE('',#14724,0.00277876);
#788=CIRCLE('',#14725,0.00277876);
#789=CIRCLE('',#14726,0.00277876);
#790=CIRCLE('',#14727,0.001);
#791=CIRCLE('',#14728,0.001);
#792=CIRCLE('',#14729,0.001);
#793=CIRCLE('',#14730,0.0104331778036387);
#794=CIRCLE('',#14731,0.044);
#795=CIRCLE('',#14733,0.0012192);
#796=CIRCLE('',#14734,0.0012192);
#797=CIRCLE('',#14735,0.0012192);
#798=CIRCLE('',#14736,0.001);
#799=CIRCLE('',#14737,0.001);
#800=CIRCLE('',#14738,0.001);
#801=CIRCLE('',#14739,0.044);
#802=CIRCLE('',#14740,0.0104331778036387);
#803=CIRCLE('',#14742,0.045);
#804=CIRCLE('',#14743,0.045);
#805=CIRCLE('',#14745,0.00943317780363869);
#806=CIRCLE('',#14746,0.00943317780363869);
#807=CIRCLE('',#14766,0.001);
#808=CIRCLE('',#14767,0.001);
#809=CIRCLE('',#14771,0.001);
#810=CIRCLE('',#14773,0.001);
#811=CIRCLE('',#14774,0.001);
#812=CIRCLE('',#14778,0.001);
#813=CIRCLE('',#14780,0.001);
#814=CIRCLE('',#14781,0.001);
#815=CIRCLE('',#14785,0.001);
#816=CIRCLE('',#14787,0.00943317780363869);
#817=CIRCLE('',#14788,0.045);
#818=CIRCLE('',#14789,0.001);
#819=CIRCLE('',#14790,0.001);
#820=CIRCLE('',#14791,0.001);
#821=CIRCLE('',#14793,0.00943317780363869);
#822=CIRCLE('',#14794,0.045);
#823=CIRCLE('',#14806,0.000477030566374308);
#824=CIRCLE('',#14807,0.00322703056637436);
#825=CIRCLE('',#14808,0.000477030566374308);
#826=CIRCLE('',#14809,0.00227296943362574);
#827=CIRCLE('',#14811,0.000477030566374308);
#828=CIRCLE('',#14813,0.000477030566374308);
#829=CIRCLE('',#14815,0.000477030566374308);
#830=CIRCLE('',#14816,0.00227296943362564);
#831=CIRCLE('',#14817,0.000477030566374308);
#832=CIRCLE('',#14818,0.00322703056637426);
#833=CIRCLE('',#14820,0.00322703056637426);
#834=CIRCLE('',#14822,0.00227296943362564);
#835=CIRCLE('',#14824,0.001);
#836=CIRCLE('',#14825,0.0035);
#837=CIRCLE('',#14826,0.001);
#838=CIRCLE('',#14827,0.0035);
#839=CIRCLE('',#14829,0.001);
#840=CIRCLE('',#14831,0.0035);
#841=CIRCLE('',#14832,0.001);
#842=CIRCLE('',#14833,0.000477030566374308);
#843=CIRCLE('',#14834,0.000477030566374308);
#844=CIRCLE('',#14836,0.0035);
#845=CIRCLE('',#14838,0.001);
#846=CIRCLE('',#14839,0.00322703056637436);
#847=CIRCLE('',#14840,0.00227296943362574);
#848=CIRCLE('',#14849,0.05);
#849=CIRCLE('',#14850,0.053);
#850=CIRCLE('',#14852,0.005);
#851=CIRCLE('',#14853,0.005);
#852=CIRCLE('',#14855,0.001397);
#853=CIRCLE('',#14856,0.003);
#854=CIRCLE('',#14857,0.003);
#855=CIRCLE('',#14858,0.005);
#856=CIRCLE('',#14859,0.05);
#857=CIRCLE('',#14861,0.005);
#858=CIRCLE('',#14863,0.001397);
#859=CIRCLE('',#14864,0.003);
#860=CIRCLE('',#14865,0.05);
#861=CIRCLE('',#14866,0.003);
#862=CIRCLE('',#14868,0.001397);
#863=CIRCLE('',#14869,0.003);
#864=CIRCLE('',#14870,0.003);
#865=CIRCLE('',#14871,0.005);
#866=CIRCLE('',#14872,0.05);
#867=CIRCLE('',#14873,0.005);
#868=CIRCLE('',#14875,0.005);
#869=CIRCLE('',#14877,0.001397);
#870=CIRCLE('',#14878,0.003);
#871=CIRCLE('',#14879,0.005);
#872=CIRCLE('',#14880,0.05);
#873=CIRCLE('',#14881,0.003);
#874=CIRCLE('',#14884,0.001397);
#875=CIRCLE('',#14885,0.003);
#876=CIRCLE('',#14886,0.003);
#877=CIRCLE('',#14887,0.005);
#878=CIRCLE('',#14888,0.05);
#879=CIRCLE('',#14889,0.005);
#880=CIRCLE('',#14891,0.001397);
#881=CIRCLE('',#14892,0.003);
#882=CIRCLE('',#14893,0.005);
#883=CIRCLE('',#14894,0.05);
#884=CIRCLE('',#14895,0.005);
#885=CIRCLE('',#14896,0.003);
#886=CIRCLE('',#14898,0.001397);
#887=CIRCLE('',#14899,0.003);
#888=CIRCLE('',#14900,0.003);
#889=CIRCLE('',#14901,0.005);
#890=CIRCLE('',#14902,0.05);
#891=CIRCLE('',#14903,0.005);
#892=CIRCLE('',#14905,0.005);
#893=CIRCLE('',#14907,0.001397);
#894=CIRCLE('',#14908,0.003);
#895=CIRCLE('',#14909,0.005);
#896=CIRCLE('',#14910,0.05);
#897=CIRCLE('',#14911,0.003);
#898=CIRCLE('',#14934,0.043);
#899=CIRCLE('',#14939,0.01);
#900=CIRCLE('',#14940,0.012);
#901=CIRCLE('',#14942,0.000202360810977542);
#902=CIRCLE('',#14944,0.0002);
#903=CIRCLE('',#14946,0.001);
#904=CIRCLE('',#14948,0.001);
#905=CIRCLE('',#14950,0.04);
#906=CIRCLE('',#14952,0.0188);
#907=CIRCLE('',#14953,0.0123);
#908=CIRCLE('',#14955,0.013);
#909=CIRCLE('',#14956,0.047);
#910=CIRCLE('',#14957,0.019);
#911=CIRCLE('',#14959,0.0441317460907982);
#912=CIRCLE('',#14960,0.01);
#913=CIRCLE('',#14961,0.02);
#914=CIRCLE('',#14963,0.05);
#915=CIRCLE('',#14966,0.019);
#916=CIRCLE('',#14967,0.019);
#917=CIRCLE('',#14969,0.0121);
#918=CIRCLE('',#14970,0.0121);
#919=CIRCLE('',#14972,0.016);
#920=CIRCLE('',#14973,0.016);
#921=CIRCLE('',#14975,0.05);
#922=CIRCLE('',#14976,0.05);
#923=CIRCLE('',#14981,0.0122857142857138);
#924=CIRCLE('',#14984,0.013);
#925=CIRCLE('',#14990,0.053);
#926=CIRCLE('',#15002,0.001);
#927=CIRCLE('',#15003,0.001);
#928=CIRCLE('',#15007,0.001);
#929=CIRCLE('',#15009,0.001);
#930=CIRCLE('',#15010,0.001);
#931=CIRCLE('',#15014,0.001);
#932=CIRCLE('',#15016,0.001);
#933=CIRCLE('',#15017,0.001);
#934=CIRCLE('',#15021,0.001);
#935=CIRCLE('',#15023,0.00400000000000265);
#936=CIRCLE('',#15024,0.05);
#937=CIRCLE('',#15025,0.00400000000000387);
#938=CIRCLE('',#15026,0.004);
#939=CIRCLE('',#15027,0.00755);
#940=CIRCLE('',#15028,0.001);
#941=CIRCLE('',#15029,0.001);
#942=CIRCLE('',#15030,0.001);
#943=CIRCLE('',#15031,0.01);
#944=CIRCLE('',#15033,0.00400000000000265);
#945=CIRCLE('',#15034,0.05);
#946=CIRCLE('',#15035,0.00400000000000387);
#947=CIRCLE('',#15036,0.004);
#948=CIRCLE('',#15037,0.00755);
#949=CIRCLE('',#15038,0.01);
#950=CIRCLE('',#15085,0.00736858102143575);
#951=CIRCLE('',#15086,0.00736858102143575);
#952=CIRCLE('',#15087,0.00736858102143575);
#953=CIRCLE('',#15088,0.00736858102143575);
#954=CIRCLE('',#15089,0.00736858102143575);
#955=CIRCLE('',#15090,0.00736858102143575);
#956=CIRCLE('',#15091,0.00736858102143575);
#957=CIRCLE('',#15092,0.00736858102143575);
#958=CIRCLE('',#15093,0.00736858102143575);
#959=CIRCLE('',#15094,0.00736858102143575);
#960=CIRCLE('',#15095,0.00736858102143575);
#961=CIRCLE('',#15096,0.0004);
#962=CIRCLE('',#15098,0.00736858102143575);
#963=CIRCLE('',#15099,0.00736858102143575);
#964=CIRCLE('',#15100,0.00736858102143575);
#965=CIRCLE('',#15101,0.00736858102143575);
#966=CIRCLE('',#15102,0.00736858102143575);
#967=CIRCLE('',#15103,0.00736858102143575);
#968=CIRCLE('',#15104,0.00736858102143575);
#969=CIRCLE('',#15105,0.00736858102143575);
#970=CIRCLE('',#15106,0.00736858102143575);
#971=CIRCLE('',#15107,0.00736858102143575);
#972=CIRCLE('',#15108,0.00736858102143575);
#973=CIRCLE('',#15109,0.005);
#974=CIRCLE('',#15112,0.005);
#975=CIRCLE('',#15113,0.0004);
#976=CIRCLE('',#15129,0.00227296943362564);
#977=CIRCLE('',#15130,0.000477030566374308);
#978=CIRCLE('',#15131,0.00322703056637426);
#979=CIRCLE('',#15132,0.000477030566374308);
#980=CIRCLE('',#15134,0.00322703056637426);
#981=CIRCLE('',#15136,0.00227296943362564);
#982=CIRCLE('',#15138,0.000477030566374308);
#983=CIRCLE('',#15139,0.00227296943362574);
#984=CIRCLE('',#15140,0.000477030566374308);
#985=CIRCLE('',#15141,0.00322703056637436);
#986=CIRCLE('',#15143,0.000477030566374308);
#987=CIRCLE('',#15145,0.000477030566374308);
#988=CIRCLE('',#15147,0.008);
#989=CIRCLE('',#15148,0.0035);
#990=CIRCLE('',#15149,0.008);
#991=CIRCLE('',#15150,0.0025);
#992=CIRCLE('',#15155,0.00209191070279862);
#993=CIRCLE('',#15156,0.00209191070279862);
#994=CIRCLE('',#15158,0.0015);
#995=CIRCLE('',#15159,0.001);
#996=CIRCLE('',#15161,0.008);
#997=CIRCLE('',#15162,0.008);
#998=CIRCLE('',#15164,0.0015);
#999=CIRCLE('',#15165,0.0099);
#1000=CIRCLE('',#15166,0.0025);
#1001=CIRCLE('',#15171,0.000477030566374308);
#1002=CIRCLE('',#15172,0.000477030566374308);
#1003=CIRCLE('',#15173,0.008);
#1004=CIRCLE('',#15174,0.0099);
#1005=CIRCLE('',#15175,0.0035);
#1006=CIRCLE('',#15176,0.00322703056637436);
#1007=CIRCLE('',#15177,0.00227296943362574);
#1008=CIRCLE('',#15182,0.001);
#1009=CIRCLE('',#15192,0.006);
#1010=CIRCLE('',#15193,0.006);
#1011=CIRCLE('',#15196,0.003);
#1012=CIRCLE('',#15197,0.003);
#1013=CIRCLE('',#15200,0.006);
#1014=CIRCLE('',#15201,0.006);
#1015=CIRCLE('',#15204,0.003);
#1016=CIRCLE('',#15205,0.003);
#1017=CIRCLE('',#15208,0.006);
#1018=CIRCLE('',#15209,0.006);
#1019=CIRCLE('',#15212,0.003);
#1020=CIRCLE('',#15213,0.003);
#1021=CIRCLE('',#15216,0.006);
#1022=CIRCLE('',#15217,0.006);
#1023=CIRCLE('',#15220,0.003);
#1024=CIRCLE('',#15221,0.003);
#1025=CIRCLE('',#15223,0.00180420299878392);
#1026=CIRCLE('',#15224,0.003);
#1027=CIRCLE('',#15225,0.003);
#1028=CIRCLE('',#15226,0.003);
#1029=CIRCLE('',#15227,0.003);
#1030=CIRCLE('',#15229,0.0077);
#1031=CIRCLE('',#15230,0.0043976164792475);
#1032=CIRCLE('',#15231,0.0043976164792475);
#1033=CIRCLE('',#15232,0.0043976164792475);
#1034=CIRCLE('',#15233,0.0043976164792475);
#1035=CIRCLE('',#15235,0.008);
#1036=CIRCLE('',#15236,0.006);
#1037=CIRCLE('',#15237,0.006);
#1038=CIRCLE('',#15238,0.006);
#1039=CIRCLE('',#15239,0.006);
#1040=CIRCLE('',#15241,0.003);
#1041=CIRCLE('',#15242,0.003);
#1042=CIRCLE('',#15243,0.003);
#1043=CIRCLE('',#15244,0.003);
#1044=CIRCLE('',#15245,0.00180420299878392);
#1045=CIRCLE('',#15255,0.008);
#1046=CIRCLE('',#15259,0.000999999999685245);
#1047=CIRCLE('',#15262,0.0009999999999995);
#1048=CIRCLE('',#15263,0.000999999999471396);
#1049=CIRCLE('',#15266,0.000999999999690151);
#1050=CIRCLE('',#15270,0.0120000000000245);
#1051=CIRCLE('',#15271,0.0192);
#1052=CIRCLE('',#15273,0.019);
#1053=CIRCLE('',#15274,0.0130000000000245);
#1054=CIRCLE('',#15276,0.0212);
#1055=CIRCLE('',#15277,0.0194);
#1056=CIRCLE('',#15279,0.0192);
#1057=CIRCLE('',#15280,0.0192);
#1058=CIRCLE('',#15282,0.0120000000000245);
#1059=CIRCLE('',#15284,0.0212);
#1060=CIRCLE('',#15291,0.01);
#1061=CIRCLE('',#15292,0.01);
#1062=B_SPLINE_CURVE_WITH_KNOTS('',3,(#19536,#19537,#19538,#19539),
 .UNSPECIFIED.,.F.,.F.,(4,4),(0.,0.00278168915164146),.UNSPECIFIED.);
#1063=B_SPLINE_CURVE_WITH_KNOTS('',2,(#19634,#19635,#19636),
 .UNSPECIFIED.,.F.,.F.,(3,3),(0.,1.),.UNSPECIFIED.);
#1064=B_SPLINE_CURVE_WITH_KNOTS('',2,(#19641,#19642,#19643),
 .UNSPECIFIED.,.F.,.F.,(3,3),(0.,1.),.UNSPECIFIED.);
#1065=B_SPLINE_CURVE_WITH_KNOTS('',3,(#19997,#19998,#19999,#20000,#20001),
 .UNSPECIFIED.,.F.,.F.,(4,1,4),(4.46872309623959E-16,0.00181535454777857,
0.0036307090955567),.UNSPECIFIED.);
#1066=B_SPLINE_CURVE_WITH_KNOTS('',3,(#20463,#20464,#20465,#20466,#20467,
#20468,#20469,#20470,#20471,#20472,#20473,#20474,#20475,#20476,#20477,#20478,
#20479,#20480,#20481,#20482,#20483,#20484,#20485,#20486,#20487,#20488,#20489,
#20490,#20491,#20492,#20493,#20494,#20495,#20496,#20497,#20498,#20499,#20500,
#20501,#20502,#20503,#20504,#20505,#20506,#20507,#20508,#20509,#20510,#20511,
#20512,#20513,#20514,#20515,#20516,#20517,#20518,#20519,#20520,#20521,#20522,
#20523,#20524,#20525,#20526,#20527,#20528,#20529,#20530,#20531,#20532,#20533,
#20534,#20535,#20536,#20537,#20538,#20539,#20540,#20541,#20542,#20543,#20544,
#20545,#20546,#20547,#20548,#20549,#20550,#20551,#20552,#20553,#20554,#20555,
#20556,#20557,#20558,#20559,#20560,#20561,#20562),.UNSPECIFIED.,.F.,.F.,
(4,1,1,1,1,1,1,1,1,1,1,1,1,1,1,1,1,1,1,1,1,1,1,1,1,1,1,1,1,1,1,1,1,1,1,
1,1,1,1,1,1,1,1,1,1,1,1,1,1,1,1,1,1,1,1,1,1,1,1,1,1,1,1,1,1,1,1,1,1,1,1,
1,1,1,1,1,1,1,1,1,1,1,1,1,1,1,1,1,1,1,1,1,1,1,1,1,1,4),(0.,0.015625,0.0234375,
0.03125,0.0390625,0.046875,0.0546875,0.0625,0.0703125,0.078125,0.0859375,
0.09375,0.1015625,0.109375,0.125,0.140625,0.1484375,0.15234375,0.15625,
0.16015625,0.1640625,0.171875,0.1796875,0.1875,0.203125,0.21875,0.234375,
0.2421875,0.25,0.2578125,0.265625,0.28125,0.296875,0.3125,0.328125,0.34375,
0.359375,0.3671875,0.37109375,0.375,0.37890625,0.3828125,0.390625,0.40625,
0.421875,0.4296875,0.4375,0.453125,0.46875,0.484375,0.5,0.515625,0.53125,
0.546875,0.5546875,0.5625,0.5703125,0.578125,0.59375,0.609375,0.6171875,
0.625,0.6328125,0.640625,0.65625,0.671875,0.6796875,0.6875,0.6953125,0.703125,
0.71875,0.734375,0.7421875,0.75,0.7578125,0.765625,0.7734375,0.78125,0.7890625,
0.796875,0.8046875,0.8125,0.8203125,0.828125,0.84375,0.859375,0.8671875,
0.875,0.8828125,0.890625,0.90625,0.921875,0.9375,0.953125,0.96875,0.9765625,
0.984375,1.),.UNSPECIFIED.);
#1067=B_SPLINE_CURVE_WITH_KNOTS('',3,(#20564,#20565,#20566,#20567,#20568,
#20569,#20570),.UNSPECIFIED.,.F.,.F.,(4,1,1,1,4),(5.29374964685745E-18,
0.000466110391549299,0.000932220783098593,0.00139833117464789,0.00186444156619718),
 .UNSPECIFIED.);
#1068=B_SPLINE_CURVE_WITH_KNOTS('',3,(#20575,#20576,#20577,#20578,#20579,
#20580,#20581),.UNSPECIFIED.,.F.,.F.,(4,1,1,1,4),(0.,0.00046618153144794,
0.00093236306289588,0.00139854459434382,0.00186472612579176),
 .UNSPECIFIED.);
#1069=B_SPLINE_CURVE_WITH_KNOTS('',3,(#21058,#21059,#21060,#21061,#21062,
#21063,#21064),.UNSPECIFIED.,.F.,.F.,(4,1,1,1,4),(0.,0.25,0.5,0.75,1.),
 .UNSPECIFIED.);
#1070=B_SPLINE_CURVE_WITH_KNOTS('',3,(#21067,#21068,#21069,#21070,#21071,
#21072,#21073,#21074,#21075,#21076,#21077),.UNSPECIFIED.,.F.,.F.,(4,1,1,
1,1,1,1,1,4),(0.,0.125,0.25,0.375,0.5,0.625,0.75,0.875,1.),
 .UNSPECIFIED.);
#1071=B_SPLINE_CURVE_WITH_KNOTS('',3,(#21078,#21079,#21080,#21081,#21082,
#21083,#21084,#21085,#21086,#21087,#21088),.UNSPECIFIED.,.F.,.F.,(4,1,1,
1,1,1,1,1,4),(0.,0.125,0.25,0.375,0.5,0.625,0.75,0.875,1.),
 .UNSPECIFIED.);
#1072=B_SPLINE_CURVE_WITH_KNOTS('',3,(#21565,#21566,#21567,#21568,#21569,
#21570,#21571),.UNSPECIFIED.,.F.,.F.,(4,1,1,1,4),(0.,0.25,0.5,0.75,1.),
 .UNSPECIFIED.);
#1073=B_SPLINE_CURVE_WITH_KNOTS('',3,(#21573,#21574,#21575,#21576,#21577,
#21578,#21579,#21580,#21581,#21582,#21583,#21584,#21585,#21586,#21587,#21588,
#21589,#21590,#21591,#21592,#21593,#21594,#21595,#21596,#21597,#21598,#21599,
#21600,#21601,#21602,#21603,#21604,#21605,#21606,#21607,#21608,#21609,#21610,
#21611,#21612,#21613,#21614,#21615,#21616,#21617,#21618,#21619,#21620,#21621,
#21622,#21623,#21624,#21625,#21626,#21627,#21628,#21629,#21630,#21631,#21632,
#21633,#21634,#21635,#21636,#21637,#21638,#21639,#21640,#21641,#21642,#21643,
#21644,#21645,#21646,#21647,#21648,#21649,#21650,#21651,#21652,#21653,#21654,
#21655,#21656,#21657,#21658,#21659,#21660,#21661,#21662,#21663,#21664,#21665,
#21666,#21667,#21668,#21669,#21670,#21671,#21672,#21673,#21674,#21675),
 .UNSPECIFIED.,.F.,.F.,(4,1,1,1,1,1,1,1,1,1,1,1,1,1,1,1,1,1,1,1,1,1,1,1,
1,1,1,1,1,1,1,1,1,1,1,1,1,1,1,1,1,1,1,1,1,1,1,1,1,1,1,1,1,1,1,1,1,1,1,1,
1,1,1,1,1,1,1,1,1,1,1,1,1,1,1,1,1,1,1,1,1,1,1,1,1,1,1,1,1,1,1,1,1,1,1,1,
1,1,1,1,4),(0.,0.015625,0.0234375,0.03125,0.0390625,0.046875,0.0546875,
0.0625,0.0703125,0.078125,0.0859375,0.09375,0.1015625,0.109375,0.125,0.140625,
0.1484375,0.15234375,0.15625,0.16015625,0.1640625,0.171875,0.1796875,0.1875,
0.203125,0.21875,0.234375,0.25,0.265625,0.28125,0.296875,0.3046875,0.3125,
0.3203125,0.328125,0.34375,0.359375,0.3671875,0.37109375,0.375,0.37890625,
0.3828125,0.390625,0.40625,0.421875,0.4296875,0.4375,0.4453125,0.453125,
0.4609375,0.46875,0.4765625,0.484375,0.5,0.515625,0.53125,0.546875,0.5546875,
0.5625,0.5703125,0.578125,0.59375,0.609375,0.6171875,0.625,0.6328125,0.640625,
0.65625,0.671875,0.6796875,0.6875,0.6953125,0.703125,0.71875,0.734375,0.7421875,
0.75,0.7578125,0.765625,0.7734375,0.78125,0.7890625,0.796875,0.8046875,
0.8125,0.8203125,0.828125,0.84375,0.859375,0.8671875,0.875,0.8828125,0.890625,
0.90625,0.921875,0.9375,0.953125,0.96875,0.9765625,0.984375,1.),
 .UNSPECIFIED.);
#1074=B_SPLINE_CURVE_WITH_KNOTS('',3,(#22220,#22221,#22222,#22223,#22224,
#22225,#22226),.UNSPECIFIED.,.F.,.F.,(4,1,1,1,4),(0.,0.25,0.5,0.75,1.),
 .UNSPECIFIED.);
#1075=B_SPLINE_CURVE_WITH_KNOTS('',3,(#22229,#22230,#22231,#22232,#22233,
#22234,#22235,#22236,#22237,#22238,#22239),.UNSPECIFIED.,.F.,.F.,(4,1,1,
1,1,1,1,1,4),(0.,0.125,0.25,0.375,0.5,0.625,0.75,0.875,1.),
 .UNSPECIFIED.);
#1076=B_SPLINE_CURVE_WITH_KNOTS('',3,(#22240,#22241,#22242,#22243,#22244,
#22245,#22246,#22247,#22248,#22249,#22250),.UNSPECIFIED.,.F.,.F.,(4,1,1,
1,1,1,1,1,4),(0.,0.125,0.25,0.375,0.5,0.625,0.75,0.875,1.),
 .UNSPECIFIED.);
#1077=B_SPLINE_CURVE_WITH_KNOTS('',3,(#22727,#22728,#22729,#22730,#22731,
#22732,#22733,#22734,#22735,#22736,#22737),.UNSPECIFIED.,.F.,.F.,(4,1,1,
1,1,1,1,1,4),(0.,0.125,0.25,0.375,0.5,0.625,0.75,0.875,1.),
 .UNSPECIFIED.);
#1078=B_SPLINE_CURVE_WITH_KNOTS('',3,(#22739,#22740,#22741,#22742,#22743,
#22744,#22745),.UNSPECIFIED.,.F.,.F.,(4,1,1,1,4),(0.,0.25,0.5,0.75,1.),
 .UNSPECIFIED.);
#1079=B_SPLINE_CURVE_WITH_KNOTS('',3,(#22747,#22748,#22749,#22750,#22751,
#22752,#22753,#22754,#22755,#22756,#22757),.UNSPECIFIED.,.F.,.F.,(4,1,1,
1,1,1,1,1,4),(0.,0.125,0.25,0.375,0.5,0.625,0.75,0.875,1.),
 .UNSPECIFIED.);
#1080=B_SPLINE_CURVE_WITH_KNOTS('',3,(#23234,#23235,#23236,#23237,#23238,
#23239,#23240),.UNSPECIFIED.,.F.,.F.,(4,1,1,1,4),(0.,0.25,0.5,0.75,1.),
 .UNSPECIFIED.);
#1081=B_SPLINE_CURVE_WITH_KNOTS('',3,(#23785,#23786,#23787,#23788,#23789,
#23790,#23791),.UNSPECIFIED.,.F.,.F.,(4,1,1,1,4),(0.,0.25,0.5,0.75,1.),
 .UNSPECIFIED.);
#1082=B_SPLINE_CURVE_WITH_KNOTS('',3,(#24336,#24337,#24338,#24339,#24340,
#24341,#24342,#24343,#24344,#24345,#24346),.UNSPECIFIED.,.F.,.F.,(4,1,1,
1,1,1,1,1,4),(0.,0.125,0.25,0.375,0.5,0.625,0.75,0.875,1.),
 .UNSPECIFIED.);
#1083=B_SPLINE_CURVE_WITH_KNOTS('',3,(#24348,#24349,#24350,#24351,#24352,
#24353,#24354),.UNSPECIFIED.,.F.,.F.,(4,1,1,1,4),(0.,0.25,0.5,0.75,1.),
 .UNSPECIFIED.);
#1084=B_SPLINE_CURVE_WITH_KNOTS('',3,(#24356,#24357,#24358,#24359,#24360,
#24361,#24362,#24363,#24364,#24365,#24366),.UNSPECIFIED.,.F.,.F.,(4,1,1,
1,1,1,1,1,4),(0.,0.125,0.25,0.375,0.5,0.625,0.75,0.875,1.),
 .UNSPECIFIED.);
#1085=B_SPLINE_CURVE_WITH_KNOTS('',3,(#24843,#24844,#24845,#24846,#24847,
#24848,#24849,#24850,#24851,#24852,#24853,#24854,#24855,#24856,#24857,#24858,
#24859,#24860,#24861),.UNSPECIFIED.,.F.,.F.,(4,1,1,1,1,1,1,1,1,1,1,1,1,
1,1,1,4),(0.,0.0625,0.125,0.1875,0.25,0.3125,0.375,0.4375,0.5,0.5625,0.625,
0.6875,0.75,0.8125,0.875,0.9375,1.),.UNSPECIFIED.);
#1086=B_SPLINE_CURVE_WITH_KNOTS('',3,(#24863,#24864,#24865,#24866,#24867,
#24868,#24869,#24870,#24871,#24872,#24873,#24874,#24875,#24876,#24877,#24878,
#24879,#24880,#24881),.UNSPECIFIED.,.F.,.F.,(4,1,1,1,1,1,1,1,1,1,1,1,1,
1,1,1,4),(0.,0.0625,0.125,0.1875,0.25,0.3125,0.375,0.4375,0.5,0.5625,0.625,
0.6875,0.75,0.8125,0.875,0.9375,1.),.UNSPECIFIED.);
#1087=B_SPLINE_CURVE_WITH_KNOTS('',3,(#24883,#24884,#24885,#24886,#24887,
#24888,#24889),.UNSPECIFIED.,.F.,.F.,(4,1,1,1,4),(0.,0.25,0.5,0.75,1.),
 .UNSPECIFIED.);
#1088=B_SPLINE_CURVE_WITH_KNOTS('',3,(#25366,#25367,#25368,#25369,#25370,
#25371,#25372),.UNSPECIFIED.,.F.,.F.,(4,1,1,1,4),(0.,0.25,0.5,0.75,1.),
 .UNSPECIFIED.);
#1089=B_SPLINE_CURVE_WITH_KNOTS('',3,(#25917,#25918,#25919,#25920,#25921,
#25922,#25923),.UNSPECIFIED.,.F.,.F.,(4,1,1,1,4),(0.,0.25,0.5,0.75,1.),
 .UNSPECIFIED.);
#1090=B_SPLINE_CURVE_WITH_KNOTS('',3,(#26468,#26469,#26470,#26471,#26472,
#26473,#26474,#26475,#26476,#26477,#26478,#26479,#26480,#26481,#26482,#26483,
#26484,#26485,#26486),.UNSPECIFIED.,.F.,.F.,(4,1,1,1,1,1,1,1,1,1,1,1,1,
1,1,1,4),(0.,0.0625,0.125,0.1875,0.25,0.3125,0.375,0.4375,0.5,0.5625,0.625,
0.6875,0.75,0.8125,0.875,0.9375,1.),.UNSPECIFIED.);
#1091=B_SPLINE_CURVE_WITH_KNOTS('',3,(#26487,#26488,#26489,#26490,#26491,
#26492,#26493,#26494,#26495,#26496,#26497,#26498,#26499,#26500,#26501,#26502,
#26503,#26504,#26505),.UNSPECIFIED.,.F.,.F.,(4,1,1,1,1,1,1,1,1,1,1,1,1,
1,1,1,4),(0.,0.0625,0.125,0.1875,0.25,0.3125,0.375,0.4375,0.5,0.5625,0.625,
0.6875,0.75,0.8125,0.875,0.9375,1.),.UNSPECIFIED.);
#1092=B_SPLINE_CURVE_WITH_KNOTS('',3,(#27276,#27277,#27278,#27279,#27280,
#27281,#27282,#27283),.UNSPECIFIED.,.F.,.F.,(4,1,1,1,1,4),(0.,0.000509865687280155,
0.00101973137456031,0.00203946274912062,0.00305919412368093,0.00407892549824124),
 .UNSPECIFIED.);
#1093=B_SPLINE_CURVE_WITH_KNOTS('',3,(#27471,#27472,#27473,#27474),
 .UNSPECIFIED.,.F.,.F.,(4,4),(0.,0.00208376980020791),.UNSPECIFIED.);
#1094=B_SPLINE_CURVE_WITH_KNOTS('',3,(#27713,#27714,#27715,#27716,#27717,
#27718,#27719,#27720),.UNSPECIFIED.,.F.,.F.,(4,1,1,1,1,4),(0.,0.00114238418818656,
0.00228476837637312,0.00342715256455968,0.00399834465865296,0.00456953675274624),
 .UNSPECIFIED.);
#1095=B_SPLINE_CURVE_WITH_KNOTS('',3,(#28043,#28044,#28045,#28046,#28047,
#28048),.UNSPECIFIED.,.F.,.F.,(4,1,1,4),(0.,0.00491511497907896,0.00737267246861844,
0.00983022995815793),.UNSPECIFIED.);
#1096=B_SPLINE_CURVE_WITH_KNOTS('',3,(#28227,#28228,#28229,#28230,#28231,
#28232),.UNSPECIFIED.,.F.,.F.,(4,1,1,4),(1.86835436258807E-17,0.00537056638515156,
0.00805584957772733,0.0107411327703031),.UNSPECIFIED.);
#1097=B_SPLINE_CURVE_WITH_KNOTS('',3,(#28493,#28494,#28495,#28496,#28497),
 .UNSPECIFIED.,.F.,.F.,(4,1,4),(0.,0.0044135208761771,0.0088270417523542),
 .UNSPECIFIED.);
#1098=B_SPLINE_CURVE_WITH_KNOTS('',3,(#30747,#30748,#30749,#30750,#30751),
 .UNSPECIFIED.,.F.,.F.,(4,1,4),(0.,0.000813104509733637,0.00162620901946727),
 .UNSPECIFIED.);
#1099=B_SPLINE_CURVE_WITH_KNOTS('',3,(#30818,#30819,#30820,#30821,#30822),
 .UNSPECIFIED.,.F.,.F.,(4,1,4),(0.,0.000813104509733632,0.00162620901946726),
 .UNSPECIFIED.);
#1100=B_SPLINE_CURVE_WITH_KNOTS('',3,(#32285,#32286,#32287,#32288),
 .UNSPECIFIED.,.F.,.F.,(4,4),(0.,0.00676281690826917),.UNSPECIFIED.);
#1101=B_SPLINE_CURVE_WITH_KNOTS('',3,(#32585,#32586,#32587,#32588,#32589),
 .UNSPECIFIED.,.F.,.F.,(4,1,4),(0.,0.00441087142557483,0.00882174285114967),
 .UNSPECIFIED.);
#1102=B_SPLINE_CURVE_WITH_KNOTS('',3,(#32936,#32937,#32938,#32939,#32940,
#32941,#32942,#32943),.UNSPECIFIED.,.F.,.F.,(4,1,1,1,1,4),(5.05159101305033E-17,
0.000510091042055662,0.00102018208411127,0.0020403641682225,0.00306054625233372,
0.00408072833644494),.UNSPECIFIED.);
#1103=B_SPLINE_CURVE_WITH_KNOTS('',3,(#33096,#33097,#33098,#33099),
 .UNSPECIFIED.,.F.,.F.,(4,4),(6.05912861432085E-17,0.00208718873665751),
 .UNSPECIFIED.);
#1104=B_SPLINE_CURVE_WITH_KNOTS('',3,(#33296,#33297,#33298,#33299,#33300,
#33301,#33302,#33303),.UNSPECIFIED.,.F.,.F.,(4,1,1,1,1,4),(0.,0.00114202028985642,
0.00228404057971283,0.00342606086956925,0.00399707101449746,0.00456808115942567),
 .UNSPECIFIED.);
#1105=B_SPLINE_CURVE_WITH_KNOTS('',3,(#33362,#33363,#33364,#33365),
 .UNSPECIFIED.,.F.,.F.,(4,4),(0.,0.000338478963180613),.UNSPECIFIED.);
#1106=B_SPLINE_CURVE_WITH_KNOTS('',3,(#33404,#33405,#33406,#33407,#33408,
#33409,#33410,#33411),.UNSPECIFIED.,.F.,.F.,(4,1,1,1,1,4),(0.,0.000572817003192511,
0.00114563400638502,0.00229126801277004,0.00343690201915507,0.00458253602554009),
 .UNSPECIFIED.);
#1107=B_SPLINE_CURVE_WITH_KNOTS('',3,(#33446,#33447,#33448,#33449),
 .UNSPECIFIED.,.F.,.F.,(4,4),(8.39720847001417E-16,0.00208289890788513),
 .UNSPECIFIED.);
#1108=B_SPLINE_CURVE_WITH_KNOTS('',3,(#33462,#33463,#33464,#33465,#33466,
#33467,#33468,#33469),.UNSPECIFIED.,.F.,.F.,(4,1,1,1,1,4),(4.60907911065496E-11,
0.000959696893981847,0.0019193937418729,0.00287909058976396,0.00335893901370949,
0.00383878743765501),.UNSPECIFIED.);
#1109=B_SPLINE_CURVE_WITH_KNOTS('',3,(#33682,#33683,#33684,#33685,#33686),
 .UNSPECIFIED.,.F.,.F.,(4,1,4),(1.76851098641564E-19,0.00223125534297384,
0.00446251068594769),.UNSPECIFIED.);
#1110=B_SPLINE_CURVE_WITH_KNOTS('',3,(#37214,#37215,#37216,#37217),
 .UNSPECIFIED.,.F.,.F.,(4,4),(0.,1.),.UNSPECIFIED.);
#1111=B_SPLINE_CURVE_WITH_KNOTS('',3,(#37220,#37221,#37222,#37223,#37224,
#37225,#37226,#37227,#37228,#37229,#37230,#37231,#37232,#37233,#37234,#37235,
#37236,#37237,#37238,#37239,#37240,#37241,#37242,#37243,#37244,#37245,#37246,
#37247,#37248,#37249,#37250,#37251,#37252,#37253,#37254,#37255,#37256,#37257,
#37258,#37259,#37260,#37261,#37262,#37263,#37264,#37265,#37266,#37267,#37268,
#37269,#37270,#37271,#37272,#37273,#37274,#37275,#37276,#37277,#37278,#37279,
#37280,#37281,#37282,#37283,#37284,#37285,#37286,#37287,#37288,#37289,#37290,
#37291,#37292,#37293,#37294,#37295,#37296,#37297,#37298,#37299,#37300,#37301,
#37302,#37303,#37304,#37305,#37306,#37307,#37308,#37309,#37310,#37311,#37312,
#37313,#37314,#37315,#37316,#37317,#37318,#37319,#37320,#37321,#37322,#37323,
#37324,#37325,#37326,#37327,#37328,#37329,#37330,#37331,#37332,#37333),
 .UNSPECIFIED.,.F.,.F.,(4,1,1,1,1,1,1,1,1,1,1,1,1,1,1,1,1,1,1,1,1,1,1,1,
1,1,1,1,1,1,1,1,1,1,1,1,1,1,1,1,1,1,1,1,1,1,1,1,1,1,1,1,1,1,1,1,1,1,1,1,
1,1,1,1,1,1,1,1,1,1,1,1,1,1,1,1,1,1,1,1,1,1,1,1,1,1,1,1,1,1,1,1,1,1,1,1,
1,1,1,1,1,1,1,1,1,1,1,1,1,1,1,4),(0.,0.0078125,0.015625,0.0234375,0.03125,
0.046875,0.0546875,0.0625,0.0703125,0.078125,0.0859375,0.09375,0.109375,
0.1171875,0.125,0.1328125,0.140625,0.1484375,0.15625,0.171875,0.1796875,
0.1875,0.1953125,0.203125,0.2109375,0.21875,0.234375,0.2421875,0.25,0.2578125,
0.265625,0.2734375,0.28125,0.296875,0.3046875,0.3125,0.3203125,0.328125,
0.3359375,0.34375,0.359375,0.3671875,0.375,0.3828125,0.390625,0.3984375,
0.40625,0.421875,0.4296875,0.4375,0.4453125,0.453125,0.4609375,0.46875,
0.484375,0.4921875,0.5,0.515625,0.5234375,0.53125,0.546875,0.5546875,0.5625,
0.5703125,0.578125,0.5859375,0.59375,0.609375,0.6171875,0.625,0.6328125,
0.640625,0.6484375,0.65625,0.671875,0.6796875,0.6875,0.6953125,0.703125,
0.7109375,0.71875,0.734375,0.7421875,0.75,0.7578125,0.765625,0.7734375,
0.78125,0.796875,0.8046875,0.8125,0.8203125,0.828125,0.8359375,0.84375,
0.859375,0.8671875,0.875,0.8828125,0.890625,0.8984375,0.90625,0.921875,
0.9296875,0.9375,0.9453125,0.953125,0.9609375,0.96875,0.984375,0.9921875,
1.),.UNSPECIFIED.);
#1112=B_SPLINE_CURVE_WITH_KNOTS('',3,(#37335,#37336,#37337,#37338),
 .UNSPECIFIED.,.F.,.F.,(4,4),(0.,1.),.UNSPECIFIED.);
#1113=B_SPLINE_CURVE_WITH_KNOTS('',3,(#37340,#37341,#37342,#37343,#37344),
 .UNSPECIFIED.,.F.,.F.,(4,1,4),(3.80821390671777E-7,0.500000190410695,1.),
 .UNSPECIFIED.);
#1114=B_SPLINE_CURVE_WITH_KNOTS('',3,(#37346,#37347,#37348,#37349,#37350),
 .UNSPECIFIED.,.F.,.F.,(4,1,4),(0.,0.5,1.),.UNSPECIFIED.);
#1115=B_SPLINE_CURVE_WITH_KNOTS('',3,(#37352,#37353,#37354,#37355,#37356,
#37357,#37358,#37359,#37360,#37361,#37362),.UNSPECIFIED.,.F.,.F.,(4,1,1,
1,1,1,1,1,4),(0.,0.125,0.25,0.375,0.5,0.625,0.75,0.875,1.),
 .UNSPECIFIED.);
#1116=B_SPLINE_CURVE_WITH_KNOTS('',3,(#37364,#37365,#37366,#37367,#37368,
#37369,#37370,#37371,#37372,#37373,#37374),.UNSPECIFIED.,.F.,.F.,(4,1,1,
1,1,1,1,1,4),(0.,0.125,0.25,0.375,0.5,0.625,0.75,0.875,1.),
 .UNSPECIFIED.);
#1117=B_SPLINE_CURVE_WITH_KNOTS('',3,(#37376,#37377,#37378,#37379,#37380,
#37381,#37382,#37383,#37384,#37385,#37386),.UNSPECIFIED.,.F.,.F.,(4,1,1,
1,1,1,1,1,4),(0.,0.125,0.25,0.375,0.5,0.625,0.75,0.875,1.),
 .UNSPECIFIED.);
#1118=B_SPLINE_CURVE_WITH_KNOTS('',3,(#37388,#37389,#37390,#37391,#37392,
#37393,#37394,#37395,#37396,#37397,#37398),.UNSPECIFIED.,.F.,.F.,(4,1,1,
1,1,1,1,1,4),(0.,0.125,0.25,0.375,0.5,0.625,0.75,0.875,1.),
 .UNSPECIFIED.);
#1119=B_SPLINE_CURVE_WITH_KNOTS('',3,(#37400,#37401,#37402,#37403,#37404,
#37405,#37406,#37407,#37408,#37409,#37410),.UNSPECIFIED.,.F.,.F.,(4,1,1,
1,1,1,1,1,4),(0.,0.125,0.25,0.375,0.5,0.625,0.75,0.875,1.),
 .UNSPECIFIED.);
#1120=B_SPLINE_CURVE_WITH_KNOTS('',3,(#37412,#37413,#37414,#37415,#37416,
#37417,#37418),.UNSPECIFIED.,.F.,.F.,(4,1,1,1,4),(0.,0.25,0.5,0.75,1.),
 .UNSPECIFIED.);
#1121=B_SPLINE_CURVE_WITH_KNOTS('',3,(#37420,#37421,#37422,#37423,#37424),
 .UNSPECIFIED.,.F.,.F.,(4,1,4),(0.,0.499999802342316,0.999999604684632),
 .UNSPECIFIED.);
#1122=B_SPLINE_CURVE_WITH_KNOTS('',3,(#37426,#37427,#37428,#37429,#37430),
 .UNSPECIFIED.,.F.,.F.,(4,1,4),(0.,0.49999980888236,0.99999961776472),
 .UNSPECIFIED.);
#1123=B_SPLINE_CURVE_WITH_KNOTS('',3,(#37433,#37434,#37435,#37436),
 .UNSPECIFIED.,.F.,.F.,(4,4),(1.04486053410473E-7,0.999999895529088),
 .UNSPECIFIED.);
#1124=B_SPLINE_CURVE_WITH_KNOTS('',3,(#37437,#37438,#37439,#37440),
 .UNSPECIFIED.,.F.,.F.,(4,4),(0.,1.),.UNSPECIFIED.);
#1125=B_SPLINE_CURVE_WITH_KNOTS('',3,(#37442,#37443,#37444,#37445),
 .UNSPECIFIED.,.F.,.F.,(4,4),(0.,0.999999872405437),.UNSPECIFIED.);
#1126=B_SPLINE_CURVE_WITH_KNOTS('',3,(#37449,#37450,#37451,#37452),
 .UNSPECIFIED.,.F.,.F.,(4,4),(1.27661041249407E-7,0.999999872030063),
 .UNSPECIFIED.);
#1127=B_SPLINE_CURVE_WITH_KNOTS('',3,(#37455,#37456,#37457,#37458),
 .UNSPECIFIED.,.F.,.F.,(4,4),(0.,1.),.UNSPECIFIED.);
#1128=B_SPLINE_CURVE_WITH_KNOTS('',3,(#37459,#37460,#37461,#37462),
 .UNSPECIFIED.,.F.,.F.,(4,4),(1.14719167408304E-7,1.),.UNSPECIFIED.);
#1129=B_SPLINE_CURVE_WITH_KNOTS('',3,(#37464,#37465,#37466,#37467),
 .UNSPECIFIED.,.F.,.F.,(4,4),(0.,1.),.UNSPECIFIED.);
#1130=B_SPLINE_CURVE_WITH_KNOTS('',3,(#37469,#37470,#37471,#37472),
 .UNSPECIFIED.,.F.,.F.,(4,4),(0.,1.),.UNSPECIFIED.);
#1131=B_SPLINE_CURVE_WITH_KNOTS('',3,(#37474,#37475,#37476,#37477),
 .UNSPECIFIED.,.F.,.F.,(4,4),(0.,1.),.UNSPECIFIED.);
#1132=B_SPLINE_CURVE_WITH_KNOTS('',3,(#38519,#38520,#38521,#38522,#38523,
#38524,#38525),.UNSPECIFIED.,.F.,.F.,(4,1,1,1,4),(0.,0.25,0.5,0.75,1.),
 .UNSPECIFIED.);
#1133=B_SPLINE_CURVE_WITH_KNOTS('',3,(#38527,#38528,#38529,#38530,#38531,
#38532,#38533,#38534,#38535,#38536,#38537),.UNSPECIFIED.,.F.,.F.,(4,1,1,
1,1,1,1,1,4),(0.,0.125,0.25,0.375,0.5,0.625,0.75,0.875,1.),
 .UNSPECIFIED.);
#1134=B_SPLINE_CURVE_WITH_KNOTS('',3,(#38539,#38540,#38541,#38542,#38543,
#38544,#38545,#38546,#38547,#38548,#38549),.UNSPECIFIED.,.F.,.F.,(4,1,1,
1,1,1,1,1,4),(0.,0.125,0.25,0.375,0.5,0.625,0.75,0.875,1.),
 .UNSPECIFIED.);
#1135=B_SPLINE_CURVE_WITH_KNOTS('',3,(#38551,#38552,#38553,#38554,#38555,
#38556,#38557,#38558,#38559,#38560,#38561),.UNSPECIFIED.,.F.,.F.,(4,1,1,
1,1,1,1,1,4),(0.,0.125,0.25,0.375,0.5,0.625,0.75,0.875,1.),
 .UNSPECIFIED.);
#1136=B_SPLINE_CURVE_WITH_KNOTS('',3,(#38563,#38564,#38565,#38566,#38567,
#38568,#38569,#38570,#38571,#38572,#38573),.UNSPECIFIED.,.F.,.F.,(4,1,1,
1,1,1,1,1,4),(0.,0.125,0.25,0.375,0.5,0.625,0.75,0.875,1.),
 .UNSPECIFIED.);
#1137=B_SPLINE_CURVE_WITH_KNOTS('',3,(#38575,#38576,#38577,#38578,#38579,
#38580,#38581,#38582,#38583,#38584,#38585),.UNSPECIFIED.,.F.,.F.,(4,1,1,
1,1,1,1,1,4),(0.,0.125,0.25,0.375,0.5,0.625,0.75,0.875,1.),
 .UNSPECIFIED.);
#1138=B_SPLINE_CURVE_WITH_KNOTS('',3,(#38587,#38588,#38589,#38590,#38591),
 .UNSPECIFIED.,.F.,.F.,(4,1,4),(0.,0.5,1.),.UNSPECIFIED.);
#1139=B_SPLINE_CURVE_WITH_KNOTS('',3,(#38592,#38593,#38594,#38595),
 .UNSPECIFIED.,.F.,.F.,(4,4),(0.,1.),.UNSPECIFIED.);
#1140=B_SPLINE_CURVE_WITH_KNOTS('',3,(#38597,#38598,#38599,#38600,#38601,
#38602,#38603,#38604,#38605,#38606,#38607,#38608,#38609,#38610,#38611,#38612,
#38613,#38614,#38615,#38616,#38617,#38618,#38619,#38620,#38621,#38622,#38623,
#38624,#38625,#38626,#38627,#38628,#38629,#38630,#38631,#38632,#38633,#38634,
#38635,#38636,#38637,#38638,#38639,#38640,#38641,#38642,#38643,#38644,#38645,
#38646,#38647,#38648,#38649,#38650,#38651,#38652,#38653,#38654,#38655,#38656,
#38657,#38658,#38659,#38660,#38661,#38662,#38663,#38664,#38665,#38666,#38667,
#38668,#38669,#38670,#38671,#38672,#38673,#38674,#38675,#38676,#38677,#38678,
#38679,#38680,#38681,#38682,#38683,#38684,#38685,#38686,#38687,#38688,#38689,
#38690,#38691,#38692,#38693,#38694,#38695,#38696,#38697,#38698,#38699,#38700,
#38701,#38702,#38703,#38704,#38705,#38706),.UNSPECIFIED.,.F.,.F.,(4,1,1,
1,1,1,1,1,1,1,1,1,1,1,1,1,1,1,1,1,1,1,1,1,1,1,1,1,1,1,1,1,1,1,1,1,1,1,1,
1,1,1,1,1,1,1,1,1,1,1,1,1,1,1,1,1,1,1,1,1,1,1,1,1,1,1,1,1,1,1,1,1,1,1,1,
1,1,1,1,1,1,1,1,1,1,1,1,1,1,1,1,1,1,1,1,1,1,1,1,1,1,1,1,1,1,1,1,4),(0.,
0.03125,0.046875,0.0546875,0.0625,0.0703125,0.078125,0.0859375,0.09375,
0.1015625,0.109375,0.1171875,0.125,0.1328125,0.140625,0.15625,0.1640625,
0.171875,0.1796875,0.1875,0.203125,0.2109375,0.21875,0.2265625,0.234375,
0.2421875,0.25,0.265625,0.2734375,0.28125,0.2890625,0.296875,0.3125,0.3203125,
0.328125,0.3359375,0.34375,0.3515625,0.359375,0.375,0.3828125,0.390625,
0.3984375,0.40625,0.421875,0.4296875,0.4375,0.4453125,0.453125,0.4609375,
0.46875,0.4765625,0.484375,0.4921875,0.5,0.515625,0.5234375,0.53125,0.546875,
0.5546875,0.5625,0.5703125,0.578125,0.59375,0.6015625,0.609375,0.6171875,
0.625,0.6328125,0.640625,0.6484375,0.65625,0.6640625,0.671875,0.6796875,
0.6875,0.703125,0.7109375,0.71875,0.7265625,0.734375,0.7421875,0.75,0.7578125,
0.765625,0.7734375,0.78125,0.7890625,0.796875,0.8125,0.8203125,0.828125,
0.8359375,0.84375,0.859375,0.8671875,0.875,0.8828125,0.890625,0.8984375,
0.90625,0.921875,0.9296875,0.9375,0.9453125,0.953125,0.96875,1.),
 .UNSPECIFIED.);
#1141=B_SPLINE_CURVE_WITH_KNOTS('',3,(#38719,#38720,#38721,#38722),
 .UNSPECIFIED.,.F.,.F.,(4,4),(0.,1.),.UNSPECIFIED.);
#1142=B_SPLINE_CURVE_WITH_KNOTS('',3,(#38724,#38725,#38726,#38727,#38728,
#38729),.UNSPECIFIED.,.F.,.F.,(4,1,1,4),(0.,0.25,0.5,1.),.UNSPECIFIED.);
#1143=B_SPLINE_CURVE_WITH_KNOTS('',3,(#38760,#38761,#38762,#38763),
 .UNSPECIFIED.,.F.,.F.,(4,4),(0.,1.),.UNSPECIFIED.);
#1144=B_SPLINE_CURVE_WITH_KNOTS('',3,(#38764,#38765,#38766,#38767,#38768),
 .UNSPECIFIED.,.F.,.F.,(4,1,4),(0.,0.5,1.),.UNSPECIFIED.);
#1145=B_SPLINE_CURVE_WITH_KNOTS('',3,(#38798,#38799,#38800,#38801,#38802,
#38803,#38804),.UNSPECIFIED.,.F.,.F.,(4,1,1,1,4),(0.,0.00242728027803591,
0.00485456055607181,0.00728184083410772,0.00970912111214362),
 .UNSPECIFIED.);
#1146=B_SPLINE_CURVE_WITH_KNOTS('',3,(#39435,#39436,#39437,#39438,#39439,
#39440,#39441),.UNSPECIFIED.,.F.,.F.,(4,1,1,1,4),(0.,0.00298225036522322,
0.00596450073044643,0.00894675109566965,0.0119290014608929),
 .UNSPECIFIED.);
#1147=B_SPLINE_CURVE_WITH_KNOTS('',3,(#40277,#40278,#40279,#40280),
 .UNSPECIFIED.,.F.,.F.,(4,4),(6.48381396703939E-18,0.00339130657297538),
 .UNSPECIFIED.);
#1148=B_SPLINE_CURVE_WITH_KNOTS('',3,(#41775,#41776,#41777,#41778,#41779),
 .UNSPECIFIED.,.F.,.F.,(4,1,4),(-0.000755554523882612,6.89428958346064E-7,
0.000756933381799304),.UNSPECIFIED.);
#1149=B_SPLINE_CURVE_WITH_KNOTS('',3,(#41969,#41970,#41971,#41972,#41973),
 .UNSPECIFIED.,.F.,.F.,(4,1,4),(0.,0.5,1.),.UNSPECIFIED.);
#1150=B_SPLINE_CURVE_WITH_KNOTS('',3,(#41978,#41979,#41980,#41981),
 .UNSPECIFIED.,.F.,.F.,(4,4),(0.,1.),.UNSPECIFIED.);
#1151=B_SPLINE_CURVE_WITH_KNOTS('',3,(#41983,#41984,#41985,#41986,#41987,
#41988,#41989,#41990),.UNSPECIFIED.,.F.,.F.,(4,1,1,1,1,4),(0.,0.25,0.5,
0.625,0.75,1.),.UNSPECIFIED.);
#1152=B_SPLINE_CURVE_WITH_KNOTS('',3,(#41992,#41993,#41994,#41995,#41996,
#41997,#41998,#41999,#42000,#42001,#42002,#42003,#42004),.UNSPECIFIED.,
 .F.,.F.,(4,1,1,1,1,1,1,1,1,1,4),(0.,0.125,0.25,0.375,0.5,0.5625,0.625,
0.6875,0.75,0.875,1.),.UNSPECIFIED.);
#1153=B_SPLINE_CURVE_WITH_KNOTS('',3,(#42006,#42007,#42008,#42009),
 .UNSPECIFIED.,.F.,.F.,(4,4),(0.,1.),.UNSPECIFIED.);
#1154=B_SPLINE_CURVE_WITH_KNOTS('',3,(#42070,#42071,#42072,#42073,#42074,
#42075,#42076,#42077,#42078,#42079,#42080,#42081,#42082),.UNSPECIFIED.,
 .F.,.F.,(4,1,1,1,1,1,1,1,1,1,4),(0.,0.125,0.1875,0.25,0.3125,0.375,0.4375,
0.5,0.625,0.75,1.),.UNSPECIFIED.);
#1155=B_SPLINE_CURVE_WITH_KNOTS('',3,(#42085,#42086,#42087,#42088),
 .UNSPECIFIED.,.F.,.F.,(4,4),(0.,1.),.UNSPECIFIED.);
#1156=B_SPLINE_CURVE_WITH_KNOTS('',3,(#42090,#42091,#42092,#42093),
 .UNSPECIFIED.,.F.,.F.,(4,4),(0.,1.),.UNSPECIFIED.);
#1157=B_SPLINE_CURVE_WITH_KNOTS('',3,(#42094,#42095,#42096,#42097),
 .UNSPECIFIED.,.F.,.F.,(4,4),(0.,1.),.UNSPECIFIED.);
#1158=B_SPLINE_CURVE_WITH_KNOTS('',3,(#42099,#42100,#42101,#42102,#42103,
#42104,#42105,#42106,#42107),.UNSPECIFIED.,.F.,.F.,(4,1,1,1,1,1,4),(0.,
0.25,0.375,0.5,0.625,0.75,1.),.UNSPECIFIED.);
#1159=B_SPLINE_CURVE_WITH_KNOTS('',3,(#42109,#42110,#42111,#42112),
 .UNSPECIFIED.,.F.,.F.,(4,4),(0.,1.),.UNSPECIFIED.);
#1160=B_SPLINE_CURVE_WITH_KNOTS('',3,(#42137,#42138,#42139,#42140),
 .UNSPECIFIED.,.F.,.F.,(4,4),(0.,1.),.UNSPECIFIED.);
#1161=B_SPLINE_CURVE_WITH_KNOTS('',3,(#42144,#42145,#42146,#42147,#42148),
 .UNSPECIFIED.,.F.,.F.,(4,1,4),(0.,0.5,1.),.UNSPECIFIED.);
#1162=B_SPLINE_CURVE_WITH_KNOTS('',3,(#42173,#42174,#42175,#42176),
 .UNSPECIFIED.,.F.,.F.,(4,4),(0.,1.),.UNSPECIFIED.);
#1163=B_SPLINE_CURVE_WITH_KNOTS('',3,(#42181,#42182,#42183,#42184,#42185),
 .UNSPECIFIED.,.F.,.F.,(4,1,4),(0.,0.5,1.),.UNSPECIFIED.);
#1164=B_SPLINE_CURVE_WITH_KNOTS('',3,(#42187,#42188,#42189,#42190,#42191,
#42192,#42193,#42194,#42195,#42196,#42197,#42198),.UNSPECIFIED.,.F.,.F.,
(4,1,1,1,1,1,1,1,1,4),(0.,0.0625,0.125,0.25,0.375,0.4375,0.5,0.625,0.75,
1.),.UNSPECIFIED.);
#1165=B_SPLINE_CURVE_WITH_KNOTS('',3,(#42200,#42201,#42202,#42203,#42204,
#42205,#42206,#42207,#42208,#42209),.UNSPECIFIED.,.F.,.F.,(4,1,1,1,1,1,
1,4),(0.,0.25,0.375,0.5,0.625,0.75,0.875,1.),.UNSPECIFIED.);
#1166=B_SPLINE_CURVE_WITH_KNOTS('',3,(#42211,#42212,#42213,#42214),
 .UNSPECIFIED.,.F.,.F.,(4,4),(0.,1.),.UNSPECIFIED.);
#1167=B_SPLINE_CURVE_WITH_KNOTS('',3,(#42251,#42252,#42253,#42254,#42255,
#42256,#42257,#42258,#42259),.UNSPECIFIED.,.F.,.F.,(4,1,1,1,1,1,4),(0.,
0.25,0.375,0.5,0.75,0.875,1.),.UNSPECIFIED.);
#1168=B_SPLINE_CURVE_WITH_KNOTS('',3,(#42262,#42263,#42264,#42265),
 .UNSPECIFIED.,.F.,.F.,(4,4),(0.,1.),.UNSPECIFIED.);
#1169=B_SPLINE_CURVE_WITH_KNOTS('',3,(#42266,#42267,#42268,#42269),
 .UNSPECIFIED.,.F.,.F.,(4,4),(0.,1.),.UNSPECIFIED.);
#1170=B_SPLINE_CURVE_WITH_KNOTS('',3,(#42271,#42272,#42273,#42274),
 .UNSPECIFIED.,.F.,.F.,(4,4),(0.,1.),.UNSPECIFIED.);
#1171=B_SPLINE_CURVE_WITH_KNOTS('',3,(#42276,#42277,#42278,#42279,#42280,
#42281,#42282,#42283),.UNSPECIFIED.,.F.,.F.,(4,1,1,1,1,4),(0.,0.125,0.25,
0.5,0.75,1.),.UNSPECIFIED.);
#1172=B_SPLINE_CURVE_WITH_KNOTS('',3,(#42285,#42286,#42287,#42288),
 .UNSPECIFIED.,.F.,.F.,(4,4),(0.,1.),.UNSPECIFIED.);
#1173=B_SPLINE_CURVE_WITH_KNOTS('',3,(#42313,#42314,#42315,#42316,#42317),
 .UNSPECIFIED.,.F.,.F.,(4,1,4),(0.,0.5,1.),.UNSPECIFIED.);
#1174=B_SPLINE_CURVE_WITH_KNOTS('',3,(#42321,#42322,#42323,#42324),
 .UNSPECIFIED.,.F.,.F.,(4,4),(0.,1.),.UNSPECIFIED.);
#1175=B_SPLINE_CURVE_WITH_KNOTS('',3,(#42853,#42854,#42855,#42856,#42857,
#42858,#42859,#42860,#42861,#42862,#42863,#42864,#42865,#42866,#42867,#42868,
#42869,#42870,#42871,#42872,#42873,#42874,#42875,#42876,#42877,#42878,#42879,
#42880,#42881,#42882,#42883,#42884,#42885,#42886,#42887,#42888,#42889,#42890,
#42891,#42892,#42893,#42894,#42895,#42896,#42897,#42898,#42899,#42900,#42901,
#42902,#42903,#42904,#42905,#42906,#42907,#42908,#42909,#42910,#42911,#42912,
#42913,#42914,#42915,#42916,#42917,#42918,#42919,#42920,#42921,#42922,#42923,
#42924,#42925,#42926,#42927,#42928,#42929,#42930,#42931,#42932,#42933,#42934,
#42935,#42936,#42937,#42938,#42939,#42940,#42941,#42942,#42943,#42944,#42945,
#42946,#42947,#42948,#42949,#42950,#42951),.UNSPECIFIED.,.F.,.F.,(4,1,1,
1,1,1,1,1,1,1,1,1,1,1,1,1,1,1,1,1,1,1,1,1,1,1,1,1,1,1,1,1,1,1,1,1,1,1,1,
1,1,1,1,1,1,1,1,1,1,1,1,1,1,1,1,1,1,1,1,1,1,1,1,1,1,1,1,1,1,1,1,1,1,1,1,
1,1,1,1,1,1,1,1,1,1,1,1,1,1,1,1,1,1,1,1,1,4),(1.77834376359015E-8,0.0156250175055714,
0.0312500172277052,0.046875016949839,0.0546875168109059,0.0625000166719728,
0.0703125165330397,0.0781250163941066,0.0937500161162403,0.109375015838374,
0.125000015560508,0.140625015282642,0.156250015004775,0.171875014726909,
0.179687514587976,0.18359376451851,0.187500014449043,0.191406264379577,
0.19531251431011,0.203125014171177,0.218750013893311,0.234375013615444,
0.242187513476511,0.250000013337578,0.257812513198645,0.265625013059712,
0.281250012781846,0.312500012226113,0.343750011670381,0.359375011392515,
0.367187511253582,0.375000011114649,0.382812510975715,0.390625010836782,
0.406250010558916,0.437500010003184,0.468750009447451,0.484375009169585,
0.492187509030652,0.496093758961185,0.500000008891719,0.503906258822252,
0.507812508752786,0.515625008613853,0.531250008335986,0.562500007780254,
0.578125007502388,0.593750007224522,0.601562507085588,0.609375006946655,
0.617187506807722,0.621093756738256,0.623046881703522,0.625000006668789,
0.626953131634056,0.628906256599323,0.632812506529856,0.640625006390923,
0.656250006113057,0.664062505974124,0.671875005835191,0.679687505696257,
0.683593755626791,0.687500005557324,0.691406255487858,0.695312505418391,
0.703125005279458,0.718750005001592,0.734375004723726,0.742187504584793,
0.746093754515326,0.750000004445859,0.753906254376393,0.757812504306926,
0.765625004167993,0.781250003890127,0.789062503751194,0.796875003612261,
0.804687503473328,0.808593753403861,0.810546878369128,0.812500003334395,
0.814453128299661,0.816406253264928,0.820312503195461,0.828125003056528,
0.835937502917595,0.843750002778662,0.859375002500796,0.867187502361863,
0.87500000222293,0.882812502083997,0.890625001945063,0.906250001667197,
0.937500001111465,0.968750000555732,1.),.UNSPECIFIED.);
#1176=B_SPLINE_CURVE_WITH_KNOTS('',3,(#42954,#42955,#42956,#42957,#42958,
#42959),.UNSPECIFIED.,.F.,.F.,(4,1,1,4),(0.,0.25,0.5,1.),.UNSPECIFIED.);
#1177=B_SPLINE_CURVE_WITH_KNOTS('',3,(#42960,#42961,#42962,#42963,#42964,
#42965,#42966,#42967,#42968,#42969,#42970,#42971,#42972,#42973,#42974,#42975,
#42976,#42977,#42978,#42979,#42980,#42981,#42982,#42983,#42984,#42985,#42986,
#42987,#42988,#42989,#42990,#42991,#42992,#42993,#42994,#42995,#42996,#42997,
#42998,#42999,#43000,#43001,#43002,#43003,#43004,#43005,#43006,#43007,#43008,
#43009,#43010,#43011,#43012,#43013,#43014,#43015,#43016,#43017,#43018,#43019,
#43020,#43021,#43022,#43023,#43024,#43025,#43026,#43027,#43028,#43029,#43030,
#43031,#43032,#43033,#43034,#43035,#43036,#43037,#43038,#43039,#43040,#43041,
#43042,#43043,#43044,#43045,#43046,#43047,#43048,#43049,#43050,#43051,#43052,
#43053,#43054,#43055,#43056,#43057,#43058,#43059,#43060,#43061,#43062,#43063,
#43064,#43065,#43066,#43067,#43068,#43069,#43070,#43071,#43072,#43073,#43074,
#43075,#43076,#43077),.UNSPECIFIED.,.F.,.F.,(4,1,1,1,1,1,1,1,1,1,1,1,1,
1,1,1,1,1,1,1,1,1,1,1,1,1,1,1,1,1,1,1,1,1,1,1,1,1,1,1,1,1,1,1,1,1,1,1,1,
1,1,1,1,1,1,1,1,1,1,1,1,1,1,1,1,1,1,1,1,1,1,1,1,1,1,1,1,1,1,1,1,1,1,1,1,
1,1,1,1,1,1,1,1,1,1,1,1,1,1,1,1,1,1,1,1,1,1,1,1,1,1,1,1,1,1,4),(0.,0.015625,
0.0234375,0.03125,0.0390625,0.046875,0.0546875,0.0625,0.078125,0.0859375,
0.09375,0.1015625,0.109375,0.1171875,0.125,0.140625,0.1484375,0.15625,0.1640625,
0.171875,0.1796875,0.1875,0.203125,0.2109375,0.21875,0.2265625,0.234375,
0.2421875,0.25,0.2578125,0.265625,0.2734375,0.28125,0.2890625,0.296875,
0.3125,0.3203125,0.328125,0.3359375,0.34375,0.3515625,0.359375,0.375,0.3828125,
0.390625,0.3984375,0.40625,0.4140625,0.421875,0.4375,0.4453125,0.453125,
0.4609375,0.46875,0.4765625,0.484375,0.4921875,0.5,0.515625,0.5234375,0.53125,
0.5390625,0.546875,0.5546875,0.5625,0.578125,0.5859375,0.59375,0.6015625,
0.609375,0.6171875,0.625,0.6328125,0.640625,0.6484375,0.65625,0.6640625,
0.671875,0.6875,0.6953125,0.703125,0.7109375,0.71875,0.7265625,0.734375,
0.75,0.7578125,0.765625,0.7734375,0.78125,0.7890625,0.796875,0.8125,0.8203125,
0.828125,0.8359375,0.84375,0.8515625,0.859375,0.8671875,0.875,0.8828125,
0.890625,0.8984375,0.90625,0.9140625,0.921875,0.9296875,0.9375,0.9453125,
0.953125,0.9609375,0.96875,0.984375,0.9921875,1.),.UNSPECIFIED.);
#1178=B_SPLINE_CURVE_WITH_KNOTS('',3,(#43078,#43079,#43080,#43081,#43082,
#43083),.UNSPECIFIED.,.F.,.F.,(4,1,1,4),(0.,0.5,0.75,1.),.UNSPECIFIED.);
#1179=B_SPLINE_CURVE_WITH_KNOTS('',3,(#43085,#43086,#43087,#43088,#43089,
#43090,#43091,#43092,#43093,#43094,#43095,#43096,#43097,#43098,#43099,#43100,
#43101,#43102,#43103,#43104,#43105,#43106,#43107,#43108,#43109,#43110,#43111,
#43112,#43113,#43114,#43115,#43116),.UNSPECIFIED.,.F.,.F.,(4,1,1,1,1,1,
1,1,1,1,1,1,1,1,1,1,1,1,1,1,1,1,1,1,1,1,1,1,1,4),(0.,0.0624999888291916,
0.124999977658383,0.187499966487575,0.218749960902171,0.234374958109469,
0.249999955316766,0.265624952524064,0.273437451127713,0.281249949731362,
0.285156199033187,0.289062448335011,0.29687494693866,0.312499944145958,
0.343749938560554,0.37499993297515,0.406249927389746,0.437499921804341,
0.499999910633533,0.531249905048129,0.546874902255427,0.562499899462725,
0.570312398066374,0.578124896670023,0.59374989387732,0.624999888291916,
0.687499877121108,0.7499998659503,0.874999843608683,0.999999821267066),
 .UNSPECIFIED.);
#1180=B_SPLINE_CURVE_WITH_KNOTS('',3,(#43118,#43119,#43120,#43121,#43122,
#43123,#43124,#43125,#43126,#43127,#43128,#43129,#43130,#43131,#43132,#43133,
#43134,#43135,#43136,#43137,#43138,#43139,#43140,#43141,#43142,#43143,#43144,
#43145,#43146,#43147,#43148,#43149,#43150,#43151,#43152,#43153,#43154,#43155,
#43156,#43157,#43158,#43159,#43160,#43161,#43162,#43163,#43164,#43165,#43166,
#43167,#43168,#43169,#43170,#43171,#43172,#43173,#43174,#43175,#43176,#43177,
#43178,#43179,#43180,#43181,#43182,#43183,#43184,#43185,#43186,#43187,#43188,
#43189,#43190,#43191,#43192,#43193,#43194,#43195,#43196,#43197,#43198,#43199,
#43200,#43201,#43202,#43203,#43204,#43205,#43206,#43207,#43208,#43209,#43210,
#43211,#43212,#43213,#43214,#43215,#43216,#43217,#43218,#43219,#43220,#43221,
#43222,#43223,#43224,#43225,#43226,#43227,#43228,#43229,#43230,#43231,#43232,
#43233,#43234,#43235,#43236,#43237,#43238),.UNSPECIFIED.,.F.,.F.,(4,1,1,
1,1,1,1,1,1,1,1,1,1,1,1,1,1,1,1,1,1,1,1,1,1,1,1,1,1,1,1,1,1,1,1,1,1,1,1,
1,1,1,1,1,1,1,1,1,1,1,1,1,1,1,1,1,1,1,1,1,1,1,1,1,1,1,1,1,1,1,1,1,1,1,1,
1,1,1,1,1,1,1,1,1,1,1,1,1,1,1,1,1,1,1,1,1,1,1,1,1,1,1,1,1,1,1,1,1,1,1,1,
1,1,1,1,1,1,1,4),(0.,0.03125,0.0625,0.09375,0.109375,0.125,0.1328125,0.140625,
0.15625,0.171875,0.1796875,0.18359375,0.1875,0.19140625,0.1953125,0.203125,
0.21875,0.2265625,0.234375,0.2421875,0.24609375,0.248046875,0.25,0.251953125,
0.25390625,0.2578125,0.265625,0.2734375,0.28125,0.296875,0.3046875,0.30859375,
0.310546875,0.3125,0.314453125,0.31640625,0.3203125,0.328125,0.3359375,
0.34375,0.3515625,0.359375,0.3671875,0.37109375,0.373046875,0.375,0.376953125,
0.37890625,0.3828125,0.390625,0.40625,0.4140625,0.421875,0.4296875,0.43359375,
0.435546875,0.4375,0.439453125,0.44140625,0.4453125,0.453125,0.4609375,
0.46875,0.484375,0.4921875,0.49609375,0.5,0.50390625,0.5078125,0.515625,
0.53125,0.5625,0.578125,0.59375,0.6015625,0.609375,0.61328125,0.6171875,
0.62109375,0.623046875,0.625,0.626953125,0.62890625,0.6328125,0.640625,
0.6484375,0.65234375,0.654296875,0.65625,0.658203125,0.66015625,0.6640625,
0.671875,0.6796875,0.6875,0.6953125,0.703125,0.71875,0.7265625,0.734375,
0.7421875,0.74609375,0.75,0.75390625,0.7578125,0.765625,0.78125,0.796875,
0.8125,0.84375,0.859375,0.8671875,0.875,0.8828125,0.890625,0.90625,0.9375,
0.96875,1.),.UNSPECIFIED.);
#1181=B_SPLINE_CURVE_WITH_KNOTS('',3,(#43240,#43241,#43242,#43243,#43244,
#43245,#43246,#43247,#43248,#43249,#43250,#43251,#43252,#43253,#43254,#43255,
#43256,#43257,#43258,#43259,#43260,#43261,#43262,#43263,#43264,#43265,#43266,
#43267,#43268,#43269,#43270,#43271,#43272,#43273,#43274,#43275,#43276,#43277,
#43278,#43279,#43280,#43281,#43282,#43283,#43284,#43285,#43286,#43287,#43288,
#43289,#43290,#43291,#43292,#43293,#43294,#43295,#43296,#43297,#43298,#43299,
#43300,#43301,#43302,#43303,#43304,#43305,#43306,#43307,#43308,#43309,#43310,
#43311,#43312,#43313,#43314,#43315,#43316,#43317,#43318,#43319,#43320,#43321,
#43322,#43323,#43324,#43325,#43326,#43327,#43328,#43329,#43330,#43331,#43332,
#43333,#43334,#43335,#43336,#43337,#43338,#43339,#43340,#43341,#43342,#43343,
#43344,#43345,#43346,#43347,#43348,#43349,#43350,#43351,#43352,#43353,#43354,
#43355,#43356,#43357,#43358,#43359,#43360,#43361,#43362,#43363,#43364,#43365,
#43366,#43367,#43368,#43369,#43370,#43371,#43372,#43373,#43374,#43375,#43376,
#43377,#43378,#43379,#43380,#43381,#43382,#43383),.UNSPECIFIED.,.F.,.F.,
(4,1,1,1,1,1,1,1,1,1,1,1,1,1,1,1,1,1,1,1,1,1,1,1,1,1,1,1,1,1,1,1,1,1,1,
1,1,1,1,1,1,1,1,1,1,1,1,1,1,1,1,1,1,1,1,1,1,1,1,1,1,1,1,1,1,1,1,1,1,1,1,
1,1,1,1,1,1,1,1,1,1,1,1,1,1,1,1,1,1,1,1,1,1,1,1,1,1,1,1,1,1,1,1,1,1,1,1,
1,1,1,1,1,1,1,1,1,1,1,1,1,1,1,1,1,1,1,1,1,1,1,1,1,1,1,1,1,1,1,1,1,1,4),
(0.,0.03125,0.046875,0.0625,0.078125,0.09375,0.1015625,0.109375,0.1171875,
0.12109375,0.123046875,0.125,0.126953125,0.12890625,0.1328125,0.140625,
0.1484375,0.15234375,0.15625,0.1640625,0.171875,0.1796875,0.1875,0.19140625,
0.1953125,0.203125,0.21875,0.2265625,0.234375,0.2421875,0.24609375,0.248046875,
0.25,0.251953125,0.25390625,0.2578125,0.265625,0.2734375,0.28125,0.296875,
0.3046875,0.30859375,0.3125,0.31640625,0.3203125,0.328125,0.34375,0.359375,
0.3671875,0.37109375,0.375,0.37890625,0.3828125,0.390625,0.40625,0.421875,
0.4375,0.453125,0.46875,0.4765625,0.484375,0.4921875,0.49609375,0.498046875,
0.5,0.501953125,0.50390625,0.5078125,0.515625,0.5234375,0.53125,0.5390625,
0.546875,0.5546875,0.55859375,0.560546875,0.5625,0.564453125,0.56640625,
0.5703125,0.578125,0.5859375,0.59375,0.609375,0.625,0.65625,0.671875,0.6875,
0.703125,0.71875,0.7265625,0.734375,0.73828125,0.7421875,0.74609375,0.748046875,
0.75,0.751953125,0.75390625,0.7578125,0.765625,0.7734375,0.78125,0.7890625,
0.796875,0.80078125,0.8046875,0.80859375,0.810546875,0.8115234375,0.8125,
0.8134765625,0.814453125,0.81640625,0.8203125,0.82421875,0.828125,0.8359375,
0.84375,0.859375,0.8671875,0.87109375,0.875,0.87890625,0.8828125,0.890625,
0.8984375,0.90625,0.9140625,0.921875,0.9296875,0.93359375,0.935546875,0.9375,
0.939453125,0.94140625,0.9453125,0.953125,0.9609375,0.96875,0.984375,1.),
 .UNSPECIFIED.);
#1182=B_SPLINE_CURVE_WITH_KNOTS('',3,(#43385,#43386,#43387,#43388,#43389,
#43390,#43391,#43392,#43393,#43394,#43395,#43396,#43397,#43398,#43399,#43400,
#43401,#43402,#43403,#43404,#43405,#43406,#43407,#43408,#43409,#43410,#43411,
#43412,#43413,#43414,#43415,#43416,#43417,#43418,#43419,#43420,#43421,#43422,
#43423,#43424,#43425,#43426,#43427,#43428,#43429,#43430,#43431,#43432,#43433,
#43434,#43435,#43436,#43437,#43438,#43439,#43440,#43441,#43442,#43443,#43444,
#43445,#43446,#43447,#43448,#43449,#43450,#43451,#43452,#43453,#43454,#43455,
#43456,#43457,#43458,#43459,#43460,#43461,#43462,#43463,#43464,#43465,#43466,
#43467,#43468,#43469,#43470,#43471,#43472,#43473,#43474,#43475,#43476,#43477,
#43478,#43479,#43480,#43481,#43482,#43483,#43484,#43485,#43486,#43487,#43488,
#43489,#43490,#43491,#43492,#43493,#43494,#43495,#43496,#43497,#43498,#43499,
#43500,#43501,#43502,#43503,#43504,#43505,#43506,#43507,#43508,#43509,#43510,
#43511,#43512,#43513,#43514,#43515,#43516,#43517,#43518),.UNSPECIFIED.,
 .F.,.F.,(4,1,1,1,1,1,1,1,1,1,1,1,1,1,1,1,1,1,1,1,1,1,1,1,1,1,1,1,1,1,1,
1,1,1,1,1,1,1,1,1,1,1,1,1,1,1,1,1,1,1,1,1,1,1,1,1,1,1,1,1,1,1,1,1,1,1,1,
1,1,1,1,1,1,1,1,1,1,1,1,1,1,1,1,1,1,1,1,1,1,1,1,1,1,1,1,1,1,1,1,1,1,1,1,
1,1,1,1,1,1,1,1,1,1,1,1,1,1,1,1,1,1,1,1,1,1,1,1,1,1,1,1,4),(0.,0.015625,
0.03125,0.046875,0.0546875,0.05859375,0.0625,0.06640625,0.0703125,0.078125,
0.09375,0.125,0.15625,0.171875,0.1875,0.203125,0.21875,0.2265625,0.234375,
0.2421875,0.24609375,0.248046875,0.25,0.251953125,0.25390625,0.2578125,
0.265625,0.2734375,0.27734375,0.28125,0.2890625,0.296875,0.3046875,0.30859375,
0.3125,0.31640625,0.3203125,0.328125,0.34375,0.359375,0.3671875,0.375,0.3828125,
0.390625,0.40625,0.421875,0.4296875,0.43359375,0.4375,0.44140625,0.4453125,
0.453125,0.46875,0.484375,0.4921875,0.49609375,0.5,0.50390625,0.5078125,
0.515625,0.53125,0.546875,0.5625,0.578125,0.59375,0.6015625,0.609375,0.6171875,
0.62109375,0.623046875,0.625,0.626953125,0.62890625,0.6328125,0.640625,
0.65625,0.6640625,0.671875,0.6796875,0.68359375,0.685546875,0.6875,0.689453125,
0.69140625,0.6953125,0.703125,0.71875,0.734375,0.7421875,0.74609375,0.75,
0.75390625,0.7578125,0.765625,0.78125,0.796875,0.8125,0.828125,0.84375,
0.8515625,0.859375,0.86328125,0.8671875,0.87109375,0.873046875,0.8740234375,
0.875,0.876953125,0.87890625,0.8828125,0.88671875,0.890625,0.8984375,0.90625,
0.9140625,0.921875,0.92578125,0.9296875,0.93359375,0.935546875,0.9365234375,
0.9375,0.9384765625,0.939453125,0.94140625,0.9453125,0.94921875,0.953125,
0.9609375,0.96875,0.984375,1.),.UNSPECIFIED.);
#1183=B_SPLINE_CURVE_WITH_KNOTS('',3,(#43520,#43521,#43522,#43523,#43524,
#43525,#43526,#43527,#43528,#43529,#43530),.UNSPECIFIED.,.F.,.F.,(4,1,1,
1,1,1,1,1,4),(0.,0.125,0.25,0.375,0.5,0.625,0.75,0.875,1.),
 .UNSPECIFIED.);
#1184=B_SPLINE_CURVE_WITH_KNOTS('',3,(#43532,#43533,#43534,#43535,#43536,
#43537,#43538,#43539,#43540,#43541,#43542),.UNSPECIFIED.,.F.,.F.,(4,1,1,
1,1,1,1,1,4),(0.,0.125,0.25,0.375,0.5,0.625,0.75,0.875,1.),
 .UNSPECIFIED.);
#1185=B_SPLINE_CURVE_WITH_KNOTS('',3,(#43544,#43545,#43546,#43547),
 .UNSPECIFIED.,.F.,.F.,(4,4),(0.,0.999935365761805),.UNSPECIFIED.);
#1186=B_SPLINE_CURVE_WITH_KNOTS('',3,(#43549,#43550,#43551,#43552),
 .UNSPECIFIED.,.F.,.F.,(4,4),(2.06275312002674E-5,0.999974447229001),
 .UNSPECIFIED.);
#1187=B_SPLINE_CURVE_WITH_KNOTS('',3,(#43553,#43554,#43555,#43556),
 .UNSPECIFIED.,.F.,.F.,(4,4),(8.00007213080448E-5,1.),.UNSPECIFIED.);
#1188=B_SPLINE_CURVE_WITH_KNOTS('',3,(#43558,#43559,#43560,#43561),
 .UNSPECIFIED.,.F.,.F.,(4,4),(2.02588963018075E-5,0.999973166574012),
 .UNSPECIFIED.);
#1189=B_SPLINE_CURVE_WITH_KNOTS('',3,(#43563,#43564,#43565,#43566),
 .UNSPECIFIED.,.F.,.F.,(4,4),(8.39549495919811E-5,1.),.UNSPECIFIED.);
#1190=B_SPLINE_CURVE_WITH_KNOTS('',3,(#43567,#43568,#43569,#43570),
 .UNSPECIFIED.,.F.,.F.,(4,4),(0.,0.99993649865183),.UNSPECIFIED.);
#1191=B_SPLINE_CURVE_WITH_KNOTS('',3,(#44099,#44100,#44101,#44102,#44103,
#44104,#44105,#44106,#44107,#44108,#44109,#44110,#44111,#44112,#44113,#44114,
#44115,#44116,#44117,#44118,#44119,#44120,#44121,#44122,#44123,#44124,#44125,
#44126,#44127,#44128,#44129,#44130,#44131,#44132,#44133,#44134,#44135,#44136,
#44137,#44138,#44139,#44140,#44141,#44142,#44143,#44144,#44145,#44146,#44147,
#44148,#44149,#44150,#44151,#44152,#44153,#44154,#44155,#44156,#44157,#44158,
#44159,#44160,#44161,#44162,#44163,#44164,#44165,#44166,#44167,#44168,#44169,
#44170,#44171,#44172,#44173,#44174,#44175,#44176,#44177,#44178,#44179,#44180,
#44181,#44182,#44183,#44184,#44185,#44186,#44187,#44188,#44189,#44190,#44191,
#44192,#44193,#44194,#44195,#44196,#44197,#44198,#44199,#44200,#44201,#44202,
#44203,#44204,#44205,#44206,#44207,#44208,#44209,#44210,#44211,#44212,#44213,
#44214,#44215,#44216),.UNSPECIFIED.,.F.,.F.,(4,1,1,1,1,1,1,1,1,1,1,1,1,
1,1,1,1,1,1,1,1,1,1,1,1,1,1,1,1,1,1,1,1,1,1,1,1,1,1,1,1,1,1,1,1,1,1,1,1,
1,1,1,1,1,1,1,1,1,1,1,1,1,1,1,1,1,1,1,1,1,1,1,1,1,1,1,1,1,1,1,1,1,1,1,1,
1,1,1,1,1,1,1,1,1,1,1,1,1,1,1,1,1,1,1,1,1,1,1,1,1,1,1,1,1,1,4),(0.,0.015625,
0.0234375,0.03125,0.0390625,0.046875,0.0546875,0.0625,0.078125,0.0859375,
0.09375,0.1015625,0.109375,0.1171875,0.125,0.140625,0.1484375,0.15625,0.1640625,
0.171875,0.1796875,0.1875,0.203125,0.2109375,0.21875,0.2265625,0.234375,
0.2421875,0.25,0.2578125,0.265625,0.2734375,0.28125,0.2890625,0.296875,
0.3125,0.3203125,0.328125,0.3359375,0.34375,0.3515625,0.359375,0.375,0.3828125,
0.390625,0.3984375,0.40625,0.4140625,0.421875,0.4375,0.4453125,0.453125,
0.4609375,0.46875,0.4765625,0.484375,0.4921875,0.5,0.515625,0.5234375,0.53125,
0.5390625,0.546875,0.5546875,0.5625,0.578125,0.5859375,0.59375,0.6015625,
0.609375,0.6171875,0.625,0.6328125,0.640625,0.6484375,0.65625,0.6640625,
0.671875,0.6875,0.6953125,0.703125,0.7109375,0.71875,0.7265625,0.734375,
0.75,0.7578125,0.765625,0.7734375,0.78125,0.7890625,0.796875,0.8125,0.8203125,
0.828125,0.8359375,0.84375,0.8515625,0.859375,0.8671875,0.875,0.8828125,
0.890625,0.8984375,0.90625,0.9140625,0.921875,0.9296875,0.9375,0.9453125,
0.953125,0.9609375,0.96875,0.984375,0.9921875,1.),.UNSPECIFIED.);
#1192=B_SPLINE_CURVE_WITH_KNOTS('',3,(#44217,#44218,#44219,#44220,#44221,
#44222),.UNSPECIFIED.,.F.,.F.,(4,1,1,4),(0.,0.5,0.75,1.),.UNSPECIFIED.);
#1193=B_SPLINE_CURVE_WITH_KNOTS('',3,(#44223,#44224,#44225,#44226,#44227,
#44228,#44229,#44230,#44231,#44232,#44233,#44234,#44235,#44236,#44237,#44238,
#44239,#44240,#44241,#44242,#44243,#44244,#44245,#44246,#44247,#44248,#44249,
#44250,#44251,#44252,#44253,#44254,#44255,#44256,#44257,#44258,#44259,#44260,
#44261,#44262,#44263,#44264,#44265,#44266,#44267,#44268,#44269,#44270,#44271,
#44272,#44273,#44274,#44275,#44276,#44277,#44278,#44279,#44280,#44281,#44282,
#44283,#44284,#44285,#44286,#44287,#44288,#44289,#44290,#44291,#44292,#44293,
#44294,#44295,#44296,#44297,#44298,#44299,#44300),.UNSPECIFIED.,.F.,.F.,
(4,1,1,1,1,1,1,1,1,1,1,1,1,1,1,1,1,1,1,1,1,1,1,1,1,1,1,1,1,1,1,1,1,1,1,
1,1,1,1,1,1,1,1,1,1,1,1,1,1,1,1,1,1,1,1,1,1,1,1,1,1,1,1,1,1,1,1,1,1,1,1,
1,1,1,1,4),(0.,0.0312499974019096,0.0624999948038192,0.0937499922057288,
0.109374990906684,0.117187490257161,0.124999989607638,0.132812488958116,
0.140624988308593,0.156249987009548,0.187499984411458,0.203124983112412,
0.218749981813367,0.234374980514322,0.242187479864799,0.246093729540038,
0.249999979215277,0.253906228890515,0.257812478565754,0.265624977916232,
0.281249976617186,0.296874975318141,0.304687474668619,0.312499974019096,
0.328124972720051,0.343749971421006,0.351562470771483,0.35937497012196,
0.367187469472438,0.371093719147676,0.374999968822915,0.378906218498154,
0.382812468173393,0.39062496752387,0.406249966224825,0.42187496492578,0.429687464276257,
0.437499963626734,0.445312462977212,0.453124962327689,0.468749961028644,
0.499999958430554,0.515624957131508,0.531249955832463,0.562499953234373,
0.593749950636282,0.609374949337237,0.617187448687714,0.624999948038192,
0.632812447388669,0.640624946739147,0.656249945440102,0.687499942842011,
0.718749940243921,0.74999993764583,0.765624936346785,0.78124993504774,0.796874933748695,
0.804687433099172,0.812499932449649,0.820312431800127,0.828124931150604,
0.843749929851559,0.859374928552514,0.867187427902991,0.87109367757823,
0.874999927253469,0.878906176928707,0.882812426603946,0.890624925954423,
0.906249924655378,0.921874923356333,0.937499922057288,0.953124920758243,
0.968749919459197,0.999999916861107),.UNSPECIFIED.);
#1194=B_SPLINE_CURVE_WITH_KNOTS('',3,(#44302,#44303,#44304,#44305,#44306,
#44307,#44308,#44309,#44310,#44311,#44312,#44313,#44314,#44315,#44316,#44317,
#44318,#44319,#44320,#44321,#44322,#44323,#44324,#44325,#44326,#44327,#44328,
#44329,#44330,#44331,#44332,#44333,#44334,#44335,#44336,#44337,#44338,#44339,
#44340,#44341,#44342,#44343,#44344,#44345,#44346,#44347,#44348,#44349,#44350,
#44351,#44352,#44353,#44354,#44355,#44356,#44357,#44358,#44359,#44360,#44361,
#44362,#44363,#44364,#44365,#44366,#44367,#44368,#44369,#44370,#44371,#44372,
#44373,#44374,#44375,#44376,#44377,#44378,#44379,#44380,#44381,#44382,#44383,
#44384,#44385,#44386,#44387,#44388,#44389,#44390,#44391,#44392,#44393,#44394,
#44395,#44396,#44397,#44398,#44399,#44400,#44401,#44402,#44403,#44404,#44405,
#44406,#44407,#44408,#44409,#44410,#44411,#44412,#44413,#44414,#44415,#44416,
#44417,#44418,#44419,#44420,#44421,#44422,#44423,#44424,#44425,#44426,#44427,
#44428,#44429,#44430,#44431,#44432,#44433,#44434,#44435,#44436,#44437,#44438,
#44439,#44440,#44441,#44442,#44443,#44444,#44445,#44446,#44447,#44448,#44449,
#44450,#44451,#44452,#44453,#44454),.UNSPECIFIED.,.F.,.F.,(4,1,1,1,1,1,
1,1,1,1,1,1,1,1,1,1,1,1,1,1,1,1,1,1,1,1,1,1,1,1,1,1,1,1,1,1,1,1,1,1,1,1,
1,1,1,1,1,1,1,1,1,1,1,1,1,1,1,1,1,1,1,1,1,1,1,1,1,1,1,1,1,1,1,1,1,1,1,1,
1,1,1,1,1,1,1,1,1,1,1,1,1,1,1,1,1,1,1,1,1,1,1,1,1,1,1,1,1,1,1,1,1,1,1,1,
1,1,1,1,1,1,1,1,1,1,1,1,1,1,1,1,1,1,1,1,1,1,1,1,1,1,1,1,1,1,1,1,1,1,1,1,
4),(0.,0.015625,0.03125,0.0390625,0.046875,0.0546875,0.05859375,0.060546875,
0.0625,0.064453125,0.06640625,0.0703125,0.078125,0.0859375,0.09375,0.109375,
0.125,0.140625,0.15625,0.171875,0.1875,0.203125,0.21875,0.2265625,0.234375,
0.23828125,0.2421875,0.24609375,0.248046875,0.25,0.251953125,0.25390625,
0.2578125,0.265625,0.2734375,0.28125,0.2890625,0.296875,0.30078125,0.3046875,
0.30859375,0.310546875,0.3115234375,0.3125,0.3134765625,0.314453125,0.31640625,
0.3203125,0.32421875,0.328125,0.3359375,0.34375,0.359375,0.3671875,0.37109375,
0.375,0.37890625,0.3828125,0.390625,0.3984375,0.40625,0.4140625,0.421875,
0.4296875,0.43359375,0.435546875,0.4375,0.439453125,0.44140625,0.4453125,
0.453125,0.4609375,0.46875,0.4765625,0.484375,0.4921875,0.49609375,0.498046875,
0.5,0.501953125,0.50390625,0.5078125,0.515625,0.5234375,0.53125,0.546875,
0.5625,0.59375,0.609375,0.625,0.6328125,0.640625,0.65625,0.671875,0.6796875,
0.68359375,0.6875,0.69140625,0.6953125,0.703125,0.71875,0.7265625,0.734375,
0.7421875,0.74609375,0.748046875,0.75,0.751953125,0.75390625,0.7578125,
0.765625,0.7734375,0.78125,0.7890625,0.796875,0.8046875,0.80859375,0.810546875,
0.8125,0.814453125,0.81640625,0.8203125,0.828125,0.8359375,0.84375,0.8515625,
0.859375,0.8671875,0.87109375,0.873046875,0.875,0.876953125,0.87890625,
0.8828125,0.890625,0.8984375,0.90625,0.9140625,0.921875,0.9296875,0.93359375,
0.935546875,0.9375,0.939453125,0.94140625,0.9453125,0.953125,0.9609375,
0.96875,0.984375,1.),.UNSPECIFIED.);
#1195=B_SPLINE_CURVE_WITH_KNOTS('',3,(#44456,#44457,#44458,#44459,#44460,
#44461,#44462,#44463,#44464,#44465,#44466),.UNSPECIFIED.,.F.,.F.,(4,1,1,
1,1,1,1,1,4),(0.,0.125,0.25,0.375,0.5,0.625,0.75,0.875,1.),
 .UNSPECIFIED.);
#1196=B_SPLINE_CURVE_WITH_KNOTS('',3,(#44468,#44469,#44470,#44471,#44472,
#44473,#44474,#44475,#44476,#44477,#44478,#44479,#44480,#44481,#44482,#44483,
#44484,#44485,#44486,#44487,#44488,#44489,#44490,#44491,#44492,#44493,#44494,
#44495,#44496,#44497,#44498,#44499,#44500,#44501,#44502,#44503,#44504,#44505,
#44506,#44507,#44508,#44509,#44510,#44511,#44512,#44513,#44514,#44515,#44516,
#44517,#44518,#44519,#44520,#44521,#44522,#44523,#44524,#44525,#44526,#44527,
#44528,#44529,#44530,#44531,#44532,#44533,#44534,#44535,#44536,#44537,#44538,
#44539,#44540,#44541,#44542,#44543,#44544,#44545,#44546,#44547,#44548,#44549,
#44550,#44551,#44552,#44553,#44554,#44555,#44556,#44557,#44558,#44559,#44560,
#44561,#44562,#44563,#44564,#44565,#44566,#44567,#44568,#44569,#44570,#44571,
#44572,#44573,#44574,#44575,#44576,#44577,#44578,#44579,#44580,#44581,#44582,
#44583,#44584,#44585,#44586,#44587,#44588,#44589,#44590,#44591,#44592),
 .UNSPECIFIED.,.F.,.F.,(4,1,1,1,1,1,1,1,1,1,1,1,1,1,1,1,1,1,1,1,1,1,1,1,
1,1,1,1,1,1,1,1,1,1,1,1,1,1,1,1,1,1,1,1,1,1,1,1,1,1,1,1,1,1,1,1,1,1,1,1,
1,1,1,1,1,1,1,1,1,1,1,1,1,1,1,1,1,1,1,1,1,1,1,1,1,1,1,1,1,1,1,1,1,1,1,1,
1,1,1,1,1,1,1,1,1,1,1,1,1,1,1,1,1,1,1,1,1,1,1,1,1,1,4),(0.,0.03125,0.046875,
0.0625,0.078125,0.09375,0.1015625,0.109375,0.11328125,0.1171875,0.12109375,
0.123046875,0.125,0.126953125,0.12890625,0.1328125,0.140625,0.1484375,0.15234375,
0.154296875,0.15625,0.158203125,0.16015625,0.1640625,0.171875,0.1796875,
0.1875,0.1953125,0.203125,0.21875,0.234375,0.2421875,0.24609375,0.248046875,
0.25,0.251953125,0.25390625,0.2578125,0.265625,0.28125,0.296875,0.3125,
0.328125,0.34375,0.359375,0.3671875,0.375,0.3828125,0.390625,0.40625,0.421875,
0.4375,0.453125,0.46875,0.4765625,0.484375,0.4921875,0.49609375,0.498046875,
0.5,0.501953125,0.50390625,0.5078125,0.515625,0.53125,0.5390625,0.546875,
0.5546875,0.55859375,0.560546875,0.5625,0.564453125,0.56640625,0.5703125,
0.578125,0.5859375,0.59375,0.609375,0.625,0.640625,0.65625,0.671875,0.6875,
0.703125,0.71875,0.7265625,0.734375,0.7421875,0.74609375,0.748046875,0.75,
0.751953125,0.75390625,0.7578125,0.765625,0.7734375,0.77734375,0.78125,
0.7890625,0.796875,0.8046875,0.80859375,0.8125,0.81640625,0.8203125,0.828125,
0.84375,0.859375,0.8671875,0.875,0.8828125,0.890625,0.90625,0.921875,0.9296875,
0.93359375,0.9375,0.94140625,0.9453125,0.953125,0.96875,0.984375,1.),
 .UNSPECIFIED.);
#1197=B_SPLINE_CURVE_WITH_KNOTS('',3,(#44594,#44595,#44596,#44597,#44598,
#44599,#44600,#44601,#44602,#44603,#44604,#44605,#44606,#44607,#44608,#44609,
#44610,#44611,#44612,#44613,#44614,#44615,#44616,#44617,#44618,#44619,#44620,
#44621,#44622,#44623,#44624,#44625,#44626,#44627,#44628,#44629,#44630,#44631,
#44632,#44633,#44634,#44635,#44636,#44637,#44638,#44639,#44640,#44641,#44642,
#44643,#44644,#44645,#44646,#44647,#44648,#44649,#44650,#44651,#44652,#44653,
#44654,#44655,#44656,#44657,#44658,#44659,#44660,#44661,#44662,#44663,#44664,
#44665,#44666,#44667,#44668,#44669,#44670,#44671,#44672,#44673,#44674,#44675,
#44676,#44677,#44678,#44679,#44680,#44681,#44682,#44683,#44684,#44685,#44686,
#44687,#44688,#44689,#44690,#44691,#44692,#44693,#44694,#44695,#44696,#44697,
#44698,#44699,#44700,#44701,#44702,#44703,#44704,#44705,#44706,#44707,#44708,
#44709,#44710,#44711,#44712,#44713,#44714,#44715,#44716,#44717,#44718,#44719,
#44720,#44721,#44722,#44723,#44724,#44725,#44726,#44727,#44728,#44729,#44730,
#44731,#44732,#44733,#44734,#44735,#44736,#44737,#44738,#44739,#44740,#44741,
#44742,#44743,#44744,#44745,#44746,#44747),.UNSPECIFIED.,.F.,.F.,(4,1,1,
1,1,1,1,1,1,1,1,1,1,1,1,1,1,1,1,1,1,1,1,1,1,1,1,1,1,1,1,1,1,1,1,1,1,1,1,
1,1,1,1,1,1,1,1,1,1,1,1,1,1,1,1,1,1,1,1,1,1,1,1,1,1,1,1,1,1,1,1,1,1,1,1,
1,1,1,1,1,1,1,1,1,1,1,1,1,1,1,1,1,1,1,1,1,1,1,1,1,1,1,1,1,1,1,1,1,1,1,1,
1,1,1,1,1,1,1,1,1,1,1,1,1,1,1,1,1,1,1,1,1,1,1,1,1,1,1,1,1,1,1,1,1,1,1,1,
1,1,1,1,4),(0.,0.015625,0.03125,0.0390625,0.046875,0.0546875,0.05859375,
0.060546875,0.0625,0.064453125,0.06640625,0.0703125,0.078125,0.09375,0.109375,
0.125,0.140625,0.15625,0.171875,0.1875,0.203125,0.21875,0.2265625,0.234375,
0.23828125,0.2421875,0.24609375,0.248046875,0.25,0.251953125,0.25390625,
0.2578125,0.265625,0.2734375,0.28125,0.2890625,0.296875,0.30078125,0.3046875,
0.30859375,0.310546875,0.3115234375,0.3125,0.3134765625,0.314453125,0.31640625,
0.3203125,0.32421875,0.328125,0.3359375,0.34375,0.359375,0.3671875,0.37109375,
0.375,0.37890625,0.3828125,0.390625,0.40625,0.4140625,0.421875,0.4296875,
0.43359375,0.435546875,0.4375,0.439453125,0.44140625,0.4453125,0.453125,
0.4609375,0.46875,0.4765625,0.484375,0.4921875,0.49609375,0.498046875,0.5,
0.501953125,0.50390625,0.5078125,0.515625,0.5234375,0.53125,0.546875,0.5625,
0.59375,0.609375,0.6171875,0.625,0.6328125,0.640625,0.65625,0.671875,0.6796875,
0.68359375,0.6875,0.69140625,0.6953125,0.703125,0.71875,0.7265625,0.734375,
0.7421875,0.74609375,0.748046875,0.75,0.751953125,0.75390625,0.7578125,
0.76171875,0.765625,0.7734375,0.78125,0.7890625,0.796875,0.8046875,0.80859375,
0.810546875,0.8125,0.814453125,0.81640625,0.8203125,0.82421875,0.828125,
0.8359375,0.84375,0.8515625,0.859375,0.8671875,0.87109375,0.873046875,0.875,
0.876953125,0.87890625,0.8828125,0.890625,0.90625,0.9140625,0.921875,0.92578125,
0.9296875,0.93359375,0.935546875,0.9375,0.939453125,0.94140625,0.9453125,
0.953125,0.9609375,0.96875,0.984375,1.),.UNSPECIFIED.);
#1198=B_SPLINE_CURVE_WITH_KNOTS('',3,(#44749,#44750,#44751,#44752,#44753,
#44754,#44755,#44756,#44757,#44758,#44759),.UNSPECIFIED.,.F.,.F.,(4,1,1,
1,1,1,1,1,4),(0.,0.125,0.25,0.375,0.5,0.625,0.75,0.875,1.),
 .UNSPECIFIED.);
#1199=B_SPLINE_CURVE_WITH_KNOTS('',3,(#44761,#44762,#44763,#44764,#44765,
#44766,#44767,#44768,#44769,#44770,#44771,#44772,#44773,#44774,#44775,#44776,
#44777,#44778,#44779,#44780,#44781,#44782,#44783,#44784,#44785,#44786,#44787,
#44788,#44789,#44790,#44791,#44792,#44793,#44794,#44795,#44796),
 .UNSPECIFIED.,.F.,.F.,(4,1,1,1,1,1,1,1,1,1,1,1,1,1,1,1,1,1,1,1,1,1,1,1,
1,1,1,1,1,1,1,1,1,4),(3.38284667726637E-8,0.0625000317141876,0.125000029599908,
0.187500027485629,0.21875002642849,0.25000002537135,0.26562502484278,0.273437524578495,
0.281250024314211,0.285156274182068,0.289062524049926,0.296875023785641,
0.312500023257071,0.343750022199931,0.375000021142792,0.437500019028513,
0.468750017971373,0.500000016914233,0.531250015857094,0.546875015328524,
0.562500014799954,0.566406264667812,0.570312514535669,0.578125014271384,
0.585937514007099,0.593750013742815,0.625000012685675,0.687500010571396,
0.750000008457117,0.781250007399977,0.812500006342838,0.875000004228558,
0.937500002114279,1.),.UNSPECIFIED.);
#1200=B_SPLINE_CURVE_WITH_KNOTS('',3,(#44797,#44798,#44799,#44800,#44801,
#44802),.UNSPECIFIED.,.F.,.F.,(4,1,1,4),(0.,0.25,0.5,1.),.UNSPECIFIED.);
#1201=PLANE('',#13804);
#1202=PLANE('',#13805);
#1203=PLANE('',#13806);
#1204=PLANE('',#13811);
#1205=PLANE('',#13814);
#1206=PLANE('',#13817);
#1207=PLANE('',#13818);
#1208=PLANE('',#13822);
#1209=PLANE('',#13823);
#1210=PLANE('',#13827);
#1211=PLANE('',#13828);
#1212=PLANE('',#13832);
#1213=PLANE('',#13835);
#1214=PLANE('',#13838);
#1215=PLANE('',#13841);
#1216=PLANE('',#13844);
#1217=PLANE('',#13858);
#1218=PLANE('',#13872);
#1219=PLANE('',#13875);
#1220=PLANE('',#13904);
#1221=PLANE('',#13907);
#1222=PLANE('',#13912);
#1223=PLANE('',#13914);
#1224=PLANE('',#13915);
#1225=PLANE('',#13918);
#1226=PLANE('',#13921);
#1227=PLANE('',#13924);
#1228=PLANE('',#13927);
#1229=PLANE('',#13930);
#1230=PLANE('',#13933);
#1231=PLANE('',#13936);
#1232=PLANE('',#13939);
#1233=PLANE('',#13986);
#1234=PLANE('',#13987);
#1235=PLANE('',#13988);
#1236=PLANE('',#13989);
#1237=PLANE('',#13997);
#1238=PLANE('',#13998);
#1239=PLANE('',#14000);
#1240=PLANE('',#14004);
#1241=PLANE('',#14006);
#1242=PLANE('',#14172);
#1243=PLANE('',#14175);
#1244=PLANE('',#14178);
#1245=PLANE('',#14182);
#1246=PLANE('',#14183);
#1247=PLANE('',#14184);
#1248=PLANE('',#14187);
#1249=PLANE('',#14194);
#1250=PLANE('',#14198);
#1251=PLANE('',#14200);
#1252=PLANE('',#14201);
#1253=PLANE('',#14203);
#1254=PLANE('',#14205);
#1255=PLANE('',#14206);
#1256=PLANE('',#14226);
#1257=PLANE('',#14228);
#1258=PLANE('',#14230);
#1259=PLANE('',#14232);
#1260=PLANE('',#14234);
#1261=PLANE('',#14236);
#1262=PLANE('',#14238);
#1263=PLANE('',#14240);
#1264=PLANE('',#14242);
#1265=PLANE('',#14243);
#1266=PLANE('',#14246);
#1267=PLANE('',#14248);
#1268=PLANE('',#14250);
#1269=PLANE('',#14252);
#1270=PLANE('',#14254);
#1271=PLANE('',#14262);
#1272=PLANE('',#14265);
#1273=PLANE('',#14277);
#1274=PLANE('',#14280);
#1275=PLANE('',#14283);
#1276=PLANE('',#14286);
#1277=PLANE('',#14289);
#1278=PLANE('',#14305);
#1279=PLANE('',#14311);
#1280=PLANE('',#14312);
#1281=PLANE('',#14317);
#1282=PLANE('',#14320);
#1283=PLANE('',#14322);
#1284=PLANE('',#14325);
#1285=PLANE('',#14327);
#1286=PLANE('',#14335);
#1287=PLANE('',#14338);
#1288=PLANE('',#14341);
#1289=PLANE('',#14344);
#1290=PLANE('',#14384);
#1291=PLANE('',#14385);
#1292=PLANE('',#14386);
#1293=PLANE('',#14389);
#1294=PLANE('',#14438);
#1295=PLANE('',#14488);
#1296=PLANE('',#14489);
#1297=PLANE('',#14491);
#1298=PLANE('',#14492);
#1299=PLANE('',#14494);
#1300=PLANE('',#14495);
#1301=PLANE('',#14497);
#1302=PLANE('',#14498);
#1303=PLANE('',#14500);
#1304=PLANE('',#14501);
#1305=PLANE('',#14503);
#1306=PLANE('',#14504);
#1307=PLANE('',#14506);
#1308=PLANE('',#14507);
#1309=PLANE('',#14509);
#1310=PLANE('',#14510);
#1311=PLANE('',#14512);
#1312=PLANE('',#14513);
#1313=PLANE('',#14515);
#1314=PLANE('',#14516);
#1315=PLANE('',#14518);
#1316=PLANE('',#14519);
#1317=PLANE('',#14521);
#1318=PLANE('',#14522);
#1319=PLANE('',#14524);
#1320=PLANE('',#14525);
#1321=PLANE('',#14527);
#1322=PLANE('',#14528);
#1323=PLANE('',#14530);
#1324=PLANE('',#14531);
#1325=PLANE('',#14533);
#1326=PLANE('',#14534);
#1327=PLANE('',#14536);
#1328=PLANE('',#14537);
#1329=PLANE('',#14539);
#1330=PLANE('',#14540);
#1331=PLANE('',#14542);
#1332=PLANE('',#14543);
#1333=PLANE('',#14545);
#1334=PLANE('',#14546);
#1335=PLANE('',#14548);
#1336=PLANE('',#14549);
#1337=PLANE('',#14551);
#1338=PLANE('',#14552);
#1339=PLANE('',#14554);
#1340=PLANE('',#14555);
#1341=PLANE('',#14557);
#1342=PLANE('',#14558);
#1343=PLANE('',#14560);
#1344=PLANE('',#14561);
#1345=PLANE('',#14563);
#1346=PLANE('',#14564);
#1347=PLANE('',#14566);
#1348=PLANE('',#14567);
#1349=PLANE('',#14569);
#1350=PLANE('',#14570);
#1351=PLANE('',#14572);
#1352=PLANE('',#14573);
#1353=PLANE('',#14575);
#1354=PLANE('',#14576);
#1355=PLANE('',#14578);
#1356=PLANE('',#14579);
#1357=PLANE('',#14581);
#1358=PLANE('',#14582);
#1359=PLANE('',#14584);
#1360=PLANE('',#14585);
#1361=PLANE('',#14587);
#1362=PLANE('',#14588);
#1363=PLANE('',#14590);
#1364=PLANE('',#14591);
#1365=PLANE('',#14593);
#1366=PLANE('',#14594);
#1367=PLANE('',#14596);
#1368=PLANE('',#14597);
#1369=PLANE('',#14599);
#1370=PLANE('',#14600);
#1371=PLANE('',#14602);
#1372=PLANE('',#14603);
#1373=PLANE('',#14605);
#1374=PLANE('',#14606);
#1375=PLANE('',#14608);
#1376=PLANE('',#14609);
#1377=PLANE('',#14611);
#1378=PLANE('',#14612);
#1379=PLANE('',#14614);
#1380=PLANE('',#14615);
#1381=PLANE('',#14616);
#1382=PLANE('',#14617);
#1383=PLANE('',#14619);
#1384=PLANE('',#14620);
#1385=PLANE('',#14622);
#1386=PLANE('',#14623);
#1387=PLANE('',#14625);
#1388=PLANE('',#14626);
#1389=PLANE('',#14628);
#1390=PLANE('',#14629);
#1391=PLANE('',#14630);
#1392=PLANE('',#14642);
#1393=PLANE('',#14645);
#1394=PLANE('',#14651);
#1395=PLANE('',#14654);
#1396=PLANE('',#14661);
#1397=PLANE('',#14670);
#1398=PLANE('',#14679);
#1399=PLANE('',#14681);
#1400=PLANE('',#14683);
#1401=PLANE('',#14699);
#1402=PLANE('',#14703);
#1403=PLANE('',#14704);
#1404=PLANE('',#14705);
#1405=PLANE('',#14709);
#1406=PLANE('',#14710);
#1407=PLANE('',#14714);
#1408=PLANE('',#14717);
#1409=PLANE('',#14720);
#1410=PLANE('',#14723);
#1411=PLANE('',#14732);
#1412=PLANE('',#14765);
#1413=PLANE('',#14768);
#1414=PLANE('',#14769);
#1415=PLANE('',#14772);
#1416=PLANE('',#14775);
#1417=PLANE('',#14776);
#1418=PLANE('',#14779);
#1419=PLANE('',#14782);
#1420=PLANE('',#14783);
#1421=PLANE('',#14786);
#1422=PLANE('',#14792);
#1423=PLANE('',#14801);
#1424=PLANE('',#14802);
#1425=PLANE('',#14803);
#1426=PLANE('',#14804);
#1427=PLANE('',#14805);
#1428=PLANE('',#14814);
#1429=PLANE('',#14823);
#1430=PLANE('',#14828);
#1431=PLANE('',#14830);
#1432=PLANE('',#14837);
#1433=PLANE('',#14848);
#1434=PLANE('',#14854);
#1435=PLANE('',#14862);
#1436=PLANE('',#14867);
#1437=PLANE('',#14876);
#1438=PLANE('',#14883);
#1439=PLANE('',#14890);
#1440=PLANE('',#14897);
#1441=PLANE('',#14906);
#1442=PLANE('',#14913);
#1443=PLANE('',#14915);
#1444=PLANE('',#14917);
#1445=PLANE('',#14919);
#1446=PLANE('',#14921);
#1447=PLANE('',#14922);
#1448=PLANE('',#14924);
#1449=PLANE('',#14926);
#1450=PLANE('',#14927);
#1451=PLANE('',#14929);
#1452=PLANE('',#14931);
#1453=PLANE('',#14932);
#1454=PLANE('',#14933);
#1455=PLANE('',#14936);
#1456=PLANE('',#14937);
#1457=PLANE('',#14938);
#1458=PLANE('',#14945);
#1459=PLANE('',#14947);
#1460=PLANE('',#14949);
#1461=PLANE('',#14951);
#1462=PLANE('',#14954);
#1463=PLANE('',#14958);
#1464=PLANE('',#15001);
#1465=PLANE('',#15004);
#1466=PLANE('',#15005);
#1467=PLANE('',#15008);
#1468=PLANE('',#15011);
#1469=PLANE('',#15012);
#1470=PLANE('',#15015);
#1471=PLANE('',#15018);
#1472=PLANE('',#15019);
#1473=PLANE('',#15022);
#1474=PLANE('',#15032);
#1475=PLANE('',#15049);
#1476=PLANE('',#15050);
#1477=PLANE('',#15051);
#1478=PLANE('',#15052);
#1479=PLANE('',#15053);
#1480=PLANE('',#15054);
#1481=PLANE('',#15055);
#1482=PLANE('',#15056);
#1483=PLANE('',#15057);
#1484=PLANE('',#15058);
#1485=PLANE('',#15059);
#1486=PLANE('',#15060);
#1487=PLANE('',#15061);
#1488=PLANE('',#15062);
#1489=PLANE('',#15063);
#1490=PLANE('',#15064);
#1491=PLANE('',#15065);
#1492=PLANE('',#15066);
#1493=PLANE('',#15067);
#1494=PLANE('',#15068);
#1495=PLANE('',#15069);
#1496=PLANE('',#15070);
#1497=PLANE('',#15071);
#1498=PLANE('',#15072);
#1499=PLANE('',#15073);
#1500=PLANE('',#15074);
#1501=PLANE('',#15075);
#1502=PLANE('',#15076);
#1503=PLANE('',#15077);
#1504=PLANE('',#15078);
#1505=PLANE('',#15079);
#1506=PLANE('',#15080);
#1507=PLANE('',#15081);
#1508=PLANE('',#15082);
#1509=PLANE('',#15083);
#1510=PLANE('',#15084);
#1511=PLANE('',#15097);
#1512=PLANE('',#15111);
#1513=PLANE('',#15128);
#1514=PLANE('',#15137);
#1515=PLANE('',#15146);
#1516=PLANE('',#15152);
#1517=PLANE('',#15153);
#1518=PLANE('',#15157);
#1519=PLANE('',#15163);
#1520=PLANE('',#15167);
#1521=PLANE('',#15168);
#1522=PLANE('',#15170);
#1523=PLANE('',#15190);
#1524=PLANE('',#15194);
#1525=PLANE('',#15198);
#1526=PLANE('',#15202);
#1527=PLANE('',#15206);
#1528=PLANE('',#15210);
#1529=PLANE('',#15214);
#1530=PLANE('',#15218);
#1531=PLANE('',#15222);
#1532=PLANE('',#15228);
#1533=PLANE('',#15234);
#1534=PLANE('',#15240);
#1535=PLANE('',#15269);
#1536=PLANE('',#15272);
#1537=PLANE('',#15275);
#1538=CYLINDRICAL_SURFACE('',#13803,0.00322675153453757);
#1539=CYLINDRICAL_SURFACE('',#13819,0.001);
#1540=CYLINDRICAL_SURFACE('',#13824,0.001);
#1541=CYLINDRICAL_SURFACE('',#13829,0.001);
#1542=CYLINDRICAL_SURFACE('',#13878,0.00455);
#1543=CYLINDRICAL_SURFACE('',#13880,0.00455);
#1544=CYLINDRICAL_SURFACE('',#13881,0.00755);
#1545=CYLINDRICAL_SURFACE('',#13882,0.00755);
#1546=CYLINDRICAL_SURFACE('',#13883,0.05);
#1547=CYLINDRICAL_SURFACE('',#13884,0.004);
#1548=CYLINDRICAL_SURFACE('',#13885,0.00400000000000265);
#1549=CYLINDRICAL_SURFACE('',#13886,0.00400000000000387);
#1550=CYLINDRICAL_SURFACE('',#13887,0.001397);
#1551=CYLINDRICAL_SURFACE('',#13888,0.00297688);
#1552=CYLINDRICAL_SURFACE('',#13889,0.001397);
#1553=CYLINDRICAL_SURFACE('',#13890,0.00297688);
#1554=CYLINDRICAL_SURFACE('',#13891,0.001397);
#1555=CYLINDRICAL_SURFACE('',#13892,0.00297688);
#1556=CYLINDRICAL_SURFACE('',#13893,0.001397);
#1557=CYLINDRICAL_SURFACE('',#13894,0.00297688);
#1558=CYLINDRICAL_SURFACE('',#13895,0.001);
#1559=CYLINDRICAL_SURFACE('',#13896,0.001);
#1560=CYLINDRICAL_SURFACE('',#13897,0.001);
#1561=CYLINDRICAL_SURFACE('',#13898,0.01);
#1562=CYLINDRICAL_SURFACE('',#13899,0.00505);
#1563=CYLINDRICAL_SURFACE('',#13900,0.00241485272203757);
#1564=CYLINDRICAL_SURFACE('',#13911,0.00748201094464285);
#1565=CYLINDRICAL_SURFACE('',#13942,0.0045);
#1566=CYLINDRICAL_SURFACE('',#13944,0.0065);
#1567=CYLINDRICAL_SURFACE('',#13947,0.0075);
#1568=CYLINDRICAL_SURFACE('',#13951,0.003);
#1569=CYLINDRICAL_SURFACE('',#13953,0.00075);
#1570=CYLINDRICAL_SURFACE('',#13957,0.0045);
#1571=CYLINDRICAL_SURFACE('',#13958,0.0045);
#1572=CYLINDRICAL_SURFACE('',#13962,0.0099);
#1573=CYLINDRICAL_SURFACE('',#13964,0.0083);
#1574=CYLINDRICAL_SURFACE('',#13967,0.0099);
#1575=CYLINDRICAL_SURFACE('',#13980,0.0035);
#1576=CYLINDRICAL_SURFACE('',#13993,0.009236);
#1577=CYLINDRICAL_SURFACE('',#14002,0.0081692);
#1578=CYLINDRICAL_SURFACE('',#14009,0.001);
#1579=CYLINDRICAL_SURFACE('',#14023,0.001);
#1580=CYLINDRICAL_SURFACE('',#14025,0.001);
#1581=CYLINDRICAL_SURFACE('',#14027,0.001);
#1582=CYLINDRICAL_SURFACE('',#14046,0.001);
#1583=CYLINDRICAL_SURFACE('',#14047,0.001);
#1584=CYLINDRICAL_SURFACE('',#14049,0.001);
#1585=CYLINDRICAL_SURFACE('',#14055,0.001);
#1586=CYLINDRICAL_SURFACE('',#14057,0.001);
#1587=CYLINDRICAL_SURFACE('',#14077,0.001);
#1588=CYLINDRICAL_SURFACE('',#14079,0.001);
#1589=CYLINDRICAL_SURFACE('',#14085,0.001);
#1590=CYLINDRICAL_SURFACE('',#14087,0.001);
#1591=CYLINDRICAL_SURFACE('',#14111,0.001);
#1592=CYLINDRICAL_SURFACE('',#14113,0.001);
#1593=CYLINDRICAL_SURFACE('',#14119,0.001);
#1594=CYLINDRICAL_SURFACE('',#14121,0.001);
#1595=CYLINDRICAL_SURFACE('',#14137,0.001);
#1596=CYLINDRICAL_SURFACE('',#14139,0.001);
#1597=CYLINDRICAL_SURFACE('',#14145,0.001);
#1598=CYLINDRICAL_SURFACE('',#14147,0.001);
#1599=CYLINDRICAL_SURFACE('',#14166,0.001);
#1600=CYLINDRICAL_SURFACE('',#14168,0.001);
#1601=CYLINDRICAL_SURFACE('',#14181,0.00753201094464286);
#1602=CYLINDRICAL_SURFACE('',#14193,0.0125);
#1603=CYLINDRICAL_SURFACE('',#14195,0.0075);
#1604=CYLINDRICAL_SURFACE('',#14199,0.0125);
#1605=CYLINDRICAL_SURFACE('',#14202,0.0125);
#1606=CYLINDRICAL_SURFACE('',#14204,0.0075);
#1607=CYLINDRICAL_SURFACE('',#14212,0.00655);
#1608=CYLINDRICAL_SURFACE('',#14213,0.0075);
#1609=CYLINDRICAL_SURFACE('',#14214,0.0012192);
#1610=CYLINDRICAL_SURFACE('',#14215,0.00277876);
#1611=CYLINDRICAL_SURFACE('',#14216,0.0012192);
#1612=CYLINDRICAL_SURFACE('',#14217,0.00277876);
#1613=CYLINDRICAL_SURFACE('',#14218,0.0012192);
#1614=CYLINDRICAL_SURFACE('',#14219,0.00277876);
#1615=CYLINDRICAL_SURFACE('',#14258,0.0012573);
#1616=CYLINDRICAL_SURFACE('',#14268,0.004);
#1617=CYLINDRICAL_SURFACE('',#14269,0.0012192);
#1618=CYLINDRICAL_SURFACE('',#14274,0.0012192);
#1619=CYLINDRICAL_SURFACE('',#14294,0.0100000000000245);
#1620=CYLINDRICAL_SURFACE('',#14295,0.0120000000000245);
#1621=CYLINDRICAL_SURFACE('',#14296,0.0140000000000245);
#1622=CYLINDRICAL_SURFACE('',#14297,0.0045499999999755);
#1623=CYLINDRICAL_SURFACE('',#14298,0.0080000000000245);
#1624=CYLINDRICAL_SURFACE('',#14303,0.0081692);
#1625=CYLINDRICAL_SURFACE('',#14308,0.009236);
#1626=CYLINDRICAL_SURFACE('',#14315,0.009236);
#1627=CYLINDRICAL_SURFACE('',#14330,0.01);
#1628=CYLINDRICAL_SURFACE('',#14331,0.008);
#1629=CYLINDRICAL_SURFACE('',#14332,0.009236);
#1630=CYLINDRICAL_SURFACE('',#14333,0.012);
#1631=CYLINDRICAL_SURFACE('',#14347,0.012);
#1632=CYLINDRICAL_SURFACE('',#14350,0.0189);
#1633=CYLINDRICAL_SURFACE('',#14352,0.012);
#1634=CYLINDRICAL_SURFACE('',#14360,0.00325);
#1635=CYLINDRICAL_SURFACE('',#14361,0.00125);
#1636=CYLINDRICAL_SURFACE('',#14371,0.01);
#1637=CYLINDRICAL_SURFACE('',#14383,0.00331189881249999);
#1638=CYLINDRICAL_SURFACE('',#14487,0.0045);
#1639=CYLINDRICAL_SURFACE('',#14490,0.0045);
#1640=CYLINDRICAL_SURFACE('',#14493,0.0045);
#1641=CYLINDRICAL_SURFACE('',#14496,0.0045);
#1642=CYLINDRICAL_SURFACE('',#14499,0.0045);
#1643=CYLINDRICAL_SURFACE('',#14502,0.0045);
#1644=CYLINDRICAL_SURFACE('',#14505,0.0045);
#1645=CYLINDRICAL_SURFACE('',#14508,0.0045);
#1646=CYLINDRICAL_SURFACE('',#14511,0.0045);
#1647=CYLINDRICAL_SURFACE('',#14514,0.0045);
#1648=CYLINDRICAL_SURFACE('',#14517,0.0045);
#1649=CYLINDRICAL_SURFACE('',#14520,0.0045);
#1650=CYLINDRICAL_SURFACE('',#14523,0.0045);
#1651=CYLINDRICAL_SURFACE('',#14526,0.0045);
#1652=CYLINDRICAL_SURFACE('',#14529,0.0045);
#1653=CYLINDRICAL_SURFACE('',#14532,0.0045);
#1654=CYLINDRICAL_SURFACE('',#14535,0.0045);
#1655=CYLINDRICAL_SURFACE('',#14538,0.0045);
#1656=CYLINDRICAL_SURFACE('',#14541,0.0045);
#1657=CYLINDRICAL_SURFACE('',#14544,0.0045);
#1658=CYLINDRICAL_SURFACE('',#14547,0.0045);
#1659=CYLINDRICAL_SURFACE('',#14550,0.0045);
#1660=CYLINDRICAL_SURFACE('',#14553,0.0045);
#1661=CYLINDRICAL_SURFACE('',#14556,0.0045);
#1662=CYLINDRICAL_SURFACE('',#14559,0.0045);
#1663=CYLINDRICAL_SURFACE('',#14562,0.0045);
#1664=CYLINDRICAL_SURFACE('',#14565,0.0045);
#1665=CYLINDRICAL_SURFACE('',#14568,0.0045);
#1666=CYLINDRICAL_SURFACE('',#14571,0.0045);
#1667=CYLINDRICAL_SURFACE('',#14574,0.0045);
#1668=CYLINDRICAL_SURFACE('',#14577,0.0045);
#1669=CYLINDRICAL_SURFACE('',#14580,0.0045);
#1670=CYLINDRICAL_SURFACE('',#14583,0.0045);
#1671=CYLINDRICAL_SURFACE('',#14586,0.0045);
#1672=CYLINDRICAL_SURFACE('',#14589,0.0045);
#1673=CYLINDRICAL_SURFACE('',#14592,0.0045);
#1674=CYLINDRICAL_SURFACE('',#14595,0.0045);
#1675=CYLINDRICAL_SURFACE('',#14598,0.0045);
#1676=CYLINDRICAL_SURFACE('',#14601,0.0045);
#1677=CYLINDRICAL_SURFACE('',#14604,0.0045);
#1678=CYLINDRICAL_SURFACE('',#14607,0.0045);
#1679=CYLINDRICAL_SURFACE('',#14610,0.0045);
#1680=CYLINDRICAL_SURFACE('',#14613,0.0045);
#1681=CYLINDRICAL_SURFACE('',#14618,0.0045);
#1682=CYLINDRICAL_SURFACE('',#14621,0.0045);
#1683=CYLINDRICAL_SURFACE('',#14624,0.0045);
#1684=CYLINDRICAL_SURFACE('',#14627,0.0045);
#1685=CYLINDRICAL_SURFACE('',#14633,0.0025);
#1686=CYLINDRICAL_SURFACE('',#14634,0.004);
#1687=CYLINDRICAL_SURFACE('',#14635,0.00025);
#1688=CYLINDRICAL_SURFACE('',#14637,0.001);
#1689=CYLINDRICAL_SURFACE('',#14648,0.00375);
#1690=CYLINDRICAL_SURFACE('',#14649,0.00325);
#1691=CYLINDRICAL_SURFACE('',#14657,0.0188);
#1692=CYLINDRICAL_SURFACE('',#14658,0.0123);
#1693=CYLINDRICAL_SURFACE('',#14666,0.000477030566374308);
#1694=CYLINDRICAL_SURFACE('',#14668,0.000477030566374308);
#1695=CYLINDRICAL_SURFACE('',#14675,0.00322703056637436);
#1696=CYLINDRICAL_SURFACE('',#14677,0.00227296943362574);
#1697=CYLINDRICAL_SURFACE('',#14690,0.001);
#1698=CYLINDRICAL_SURFACE('',#14691,0.0035);
#1699=CYLINDRICAL_SURFACE('',#14692,0.000477030566374308);
#1700=CYLINDRICAL_SURFACE('',#14693,0.000477030566374308);
#1701=CYLINDRICAL_SURFACE('',#14694,0.00322703056637436);
#1702=CYLINDRICAL_SURFACE('',#14695,0.00227296943362574);
#1703=CYLINDRICAL_SURFACE('',#14700,0.001);
#1704=CYLINDRICAL_SURFACE('',#14706,0.001);
#1705=CYLINDRICAL_SURFACE('',#14711,0.001);
#1706=CYLINDRICAL_SURFACE('',#14741,0.045);
#1707=CYLINDRICAL_SURFACE('',#14744,0.00943317780363869);
#1708=CYLINDRICAL_SURFACE('',#14747,0.0012192);
#1709=CYLINDRICAL_SURFACE('',#14748,0.00277876);
#1710=CYLINDRICAL_SURFACE('',#14749,0.0012192);
#1711=CYLINDRICAL_SURFACE('',#14750,0.00277876);
#1712=CYLINDRICAL_SURFACE('',#14751,0.0012192);
#1713=CYLINDRICAL_SURFACE('',#14752,0.00277876);
#1714=CYLINDRICAL_SURFACE('',#14753,0.001);
#1715=CYLINDRICAL_SURFACE('',#14754,0.001);
#1716=CYLINDRICAL_SURFACE('',#14755,0.001);
#1717=CYLINDRICAL_SURFACE('',#14770,0.001);
#1718=CYLINDRICAL_SURFACE('',#14777,0.001);
#1719=CYLINDRICAL_SURFACE('',#14784,0.001);
#1720=CYLINDRICAL_SURFACE('',#14795,0.045);
#1721=CYLINDRICAL_SURFACE('',#14796,0.00943317780363869);
#1722=CYLINDRICAL_SURFACE('',#14797,0.001);
#1723=CYLINDRICAL_SURFACE('',#14798,0.001);
#1724=CYLINDRICAL_SURFACE('',#14799,0.001);
#1725=CYLINDRICAL_SURFACE('',#14810,0.000477030566374308);
#1726=CYLINDRICAL_SURFACE('',#14812,0.000477030566374308);
#1727=CYLINDRICAL_SURFACE('',#14819,0.00322703056637436);
#1728=CYLINDRICAL_SURFACE('',#14821,0.00227296943362574);
#1729=CYLINDRICAL_SURFACE('',#14835,0.0035);
#1730=CYLINDRICAL_SURFACE('',#14841,0.001);
#1731=CYLINDRICAL_SURFACE('',#14842,0.0035);
#1732=CYLINDRICAL_SURFACE('',#14843,0.000477030566374308);
#1733=CYLINDRICAL_SURFACE('',#14844,0.000477030566374308);
#1734=CYLINDRICAL_SURFACE('',#14845,0.00322703056637436);
#1735=CYLINDRICAL_SURFACE('',#14846,0.00227296943362574);
#1736=CYLINDRICAL_SURFACE('',#14851,0.005);
#1737=CYLINDRICAL_SURFACE('',#14860,0.005);
#1738=CYLINDRICAL_SURFACE('',#14874,0.005);
#1739=CYLINDRICAL_SURFACE('',#14882,0.005);
#1740=CYLINDRICAL_SURFACE('',#14904,0.005);
#1741=CYLINDRICAL_SURFACE('',#14912,0.005);
#1742=CYLINDRICAL_SURFACE('',#14914,0.003);
#1743=CYLINDRICAL_SURFACE('',#14916,0.003);
#1744=CYLINDRICAL_SURFACE('',#14918,0.003);
#1745=CYLINDRICAL_SURFACE('',#14920,0.003);
#1746=CYLINDRICAL_SURFACE('',#14923,0.003);
#1747=CYLINDRICAL_SURFACE('',#14925,0.003);
#1748=CYLINDRICAL_SURFACE('',#14928,0.003);
#1749=CYLINDRICAL_SURFACE('',#14930,0.003);
#1750=CYLINDRICAL_SURFACE('',#14935,0.0108118988125);
#1751=CYLINDRICAL_SURFACE('',#14941,0.000199965309748703);
#1752=CYLINDRICAL_SURFACE('',#14943,0.000199947311632309);
#1753=CYLINDRICAL_SURFACE('',#14964,0.01);
#1754=CYLINDRICAL_SURFACE('',#14965,0.019);
#1755=CYLINDRICAL_SURFACE('',#14968,0.0121);
#1756=CYLINDRICAL_SURFACE('',#14971,0.016);
#1757=CYLINDRICAL_SURFACE('',#14974,0.05);
#1758=CYLINDRICAL_SURFACE('',#14983,0.013);
#1759=CYLINDRICAL_SURFACE('',#14991,0.001397);
#1760=CYLINDRICAL_SURFACE('',#14992,0.001397);
#1761=CYLINDRICAL_SURFACE('',#14993,0.001397);
#1762=CYLINDRICAL_SURFACE('',#14994,0.001397);
#1763=CYLINDRICAL_SURFACE('',#14995,0.053);
#1764=CYLINDRICAL_SURFACE('',#14996,0.005);
#1765=CYLINDRICAL_SURFACE('',#14997,0.005);
#1766=CYLINDRICAL_SURFACE('',#14998,0.05);
#1767=CYLINDRICAL_SURFACE('',#15006,0.001);
#1768=CYLINDRICAL_SURFACE('',#15013,0.001);
#1769=CYLINDRICAL_SURFACE('',#15020,0.001);
#1770=CYLINDRICAL_SURFACE('',#15039,0.05);
#1771=CYLINDRICAL_SURFACE('',#15040,0.00400000000000387);
#1772=CYLINDRICAL_SURFACE('',#15041,0.004);
#1773=CYLINDRICAL_SURFACE('',#15042,0.00755);
#1774=CYLINDRICAL_SURFACE('',#15043,0.00400000000000265);
#1775=CYLINDRICAL_SURFACE('',#15044,0.001);
#1776=CYLINDRICAL_SURFACE('',#15045,0.001);
#1777=CYLINDRICAL_SURFACE('',#15046,0.001);
#1778=CYLINDRICAL_SURFACE('',#15047,0.01);
#1779=CYLINDRICAL_SURFACE('',#15110,0.00736858102143575);
#1780=CYLINDRICAL_SURFACE('',#15114,0.00736858102143575);
#1781=CYLINDRICAL_SURFACE('',#15115,0.00736858102143575);
#1782=CYLINDRICAL_SURFACE('',#15116,0.00736858102143575);
#1783=CYLINDRICAL_SURFACE('',#15117,0.00736858102143575);
#1784=CYLINDRICAL_SURFACE('',#15118,0.00736858102143575);
#1785=CYLINDRICAL_SURFACE('',#15119,0.00736858102143575);
#1786=CYLINDRICAL_SURFACE('',#15120,0.00736858102143575);
#1787=CYLINDRICAL_SURFACE('',#15121,0.00736858102143575);
#1788=CYLINDRICAL_SURFACE('',#15122,0.00736858102143575);
#1789=CYLINDRICAL_SURFACE('',#15123,0.00736858102143575);
#1790=CYLINDRICAL_SURFACE('',#15124,0.005);
#1791=CYLINDRICAL_SURFACE('',#15125,0.0004);
#1792=CYLINDRICAL_SURFACE('',#15133,0.00322703056637436);
#1793=CYLINDRICAL_SURFACE('',#15135,0.00227296943362574);
#1794=CYLINDRICAL_SURFACE('',#15142,0.000477030566374308);
#1795=CYLINDRICAL_SURFACE('',#15144,0.000477030566374308);
#1796=CYLINDRICAL_SURFACE('',#15151,0.0107118988125);
#1797=CYLINDRICAL_SURFACE('',#15154,0.00209191070279862);
#1798=CYLINDRICAL_SURFACE('',#15160,0.008);
#1799=CYLINDRICAL_SURFACE('',#15169,0.0025);
#1800=CYLINDRICAL_SURFACE('',#15178,0.0099);
#1801=CYLINDRICAL_SURFACE('',#15179,0.008);
#1802=CYLINDRICAL_SURFACE('',#15180,0.0015);
#1803=CYLINDRICAL_SURFACE('',#15181,0.001);
#1804=CYLINDRICAL_SURFACE('',#15184,0.0035);
#1805=CYLINDRICAL_SURFACE('',#15185,0.00322703056637436);
#1806=CYLINDRICAL_SURFACE('',#15186,0.00227296943362574);
#1807=CYLINDRICAL_SURFACE('',#15187,0.000477030566374308);
#1808=CYLINDRICAL_SURFACE('',#15188,0.000477030566374308);
#1809=CYLINDRICAL_SURFACE('',#15191,0.006);
#1810=CYLINDRICAL_SURFACE('',#15195,0.003);
#1811=CYLINDRICAL_SURFACE('',#15199,0.006);
#1812=CYLINDRICAL_SURFACE('',#15203,0.003);
#1813=CYLINDRICAL_SURFACE('',#15207,0.006);
#1814=CYLINDRICAL_SURFACE('',#15211,0.003);
#1815=CYLINDRICAL_SURFACE('',#15215,0.006);
#1816=CYLINDRICAL_SURFACE('',#15219,0.003);
#1817=CYLINDRICAL_SURFACE('',#15252,0.00180420299878392);
#1818=CYLINDRICAL_SURFACE('',#15254,0.008);
#1819=CYLINDRICAL_SURFACE('',#15264,0.00100009891588755);
#1820=CYLINDRICAL_SURFACE('',#15267,0.000199929791356894);
#1821=CYLINDRICAL_SURFACE('',#15268,0.000199893207290678);
#1822=CYLINDRICAL_SURFACE('',#15278,0.0192);
#1823=CYLINDRICAL_SURFACE('',#15281,0.0120000000000245);
#1824=CYLINDRICAL_SURFACE('',#15283,0.0212);
#1825=CYLINDRICAL_SURFACE('',#15290,0.01);
#1826=(
BOUNDED_CURVE()
B_SPLINE_CURVE(2,(#19227,#19228,#19229,#19230,#19231,#19232,#19233,#19234,
#19235),.UNSPECIFIED.,.F.,.F.)
B_SPLINE_CURVE_WITH_KNOTS((3,2,2,2,3),(0.,0.03125,0.0625,0.09375,0.125),
 .UNSPECIFIED.)
CURVE()
GEOMETRIC_REPRESENTATION_ITEM()
RATIONAL_B_SPLINE_CURVE((1.,0.923879532511287,1.,0.923879532511287,1.,0.923879532511287,
1.,0.923879532511287,1.))
REPRESENTATION_ITEM('')
);
#1827=(
BOUNDED_CURVE()
B_SPLINE_CURVE(2,(#19237,#19238,#19239,#19240,#19241,#19242,#19243,#19244,
#19245),.UNSPECIFIED.,.F.,.F.)
B_SPLINE_CURVE_WITH_KNOTS((3,2,2,2,3),(0.125,0.15625,0.1875,0.21875,0.25),
 .UNSPECIFIED.)
CURVE()
GEOMETRIC_REPRESENTATION_ITEM()
RATIONAL_B_SPLINE_CURVE((1.,0.923879532511287,1.,0.923879532511287,1.,0.923879532511287,
1.,0.923879532511287,1.))
REPRESENTATION_ITEM('')
);
#1828=(
BOUNDED_CURVE()
B_SPLINE_CURVE(2,(#19247,#19248,#19249,#19250,#19251,#19252,#19253,#19254,
#19255),.UNSPECIFIED.,.F.,.F.)
B_SPLINE_CURVE_WITH_KNOTS((3,2,2,2,3),(0.25,0.28125,0.3125,0.34375,0.375),
 .UNSPECIFIED.)
CURVE()
GEOMETRIC_REPRESENTATION_ITEM()
RATIONAL_B_SPLINE_CURVE((1.,0.923879532511287,1.,0.923879532511287,1.,0.923879532511287,
1.,0.923879532511287,1.))
REPRESENTATION_ITEM('')
);
#1829=(
BOUNDED_CURVE()
B_SPLINE_CURVE(2,(#19257,#19258,#19259,#19260,#19261,#19262,#19263,#19264,
#19265),.UNSPECIFIED.,.F.,.F.)
B_SPLINE_CURVE_WITH_KNOTS((3,2,2,2,3),(0.375,0.40625,0.4375,0.46875,0.5),
 .UNSPECIFIED.)
CURVE()
GEOMETRIC_REPRESENTATION_ITEM()
RATIONAL_B_SPLINE_CURVE((1.,0.923879532511287,1.,0.923879532511287,1.,0.923879532511287,
1.,0.923879532511287,1.))
REPRESENTATION_ITEM('')
);
#1830=(
BOUNDED_CURVE()
B_SPLINE_CURVE(2,(#19267,#19268,#19269,#19270,#19271,#19272,#19273,#19274,
#19275),.UNSPECIFIED.,.F.,.F.)
B_SPLINE_CURVE_WITH_KNOTS((3,2,2,2,3),(0.5,0.53125,0.5625,0.59375,0.625),
 .UNSPECIFIED.)
CURVE()
GEOMETRIC_REPRESENTATION_ITEM()
RATIONAL_B_SPLINE_CURVE((1.,0.923879532511287,1.,0.923879532511287,1.,0.923879532511287,
1.,0.923879532511287,1.))
REPRESENTATION_ITEM('')
);
#1831=(
BOUNDED_CURVE()
B_SPLINE_CURVE(2,(#19277,#19278,#19279,#19280,#19281,#19282,#19283,#19284,
#19285),.UNSPECIFIED.,.F.,.F.)
B_SPLINE_CURVE_WITH_KNOTS((3,2,2,2,3),(0.625,0.65625,0.6875,0.71875,0.75),
 .UNSPECIFIED.)
CURVE()
GEOMETRIC_REPRESENTATION_ITEM()
RATIONAL_B_SPLINE_CURVE((1.,0.923879532511287,1.,0.923879532511287,1.,0.923879532511287,
1.,0.923879532511287,1.))
REPRESENTATION_ITEM('')
);
#1832=(
BOUNDED_CURVE()
B_SPLINE_CURVE(2,(#19287,#19288,#19289,#19290,#19291,#19292,#19293,#19294,
#19295),.UNSPECIFIED.,.F.,.F.)
B_SPLINE_CURVE_WITH_KNOTS((3,2,2,2,3),(0.75,0.78125,0.8125,0.84375,0.875),
 .UNSPECIFIED.)
CURVE()
GEOMETRIC_REPRESENTATION_ITEM()
RATIONAL_B_SPLINE_CURVE((1.,0.923879532511287,1.,0.923879532511287,1.,0.923879532511287,
1.,0.923879532511287,1.))
REPRESENTATION_ITEM('')
);
#1833=(
BOUNDED_CURVE()
B_SPLINE_CURVE(2,(#19299,#19300,#19301,#19302,#19303,#19304,#19305,#19306,
#19307,#19308,#19309,#19310,#19311,#19312,#19313,#19314,#19315,#19316,#19317,
#19318,#19319,#19320,#19321,#19322,#19323,#19324,#19325,#19326,#19327,#19328,
#19329,#19330,#19331,#19332,#19333,#19334,#19335,#19336,#19337,#19338,#19339,
#19340,#19341,#19342,#19343,#19344,#19345,#19346,#19347,#19348,#19349,#19350,
#19351,#19352,#19353,#19354,#19355),.UNSPECIFIED.,.F.,.F.)
B_SPLINE_CURVE_WITH_KNOTS((3,2,2,2,2,2,2,2,2,2,2,2,2,2,2,2,2,2,2,2,2,2,
2,2,2,2,2,2,3),(0.,0.03125,0.0625,0.09375,0.125,0.15625,0.1875,0.21875,
0.25,0.28125,0.3125,0.34375,0.375,0.40625,0.4375,0.46875,0.5,0.53125,0.5625,
0.59375,0.625,0.65625,0.6875,0.71875,0.75,0.78125,0.8125,0.84375,0.875),
 .UNSPECIFIED.)
CURVE()
GEOMETRIC_REPRESENTATION_ITEM()
RATIONAL_B_SPLINE_CURVE((1.,0.923879532511287,1.,0.923879532511287,1.,0.923879532511287,
1.,0.923879532511287,1.,0.923879532511287,1.,0.923879532511287,1.,0.923879532511287,
1.,0.923879532511287,1.,0.923879532511287,1.,0.923879532511287,1.,0.923879532511287,
1.,0.923879532511287,1.,0.923879532511287,1.,0.923879532511287,1.,0.923879532511287,
1.,0.923879532511287,1.,0.923879532511287,1.,0.923879532511287,1.,0.923879532511287,
1.,0.923879532511287,1.,0.923879532511287,1.,0.923879532511287,1.,0.923879532511287,
1.,0.923879532511287,1.,0.923879532511287,1.,0.923879532511287,1.,0.923879532511287,
1.,0.923879532511287,1.))
REPRESENTATION_ITEM('')
);
#1834=(
BOUNDED_CURVE()
B_SPLINE_CURVE(2,(#19361,#19362,#19363,#19364,#19365,#19366,#19367,#19368,
#19369,#19370,#19371,#19372,#19373,#19374,#19375,#19376,#19377,#19378,#19379,
#19380,#19381,#19382,#19383,#19384,#19385,#19386,#19387,#19388,#19389,#19390,
#19391,#19392,#19393,#19394,#19395,#19396,#19397,#19398,#19399,#19400,#19401,
#19402,#19403,#19404,#19405,#19406,#19407,#19408,#19409,#19410,#19411,#19412,
#19413,#19414,#19415,#19416,#19417),.UNSPECIFIED.,.F.,.F.)
B_SPLINE_CURVE_WITH_KNOTS((3,2,2,2,2,2,2,2,2,2,2,2,2,2,2,2,2,2,2,2,2,2,
2,2,2,2,2,2,3),(0.,0.03125,0.0625,0.09375,0.125,0.15625,0.1875,0.21875,
0.25,0.28125,0.3125,0.34375,0.375,0.40625,0.4375,0.46875,0.5,0.53125,0.5625,
0.59375,0.625,0.65625,0.6875,0.71875,0.75,0.78125,0.8125,0.84375,0.875),
 .UNSPECIFIED.)
CURVE()
GEOMETRIC_REPRESENTATION_ITEM()
RATIONAL_B_SPLINE_CURVE((1.,0.923879532511287,1.,0.923879532511287,1.,0.923879532511287,
1.,0.923879532511287,1.,0.923879532511287,1.,0.923879532511287,1.,0.923879532511287,
1.,0.923879532511287,1.,0.923879532511287,1.,0.923879532511287,1.,0.923879532511287,
1.,0.923879532511287,1.,0.923879532511287,1.,0.923879532511287,1.,0.923879532511287,
1.,0.923879532511287,1.,0.923879532511287,1.,0.923879532511287,1.,0.923879532511287,
1.,0.923879532511287,1.,0.923879532511287,1.,0.923879532511287,1.,0.923879532511287,
1.,0.923879532511287,1.,0.923879532511287,1.,0.923879532511287,1.,0.923879532511287,
1.,0.923879532511287,1.))
REPRESENTATION_ITEM('')
);
#1835=(
BOUNDED_CURVE()
B_SPLINE_CURVE(2,(#19543,#19544,#19545,#19546,#19547,#19548,#19549,#19550,
#19551),.UNSPECIFIED.,.F.,.F.)
B_SPLINE_CURVE_WITH_KNOTS((3,2,2,2,3),(0.75,0.78125,0.8125,0.84375,0.875),
 .UNSPECIFIED.)
CURVE()
GEOMETRIC_REPRESENTATION_ITEM()
RATIONAL_B_SPLINE_CURVE((1.,0.923879532511287,1.,0.923879532511287,1.,0.923879532511287,
1.,0.923879532511287,1.))
REPRESENTATION_ITEM('')
);
#1836=(
BOUNDED_CURVE()
B_SPLINE_CURVE(2,(#19553,#19554,#19555,#19556,#19557,#19558,#19559,#19560,
#19561),.UNSPECIFIED.,.F.,.F.)
B_SPLINE_CURVE_WITH_KNOTS((3,2,2,2,3),(0.625,0.65625,0.6875,0.71875,0.75),
 .UNSPECIFIED.)
CURVE()
GEOMETRIC_REPRESENTATION_ITEM()
RATIONAL_B_SPLINE_CURVE((1.,0.923879532511287,1.,0.923879532511287,1.,0.923879532511287,
1.,0.923879532511287,1.))
REPRESENTATION_ITEM('')
);
#1837=(
BOUNDED_CURVE()
B_SPLINE_CURVE(2,(#19563,#19564,#19565,#19566,#19567,#19568,#19569,#19570,
#19571),.UNSPECIFIED.,.F.,.F.)
B_SPLINE_CURVE_WITH_KNOTS((3,2,2,2,3),(0.5,0.53125,0.5625,0.59375,0.625),
 .UNSPECIFIED.)
CURVE()
GEOMETRIC_REPRESENTATION_ITEM()
RATIONAL_B_SPLINE_CURVE((1.,0.923879532511287,1.,0.923879532511287,1.,0.923879532511287,
1.,0.923879532511287,1.))
REPRESENTATION_ITEM('')
);
#1838=(
BOUNDED_CURVE()
B_SPLINE_CURVE(2,(#19573,#19574,#19575,#19576,#19577,#19578,#19579,#19580,
#19581),.UNSPECIFIED.,.F.,.F.)
B_SPLINE_CURVE_WITH_KNOTS((3,2,2,2,3),(0.375,0.40625,0.4375,0.46875,0.5),
 .UNSPECIFIED.)
CURVE()
GEOMETRIC_REPRESENTATION_ITEM()
RATIONAL_B_SPLINE_CURVE((1.,0.923879532511287,1.,0.923879532511287,1.,0.923879532511287,
1.,0.923879532511287,1.))
REPRESENTATION_ITEM('')
);
#1839=(
BOUNDED_CURVE()
B_SPLINE_CURVE(2,(#19583,#19584,#19585,#19586,#19587,#19588,#19589,#19590,
#19591),.UNSPECIFIED.,.F.,.F.)
B_SPLINE_CURVE_WITH_KNOTS((3,2,2,2,3),(0.25,0.28125,0.3125,0.34375,0.375),
 .UNSPECIFIED.)
CURVE()
GEOMETRIC_REPRESENTATION_ITEM()
RATIONAL_B_SPLINE_CURVE((1.,0.923879532511287,1.,0.923879532511287,1.,0.923879532511287,
1.,0.923879532511287,1.))
REPRESENTATION_ITEM('')
);
#1840=(
BOUNDED_CURVE()
B_SPLINE_CURVE(2,(#19593,#19594,#19595,#19596,#19597,#19598,#19599,#19600,
#19601),.UNSPECIFIED.,.F.,.F.)
B_SPLINE_CURVE_WITH_KNOTS((3,2,2,2,3),(0.125,0.15625,0.1875,0.21875,0.25),
 .UNSPECIFIED.)
CURVE()
GEOMETRIC_REPRESENTATION_ITEM()
RATIONAL_B_SPLINE_CURVE((1.,0.923879532511287,1.,0.923879532511287,1.,0.923879532511287,
1.,0.923879532511287,1.))
REPRESENTATION_ITEM('')
);
#1841=(
BOUNDED_CURVE()
B_SPLINE_CURVE(2,(#19603,#19604,#19605,#19606,#19607,#19608,#19609),
 .UNSPECIFIED.,.F.,.F.)
B_SPLINE_CURVE_WITH_KNOTS((3,2,2,3),(0.0418443486222184,0.0625,0.09375,
0.125),.UNSPECIFIED.)
CURVE()
GEOMETRIC_REPRESENTATION_ITEM()
RATIONAL_B_SPLINE_CURVE((0.965885064534014,0.94968582914686,1.,0.923879532511287,
1.,0.923879532511287,1.))
REPRESENTATION_ITEM('')
);
#1842=(
BOUNDED_CURVE()
B_SPLINE_CURVE(2,(#19957,#19958,#19959,#19960,#19961,#19962,#19963,#19964,
#19965,#19966,#19967,#19968,#19969,#19970,#19971,#19972,#19973,#19974,#19975,
#19976,#19977,#19978,#19979,#19980,#19981,#19982,#19983,#19984,#19985,#19986,
#19987,#19988,#19989,#19990,#19991),.UNSPECIFIED.,.F.,.F.)
B_SPLINE_CURVE_WITH_KNOTS((3,2,2,2,2,2,2,2,2,2,2,2,2,2,2,2,2,3),(0.,0.05,
0.1,0.15,0.2,0.25,0.3,0.35,0.4,0.45,0.5,0.55,0.6,0.65,0.7,0.75,0.8,0.826757086852849),
 .UNSPECIFIED.)
CURVE()
GEOMETRIC_REPRESENTATION_ITEM()
RATIONAL_B_SPLINE_CURVE((1.,0.951056516295154,1.,0.951056516295154,1.,0.951056516295154,
1.,0.951056516295154,1.,0.951056516295154,1.,0.951056516295154,1.,0.951056516295154,
1.,0.951056516295154,1.,0.951056516295154,1.,0.951056516295154,1.,0.951056516295154,
1.,0.951056516295154,1.,0.951056516295154,1.,0.951056516295154,1.,0.951056516295154,
1.,0.951056516295154,1.,0.973808299112568,0.975649142843891))
REPRESENTATION_ITEM('')
);
#1843=(
BOUNDED_CURVE()
B_SPLINE_CURVE(2,(#20005,#20006,#20007,#20008,#20009,#20010,#20011,#20012,
#20013,#20014,#20015),.UNSPECIFIED.,.F.,.F.)
B_SPLINE_CURVE_WITH_KNOTS((3,2,2,2,2,3),(0.5,0.55,0.6,0.65,0.7,0.75),
 .UNSPECIFIED.)
CURVE()
GEOMETRIC_REPRESENTATION_ITEM()
RATIONAL_B_SPLINE_CURVE((1.,0.951056516295153,1.,0.951056516295154,1.,0.951056516295154,
1.,0.951056516295154,1.,0.951056516295155,1.))
REPRESENTATION_ITEM('')
);
#1844=(
BOUNDED_CURVE()
B_SPLINE_CURVE(2,(#20017,#20018,#20019,#20020,#20021,#20022,#20023,#20024,
#20025,#20026,#20027),.UNSPECIFIED.,.F.,.F.)
B_SPLINE_CURVE_WITH_KNOTS((3,2,2,2,2,3),(0.25,0.3,0.35,0.4,0.45,0.5),
 .UNSPECIFIED.)
CURVE()
GEOMETRIC_REPRESENTATION_ITEM()
RATIONAL_B_SPLINE_CURVE((1.,0.951056516295153,1.,0.951056516295154,1.,0.951056516295154,
1.,0.951056516295154,1.,0.951056516295154,1.))
REPRESENTATION_ITEM('')
);
#1845=(
BOUNDED_CURVE()
B_SPLINE_CURVE(2,(#20029,#20030,#20031,#20032,#20033,#20034,#20035,#20036,
#20037,#20038,#20039),.UNSPECIFIED.,.F.,.F.)
B_SPLINE_CURVE_WITH_KNOTS((3,2,2,2,2,3),(0.,0.05,0.1,0.15,0.2,0.25),
 .UNSPECIFIED.)
CURVE()
GEOMETRIC_REPRESENTATION_ITEM()
RATIONAL_B_SPLINE_CURVE((1.,0.951056516295154,1.,0.951056516295154,1.,0.951056516295154,
1.,0.951056516295154,1.,0.951056516295154,1.))
REPRESENTATION_ITEM('')
);
#1846=(
BOUNDED_CURVE()
B_SPLINE_CURVE(2,(#20267,#20268,#20269,#20270,#20271,#20272,#20273,#20274,
#20275,#20276,#20277),.UNSPECIFIED.,.F.,.F.)
B_SPLINE_CURVE_WITH_KNOTS((3,2,2,2,2,3),(0.,0.05,0.1,0.15,0.2,0.25),
 .UNSPECIFIED.)
CURVE()
GEOMETRIC_REPRESENTATION_ITEM()
RATIONAL_B_SPLINE_CURVE((1.,0.951056516295154,1.,0.951056516295154,1.,0.951056516295154,
1.,0.951056516295154,1.,0.951056516295154,1.))
REPRESENTATION_ITEM('')
);
#1847=(
BOUNDED_CURVE()
B_SPLINE_CURVE(2,(#20279,#20280,#20281,#20282,#20283,#20284,#20285,#20286,
#20287,#20288,#20289),.UNSPECIFIED.,.F.,.F.)
B_SPLINE_CURVE_WITH_KNOTS((3,2,2,2,2,3),(0.25,0.3,0.35,0.4,0.45,0.5),
 .UNSPECIFIED.)
CURVE()
GEOMETRIC_REPRESENTATION_ITEM()
RATIONAL_B_SPLINE_CURVE((1.,0.951056516295153,1.,0.951056516295154,1.,0.951056516295154,
1.,0.951056516295154,1.,0.951056516295154,1.))
REPRESENTATION_ITEM('')
);
#1848=(
BOUNDED_CURVE()
B_SPLINE_CURVE(2,(#20291,#20292,#20293,#20294,#20295,#20296,#20297,#20298,
#20299,#20300,#20301),.UNSPECIFIED.,.F.,.F.)
B_SPLINE_CURVE_WITH_KNOTS((3,2,2,2,2,3),(0.5,0.55,0.6,0.65,0.7,0.75),
 .UNSPECIFIED.)
CURVE()
GEOMETRIC_REPRESENTATION_ITEM()
RATIONAL_B_SPLINE_CURVE((1.,0.951056516295153,1.,0.951056516295154,1.,0.951056516295154,
1.,0.951056516295154,1.,0.951056516295155,1.))
REPRESENTATION_ITEM('')
);
#1849=(
BOUNDED_CURVE()
B_SPLINE_CURVE(2,(#20303,#20304,#20305,#20306,#20307),.UNSPECIFIED.,.F.,
 .F.)
B_SPLINE_CURVE_WITH_KNOTS((3,2,3),(0.75,0.8,0.826757130829527),
 .UNSPECIFIED.)
CURVE()
GEOMETRIC_REPRESENTATION_ITEM()
RATIONAL_B_SPLINE_CURVE((1.,0.951056516295153,1.,0.973808256065132,0.975649148895013))
REPRESENTATION_ITEM('')
);
#1850=(
BOUNDED_CURVE()
B_SPLINE_CURVE(2,(#20311,#20312,#20313,#20314,#20315,#20316,#20317,#20318,
#20319,#20320,#20321,#20322,#20323,#20324,#20325,#20326,#20327,#20328,#20329,
#20330,#20331,#20332,#20333,#20334,#20335,#20336,#20337,#20338,#20339,#20340,
#20341,#20342,#20343,#20344,#20345),.UNSPECIFIED.,.F.,.F.)
B_SPLINE_CURVE_WITH_KNOTS((3,2,2,2,2,2,2,2,2,2,2,2,2,2,2,2,2,3),(0.,0.05,
0.1,0.15,0.2,0.25,0.3,0.35,0.4,0.45,0.5,0.55,0.6,0.65,0.7,0.75,0.8,0.826757072590209),
 .UNSPECIFIED.)
CURVE()
GEOMETRIC_REPRESENTATION_ITEM()
RATIONAL_B_SPLINE_CURVE((1.,0.951056516295154,1.,0.951056516295154,1.,0.951056516295154,
1.,0.951056516295154,1.,0.951056516295154,1.,0.951056516295154,1.,0.951056516295154,
1.,0.951056516295154,1.,0.951056516295154,1.,0.951056516295154,1.,0.951056516295154,
1.,0.951056516295154,1.,0.951056516295154,1.,0.951056516295154,1.,0.951056516295154,
1.,0.951056516295154,1.,0.973808313073834,0.975649140881406))
REPRESENTATION_ITEM('')
);
#1851=(
BOUNDED_CURVE()
B_SPLINE_CURVE(2,(#27231,#27232,#27233,#27234,#27235,#27236,#27237,#27238,
#27239,#27240,#27241,#27242,#27243,#27244,#27245,#27246,#27247,#27248,#27249,
#27250,#27251,#27252,#27253,#27254,#27255,#27256,#27257,#27258,#27259,#27260,
#27261,#27262,#27263,#27264,#27265,#27266,#27267,#27268,#27269,#27270,#27271,
#27272,#27273),.UNSPECIFIED.,.F.,.F.)
B_SPLINE_CURVE_WITH_KNOTS((3,2,2,2,2,2,2,2,2,2,2,2,2,2,2,2,2,2,2,2,2,3),
(0.253327980224673,0.277777777777778,0.305555555555555,0.333333333333334,
0.361111111111111,0.388888888888889,0.416666666666667,0.444444444444444,
0.472222222222222,0.5,0.527777777777778,0.555555555555556,0.583333333333333,
0.611111111111111,0.638888888888889,0.666666666666667,0.694444444444444,
0.722222222222222,0.75,0.777777777777778,0.805555555555556,0.833333333333333),
 .UNSPECIFIED.)
CURVE()
GEOMETRIC_REPRESENTATION_ITEM()
RATIONAL_B_SPLINE_CURVE((0.992813518121856,0.970008160635222,1.,0.965925826289068,
1.,0.965925826289068,1.,0.965925826289068,1.,0.965925826289068,1.,0.965925826289068,
1.,0.965925826289068,1.,0.965925826289068,1.,0.965925826289068,1.,0.965925826289068,
1.,0.965925826289068,1.,0.965925826289068,1.,0.965925826289068,1.,0.965925826289068,
1.,0.965925826289068,1.,0.965925826289068,1.,0.965925826289068,1.,0.965925826289068,
1.,0.965925826289068,1.,0.965925826289068,1.,0.965925826289068,1.))
REPRESENTATION_ITEM('')
);
#1852=(
BOUNDED_CURVE()
B_SPLINE_CURVE(2,(#27285,#27286,#27287,#27288,#27289),.UNSPECIFIED.,.F.,
 .F.)
B_SPLINE_CURVE_WITH_KNOTS((3,2,3),(0.27956288087666,0.305555555555555,0.333333333333333),
 .UNSPECIFIED.)
CURVE()
GEOMETRIC_REPRESENTATION_ITEM()
RATIONAL_B_SPLINE_CURVE((0.995901974981237,0.968115559160064,1.,0.965925826289069,
1.))
REPRESENTATION_ITEM('')
);
#1853=(
BOUNDED_CURVE()
B_SPLINE_CURVE(2,(#27291,#27292,#27293,#27294,#27295,#27296,#27297,#27298,
#27299,#27300,#27301,#27302,#27303),.UNSPECIFIED.,.F.,.F.)
B_SPLINE_CURVE_WITH_KNOTS((3,2,2,2,2,2,3),(0.333333333333333,0.361111111111111,
0.388888888888889,0.416666666666667,0.444444444444444,0.472222222222222,
0.5),.UNSPECIFIED.)
CURVE()
GEOMETRIC_REPRESENTATION_ITEM()
RATIONAL_B_SPLINE_CURVE((1.,0.965925826289068,1.,0.965925826289068,1.,0.965925826289068,
1.,0.965925826289068,1.,0.965925826289068,1.,0.965925826289068,1.))
REPRESENTATION_ITEM('')
);
#1854=(
BOUNDED_CURVE()
B_SPLINE_CURVE(2,(#27305,#27306,#27307,#27308,#27309,#27310,#27311,#27312,
#27313,#27314,#27315,#27316,#27317),.UNSPECIFIED.,.F.,.F.)
B_SPLINE_CURVE_WITH_KNOTS((3,2,2,2,2,2,3),(0.5,0.527777777777778,0.555555555555556,
0.583333333333333,0.611111111111111,0.638888888888889,0.666666666666666),
 .UNSPECIFIED.)
CURVE()
GEOMETRIC_REPRESENTATION_ITEM()
RATIONAL_B_SPLINE_CURVE((1.,0.965925826289069,1.,0.965925826289068,1.,0.965925826289068,
1.,0.965925826289068,1.,0.965925826289068,1.,0.965925826289069,1.))
REPRESENTATION_ITEM('')
);
#1855=(
BOUNDED_CURVE()
B_SPLINE_CURVE(2,(#27319,#27320,#27321,#27322,#27323,#27324,#27325,#27326,
#27327,#27328,#27329,#27330,#27331),.UNSPECIFIED.,.F.,.F.)
B_SPLINE_CURVE_WITH_KNOTS((3,2,2,2,2,2,3),(0.666666666666666,0.694444444444444,
0.722222222222222,0.75,0.777777777777778,0.805555555555556,0.833333333333333),
 .UNSPECIFIED.)
CURVE()
GEOMETRIC_REPRESENTATION_ITEM()
RATIONAL_B_SPLINE_CURVE((1.,0.965925826289068,1.,0.965925826289068,1.,0.965925826289068,
1.,0.965925826289068,1.,0.965925826289068,1.,0.965925826289068,1.))
REPRESENTATION_ITEM('')
);
#1856=(
BOUNDED_CURVE()
B_SPLINE_CURVE(2,(#27424,#27425,#27426,#27427,#27428,#27429,#27430,#27431,
#27432,#27433,#27434,#27435,#27436,#27437,#27438,#27439,#27440,#27441,#27442,
#27443,#27444,#27445,#27446,#27447,#27448,#27449,#27450,#27451,#27452,#27453,
#27454,#27455,#27456,#27457,#27458,#27459,#27460,#27461,#27462,#27463,#27464,
#27465,#27466,#27467,#27468),.UNSPECIFIED.,.F.,.F.)
B_SPLINE_CURVE_WITH_KNOTS((3,2,2,2,2,2,2,2,2,2,2,2,2,2,2,2,2,2,2,2,2,2,
3),(0.241197850932585,0.25,0.277777777777778,0.305555555555555,0.333333333333334,
0.361111111111111,0.388888888888889,0.416666666666667,0.444444444444444,
0.472222222222222,0.5,0.527777777777778,0.555555555555556,0.583333333333333,
0.611111111111111,0.638888888888889,0.666666666666667,0.694444444444444,
0.722222222222222,0.75,0.777777777777778,0.805555555555556,0.833333333333333),
 .UNSPECIFIED.)
CURVE()
GEOMETRIC_REPRESENTATION_ITEM()
RATIONAL_B_SPLINE_CURVE((0.985248192939002,0.989202665571305,1.,0.965925826289068,
1.,0.965925826289068,1.,0.965925826289068,1.,0.965925826289068,1.,0.965925826289068,
1.,0.965925826289068,1.,0.965925826289068,1.,0.965925826289068,1.,0.965925826289068,
1.,0.965925826289068,1.,0.965925826289068,1.,0.965925826289068,1.,0.965925826289068,
1.,0.965925826289068,1.,0.965925826289068,1.,0.965925826289068,1.,0.965925826289068,
1.,0.965925826289068,1.,0.965925826289068,1.,0.965925826289068,1.,0.965925826289068,
1.))
REPRESENTATION_ITEM('')
);
#1857=(
BOUNDED_CURVE()
B_SPLINE_CURVE(2,(#27664,#27665,#27666,#27667,#27668,#27669,#27670,#27671,
#27672,#27673,#27674,#27675,#27676,#27677,#27678,#27679,#27680,#27681,#27682,
#27683,#27684,#27685,#27686,#27687,#27688,#27689,#27690,#27691,#27692,#27693,
#27694,#27695,#27696,#27697,#27698,#27699,#27700,#27701,#27702,#27703,#27704,
#27705,#27706,#27707,#27708,#27709,#27710),.UNSPECIFIED.,.F.,.F.)
B_SPLINE_CURVE_WITH_KNOTS((3,2,2,2,2,2,2,2,2,2,2,2,2,2,2,2,2,2,2,2,2,2,
2,3),(0.214924305846367,0.222222222222222,0.25,0.277777777777778,0.305555555555555,
0.333333333333334,0.361111111111111,0.388888888888889,0.416666666666667,
0.444444444444444,0.472222222222222,0.5,0.527777777777778,0.555555555555556,
0.583333333333333,0.611111111111111,0.638888888888889,0.666666666666667,
0.694444444444444,0.722222222222222,0.75,0.777777777777778,0.805555555555556,
0.833333333333333),.UNSPECIFIED.)
CURVE()
GEOMETRIC_REPRESENTATION_ITEM()
RATIONAL_B_SPLINE_CURVE((0.98679962630025,0.991047863068525,1.,0.965925826289068,
1.,0.965925826289068,1.,0.965925826289068,1.,0.965925826289068,1.,0.965925826289068,
1.,0.965925826289068,1.,0.965925826289068,1.,0.965925826289068,1.,0.965925826289068,
1.,0.965925826289068,1.,0.965925826289068,1.,0.965925826289068,1.,0.965925826289068,
1.,0.965925826289068,1.,0.965925826289068,1.,0.965925826289068,1.,0.965925826289068,
1.,0.965925826289068,1.,0.965925826289068,1.,0.965925826289068,1.,0.965925826289068,
1.,0.965925826289068,1.))
REPRESENTATION_ITEM('')
);
#1858=(
BOUNDED_CURVE()
B_SPLINE_CURVE(2,(#27723,#27724,#27725,#27726,#27727,#27728,#27729,#27730,
#27731,#27732,#27733,#27734,#27735,#27736,#27737,#27738,#27739,#27740,#27741,
#27742,#27743,#27744,#27745,#27746,#27747,#27748,#27749,#27750,#27751,#27752,
#27753,#27754,#27755,#27756,#27757,#27758,#27759,#27760,#27761,#27762,#27763,
#27764,#27765,#27766,#27767,#27768,#27769,#27770,#27771),.UNSPECIFIED.,
 .F.,.F.)
B_SPLINE_CURVE_WITH_KNOTS((3,2,2,2,2,2,2,2,2,2,2,2,2,2,2,2,2,2,2,2,2,2,
2,2,3),(0.178312023944365,0.194444444444445,0.222222222222222,0.25,0.277777777777778,
0.305555555555555,0.333333333333334,0.361111111111111,0.388888888888889,
0.416666666666667,0.444444444444444,0.472222222222222,0.5,0.527777777777778,
0.555555555555556,0.583333333333334,0.611111111111111,0.638888888888889,
0.666666666666667,0.694444444444444,0.722222222222222,0.75,0.777777777777778,
0.805555555555556,0.833333333333333),.UNSPECIFIED.)
CURVE()
GEOMETRIC_REPRESENTATION_ITEM()
RATIONAL_B_SPLINE_CURVE((0.983407467343328,0.980210839654089,1.,0.965925826289068,
1.,0.965925826289068,1.,0.965925826289068,1.,0.965925826289068,1.,0.965925826289068,
1.,0.965925826289068,1.,0.965925826289068,1.,0.965925826289068,1.,0.965925826289068,
1.,0.965925826289068,1.,0.965925826289068,1.,0.965925826289068,1.,0.965925826289068,
1.,0.965925826289068,1.,0.965925826289068,1.,0.965925826289068,1.,0.965925826289068,
1.,0.965925826289068,1.,0.965925826289068,1.,0.965925826289068,1.,0.965925826289068,
1.,0.965925826289068,1.,0.965925826289068,1.))
REPRESENTATION_ITEM('')
);
#1859=(
BOUNDED_CURVE()
B_SPLINE_CURVE(2,(#27988,#27989,#27990,#27991,#27992,#27993,#27994,#27995,
#27996,#27997,#27998,#27999,#28000,#28001,#28002,#28003,#28004,#28005,#28006,
#28007,#28008,#28009,#28010,#28011,#28012,#28013,#28014,#28015,#28016,#28017,
#28018,#28019,#28020,#28021,#28022,#28023,#28024,#28025,#28026,#28027,#28028,
#28029,#28030,#28031,#28032,#28033,#28034,#28035,#28036,#28037,#28038,#28039,
#28040),.UNSPECIFIED.,.F.,.F.)
B_SPLINE_CURVE_WITH_KNOTS((3,2,2,2,2,2,2,2,2,2,2,2,2,2,2,2,2,2,2,2,2,2,
2,2,2,2,3),(0.121758697158625,0.138888888888889,0.166666666666667,0.194444444444445,
0.222222222222222,0.25,0.277777777777778,0.305555555555555,0.333333333333334,
0.361111111111111,0.388888888888889,0.416666666666667,0.444444444444444,
0.472222222222222,0.5,0.527777777777778,0.555555555555556,0.583333333333333,
0.611111111111111,0.638888888888889,0.666666666666667,0.694444444444444,
0.722222222222222,0.75,0.777777777777778,0.805555555555556,0.833333333333334),
 .UNSPECIFIED.)
CURVE()
GEOMETRIC_REPRESENTATION_ITEM()
RATIONAL_B_SPLINE_CURVE((0.983890809673563,0.978986903366131,1.,0.965925826289068,
1.,0.965925826289068,1.,0.965925826289068,1.,0.965925826289068,1.,0.965925826289068,
1.,0.965925826289068,1.,0.965925826289068,1.,0.965925826289068,1.,0.965925826289068,
1.,0.965925826289068,1.,0.965925826289068,1.,0.965925826289068,1.,0.965925826289068,
1.,0.965925826289068,1.,0.965925826289068,1.,0.965925826289068,1.,0.965925826289068,
1.,0.965925826289068,1.,0.965925826289068,1.,0.965925826289068,1.,0.965925826289068,
1.,0.965925826289068,1.,0.965925826289068,1.,0.965925826289068,1.,0.965925826289068,
1.))
REPRESENTATION_ITEM('')
);
#1860=(
BOUNDED_CURVE()
B_SPLINE_CURVE(2,(#28168,#28169,#28170,#28171,#28172,#28173,#28174,#28175,
#28176,#28177,#28178,#28179,#28180,#28181,#28182,#28183,#28184,#28185,#28186,
#28187,#28188,#28189,#28190,#28191,#28192,#28193,#28194,#28195,#28196,#28197,
#28198,#28199,#28200,#28201,#28202,#28203,#28204,#28205,#28206,#28207,#28208,
#28209,#28210,#28211,#28212,#28213,#28214,#28215,#28216,#28217,#28218,#28219,
#28220,#28221,#28222,#28223,#28224),.UNSPECIFIED.,.F.,.F.)
B_SPLINE_CURVE_WITH_KNOTS((3,2,2,2,2,2,2,2,2,2,2,2,2,2,2,2,2,2,2,2,2,2,
2,2,2,2,2,2,3),(0.0566003037608321,0.0833333333333333,0.111111111111111,
0.138888888888889,0.166666666666667,0.194444444444445,0.222222222222222,
0.25,0.277777777777778,0.305555555555555,0.333333333333334,0.361111111111111,
0.388888888888889,0.416666666666667,0.444444444444444,0.472222222222222,
0.5,0.527777777777778,0.555555555555556,0.583333333333333,0.611111111111111,
0.638888888888889,0.666666666666667,0.694444444444444,0.722222222222222,
0.75,0.777777777777778,0.805555555555556,0.833333333333333),
 .UNSPECIFIED.)
CURVE()
GEOMETRIC_REPRESENTATION_ITEM()
RATIONAL_B_SPLINE_CURVE((0.997533278365187,0.967207387834976,1.,0.965925826289068,
1.,0.965925826289068,1.,0.965925826289068,1.,0.965925826289068,1.,0.965925826289068,
1.,0.965925826289068,1.,0.965925826289068,1.,0.965925826289068,1.,0.965925826289068,
1.,0.965925826289068,1.,0.965925826289068,1.,0.965925826289068,1.,0.965925826289068,
1.,0.965925826289068,1.,0.965925826289068,1.,0.965925826289068,1.,0.965925826289068,
1.,0.965925826289068,1.,0.965925826289068,1.,0.965925826289068,1.,0.965925826289068,
1.,0.965925826289068,1.,0.965925826289068,1.,0.965925826289068,1.,0.965925826289068,
1.,0.965925826289068,1.,0.965925826289068,1.))
REPRESENTATION_ITEM('')
);
#1861=(
BOUNDED_CURVE()
B_SPLINE_CURVE(2,(#28478,#28479,#28480,#28481,#28482,#28483,#28484,#28485,
#28486,#28487,#28488,#28489,#28490),.UNSPECIFIED.,.F.,.F.)
B_SPLINE_CURVE_WITH_KNOTS((3,2,2,2,2,2,3),(0.,0.0277777777777779,0.0555555555555558,
0.0833333333333336,0.111111111111111,0.138888888888889,0.166666666666668),
 .UNSPECIFIED.)
CURVE()
GEOMETRIC_REPRESENTATION_ITEM()
RATIONAL_B_SPLINE_CURVE((1.,0.965925826289068,1.,0.965925826289068,1.,0.965925826289068,
1.,0.965925826289068,1.,0.965925826289068,1.,0.965925826289068,1.))
REPRESENTATION_ITEM('')
);
#1862=(
BOUNDED_CURVE()
B_SPLINE_CURVE(2,(#28500,#28501,#28502,#28503,#28504,#28505,#28506,#28507,
#28508,#28509,#28510,#28511,#28512),.UNSPECIFIED.,.F.,.F.)
B_SPLINE_CURVE_WITH_KNOTS((3,2,2,2,2,2,3),(0.666666666666666,0.694444444444444,
0.722222222222222,0.75,0.777777777777778,0.805555555555556,0.833333333333333),
 .UNSPECIFIED.)
CURVE()
GEOMETRIC_REPRESENTATION_ITEM()
RATIONAL_B_SPLINE_CURVE((1.,0.965925826289068,1.,0.965925826289068,1.,0.965925826289068,
1.,0.965925826289068,1.,0.965925826289068,1.,0.965925826289068,1.))
REPRESENTATION_ITEM('')
);
#1863=(
BOUNDED_CURVE()
B_SPLINE_CURVE(2,(#28514,#28515,#28516,#28517,#28518,#28519,#28520,#28521,
#28522,#28523,#28524,#28525,#28526),.UNSPECIFIED.,.F.,.F.)
B_SPLINE_CURVE_WITH_KNOTS((3,2,2,2,2,2,3),(0.5,0.527777777777778,0.555555555555556,
0.583333333333333,0.611111111111111,0.638888888888889,0.666666666666666),
 .UNSPECIFIED.)
CURVE()
GEOMETRIC_REPRESENTATION_ITEM()
RATIONAL_B_SPLINE_CURVE((1.,0.965925826289069,1.,0.965925826289068,1.,0.965925826289068,
1.,0.965925826289068,1.,0.965925826289068,1.,0.965925826289069,1.))
REPRESENTATION_ITEM('')
);
#1864=(
BOUNDED_CURVE()
B_SPLINE_CURVE(2,(#28528,#28529,#28530,#28531,#28532,#28533,#28534,#28535,
#28536,#28537,#28538,#28539,#28540),.UNSPECIFIED.,.F.,.F.)
B_SPLINE_CURVE_WITH_KNOTS((3,2,2,2,2,2,3),(0.333333333333333,0.361111111111111,
0.388888888888889,0.416666666666667,0.444444444444444,0.472222222222222,
0.5),.UNSPECIFIED.)
CURVE()
GEOMETRIC_REPRESENTATION_ITEM()
RATIONAL_B_SPLINE_CURVE((1.,0.965925826289068,1.,0.965925826289068,1.,0.965925826289068,
1.,0.965925826289068,1.,0.965925826289068,1.,0.965925826289068,1.))
REPRESENTATION_ITEM('')
);
#1865=(
BOUNDED_CURVE()
B_SPLINE_CURVE(2,(#28542,#28543,#28544,#28545,#28546,#28547,#28548,#28549,
#28550,#28551,#28552,#28553,#28554),.UNSPECIFIED.,.F.,.F.)
B_SPLINE_CURVE_WITH_KNOTS((3,2,2,2,2,2,3),(0.166666666666668,0.194444444444445,
0.222222222222222,0.25,0.277777777777778,0.305555555555555,0.333333333333333),
 .UNSPECIFIED.)
CURVE()
GEOMETRIC_REPRESENTATION_ITEM()
RATIONAL_B_SPLINE_CURVE((1.,0.965925826289069,1.,0.965925826289068,1.,0.965925826289068,
1.,0.965925826289068,1.,0.965925826289068,1.,0.965925826289069,1.))
REPRESENTATION_ITEM('')
);
#1866=(
BOUNDED_CURVE()
B_SPLINE_CURVE(2,(#31140,#31141,#31142,#31143,#31144,#31145,#31146,#31147,
#31148,#31149,#31150),.UNSPECIFIED.,.F.,.F.)
B_SPLINE_CURVE_WITH_KNOTS((3,2,2,2,2,3),(0.,0.05,0.1,0.15,0.2,0.25),
 .UNSPECIFIED.)
CURVE()
GEOMETRIC_REPRESENTATION_ITEM()
RATIONAL_B_SPLINE_CURVE((1.,0.951056516295154,1.,0.951056516295154,1.,0.951056516295154,
1.,0.951056516295154,1.,0.951056516295154,1.))
REPRESENTATION_ITEM('')
);
#1867=(
BOUNDED_CURVE()
B_SPLINE_CURVE(2,(#31152,#31153,#31154,#31155,#31156,#31157,#31158,#31159,
#31160,#31161,#31162),.UNSPECIFIED.,.F.,.F.)
B_SPLINE_CURVE_WITH_KNOTS((3,2,2,2,2,3),(0.25,0.3,0.35,0.4,0.45,0.5),
 .UNSPECIFIED.)
CURVE()
GEOMETRIC_REPRESENTATION_ITEM()
RATIONAL_B_SPLINE_CURVE((1.,0.951056516295153,1.,0.951056516295154,1.,0.951056516295154,
1.,0.951056516295154,1.,0.951056516295154,1.))
REPRESENTATION_ITEM('')
);
#1868=(
BOUNDED_CURVE()
B_SPLINE_CURVE(2,(#31164,#31165,#31166,#31167,#31168,#31169,#31170,#31171,
#31172,#31173,#31174),.UNSPECIFIED.,.F.,.F.)
B_SPLINE_CURVE_WITH_KNOTS((3,2,2,2,2,3),(0.5,0.55,0.6,0.65,0.7,0.75),
 .UNSPECIFIED.)
CURVE()
GEOMETRIC_REPRESENTATION_ITEM()
RATIONAL_B_SPLINE_CURVE((1.,0.951056516295153,1.,0.951056516295154,1.,0.951056516295154,
1.,0.951056516295154,1.,0.951056516295154,1.))
REPRESENTATION_ITEM('')
);
#1869=(
BOUNDED_CURVE()
B_SPLINE_CURVE(2,(#31176,#31177,#31178,#31179,#31180),.UNSPECIFIED.,.F.,
 .F.)
B_SPLINE_CURVE_WITH_KNOTS((3,2,3),(0.75,0.8,0.826757087433802),
 .UNSPECIFIED.)
CURVE()
GEOMETRIC_REPRESENTATION_ITEM()
RATIONAL_B_SPLINE_CURVE((1.,0.951056516295153,1.,0.973808298543891,0.975649142923828))
REPRESENTATION_ITEM('')
);
#1870=(
BOUNDED_CURVE()
B_SPLINE_CURVE(2,(#31184,#31185,#31186,#31187,#31188,#31189,#31190,#31191,
#31192,#31193,#31194,#31195,#31196,#31197,#31198,#31199,#31200,#31201,#31202,
#31203,#31204,#31205,#31206,#31207,#31208,#31209,#31210,#31211,#31212,#31213,
#31214,#31215,#31216,#31217,#31218),.UNSPECIFIED.,.F.,.F.)
B_SPLINE_CURVE_WITH_KNOTS((3,2,2,2,2,2,2,2,2,2,2,2,2,2,2,2,2,3),(0.,0.05,
0.1,0.15,0.2,0.25,0.3,0.35,0.4,0.45,0.5,0.55,0.6,0.65,0.7,0.75,0.8,0.826757087433802),
 .UNSPECIFIED.)
CURVE()
GEOMETRIC_REPRESENTATION_ITEM()
RATIONAL_B_SPLINE_CURVE((1.,0.951056516295154,1.,0.951056516295154,1.,0.951056516295154,
1.,0.951056516295154,1.,0.951056516295154,1.,0.951056516295154,1.,0.951056516295154,
1.,0.951056516295154,1.,0.951056516295154,1.,0.951056516295154,1.,0.951056516295154,
1.,0.951056516295154,1.,0.951056516295154,1.,0.951056516295154,1.,0.951056516295154,
1.,0.951056516295154,1.,0.973808298543891,0.975649142923828))
REPRESENTATION_ITEM('')
);
#1871=(
BOUNDED_CURVE()
B_SPLINE_CURVE(2,(#31454,#31455,#31456,#31457,#31458,#31459,#31460,#31461,
#31462,#31463,#31464,#31465,#31466,#31467,#31468,#31469,#31470,#31471,#31472,
#31473,#31474,#31475,#31476,#31477,#31478,#31479,#31480,#31481,#31482,#31483,
#31484,#31485,#31486,#31487,#31488),.UNSPECIFIED.,.F.,.F.)
B_SPLINE_CURVE_WITH_KNOTS((3,2,2,2,2,2,2,2,2,2,2,2,2,2,2,2,2,3),(0.,0.05,
0.1,0.15,0.2,0.25,0.3,0.35,0.4,0.45,0.5,0.55,0.6,0.65,0.7,0.75,0.8,0.826757073484189),
 .UNSPECIFIED.)
CURVE()
GEOMETRIC_REPRESENTATION_ITEM()
RATIONAL_B_SPLINE_CURVE((1.,0.951056516295154,1.,0.951056516295154,1.,0.951056516295154,
1.,0.951056516295154,1.,0.951056516295154,1.,0.951056516295154,1.,0.951056516295154,
1.,0.951056516295154,1.,0.951056516295154,1.,0.951056516295154,1.,0.951056516295154,
1.,0.951056516295154,1.,0.951056516295154,1.,0.951056516295154,1.,0.951056516295154,
1.,0.951056516295154,1.,0.973808312198744,0.975649141004414))
REPRESENTATION_ITEM('')
);
#1872=(
BOUNDED_CURVE()
B_SPLINE_CURVE(2,(#31492,#31493,#31494,#31495,#31496),.UNSPECIFIED.,.F.,
 .F.)
B_SPLINE_CURVE_WITH_KNOTS((3,2,3),(0.75,0.8,0.826757130829527),
 .UNSPECIFIED.)
CURVE()
GEOMETRIC_REPRESENTATION_ITEM()
RATIONAL_B_SPLINE_CURVE((1.,0.951056516295153,1.,0.973808256065132,0.975649148895013))
REPRESENTATION_ITEM('')
);
#1873=(
BOUNDED_CURVE()
B_SPLINE_CURVE(2,(#31498,#31499,#31500,#31501,#31502,#31503,#31504,#31505,
#31506,#31507,#31508),.UNSPECIFIED.,.F.,.F.)
B_SPLINE_CURVE_WITH_KNOTS((3,2,2,2,2,3),(0.5,0.55,0.6,0.65,0.7,0.75),
 .UNSPECIFIED.)
CURVE()
GEOMETRIC_REPRESENTATION_ITEM()
RATIONAL_B_SPLINE_CURVE((1.,0.951056516295153,1.,0.951056516295154,1.,0.951056516295154,
1.,0.951056516295154,1.,0.951056516295154,1.))
REPRESENTATION_ITEM('')
);
#1874=(
BOUNDED_CURVE()
B_SPLINE_CURVE(2,(#31510,#31511,#31512,#31513,#31514,#31515,#31516,#31517,
#31518,#31519,#31520),.UNSPECIFIED.,.F.,.F.)
B_SPLINE_CURVE_WITH_KNOTS((3,2,2,2,2,3),(0.25,0.3,0.35,0.4,0.45,0.5),
 .UNSPECIFIED.)
CURVE()
GEOMETRIC_REPRESENTATION_ITEM()
RATIONAL_B_SPLINE_CURVE((1.,0.951056516295153,1.,0.951056516295154,1.,0.951056516295154,
1.,0.951056516295154,1.,0.951056516295154,1.))
REPRESENTATION_ITEM('')
);
#1875=(
BOUNDED_CURVE()
B_SPLINE_CURVE(2,(#31522,#31523,#31524,#31525,#31526,#31527,#31528,#31529,
#31530,#31531,#31532),.UNSPECIFIED.,.F.,.F.)
B_SPLINE_CURVE_WITH_KNOTS((3,2,2,2,2,3),(0.,0.05,0.1,0.15,0.2,0.25),
 .UNSPECIFIED.)
CURVE()
GEOMETRIC_REPRESENTATION_ITEM()
RATIONAL_B_SPLINE_CURVE((1.,0.951056516295154,1.,0.951056516295154,1.,0.951056516295154,
1.,0.951056516295154,1.,0.951056516295154,1.))
REPRESENTATION_ITEM('')
);
#1876=(
BOUNDED_CURVE()
B_SPLINE_CURVE(2,(#31969,#31970,#31971,#31972,#31973,#31974,#31975,#31976,
#31977,#31978,#31979,#31980,#31981,#31982,#31983,#31984,#31985,#31986,#31987,
#31988,#31989,#31990,#31991,#31992,#31993,#31994,#31995,#31996,#31997,#31998,
#31999,#32000,#32001,#32002,#32003,#32004,#32005,#32006,#32007,#32008,#32009,
#32010,#32011,#32012,#32013,#32014,#32015,#32016,#32017,#32018,#32019,#32020,
#32021,#32022,#32023,#32024,#32025,#32026,#32027,#32028,#32029),
 .UNSPECIFIED.,.F.,.F.)
B_SPLINE_CURVE_WITH_KNOTS((3,2,2,2,2,2,2,2,2,2,2,2,2,2,2,2,2,2,2,2,2,2,
2,2,2,2,2,2,2,2,3),(0.,0.0277777777777778,0.0555555555555556,0.0833333333333333,
0.111111111111111,0.138888888888889,0.166666666666667,0.194444444444445,
0.222222222222222,0.25,0.277777777777778,0.305555555555555,0.333333333333334,
0.361111111111111,0.388888888888889,0.416666666666667,0.444444444444444,
0.472222222222222,0.5,0.527777777777778,0.555555555555556,0.583333333333333,
0.611111111111111,0.638888888888889,0.666666666666667,0.694444444444444,
0.722222222222222,0.75,0.777777777777778,0.805555555555556,0.833333333333333),
 .UNSPECIFIED.)
CURVE()
GEOMETRIC_REPRESENTATION_ITEM()
RATIONAL_B_SPLINE_CURVE((1.,0.965925826289068,1.,0.965925826289068,1.,0.965925826289068,
1.,0.965925826289068,1.,0.965925826289068,1.,0.965925826289068,1.,0.965925826289068,
1.,0.965925826289068,1.,0.965925826289068,1.,0.965925826289068,1.,0.965925826289068,
1.,0.965925826289068,1.,0.965925826289068,1.,0.965925826289068,1.,0.965925826289068,
1.,0.965925826289068,1.,0.965925826289068,1.,0.965925826289068,1.,0.965925826289068,
1.,0.965925826289068,1.,0.965925826289068,1.,0.965925826289068,1.,0.965925826289068,
1.,0.965925826289068,1.,0.965925826289068,1.,0.965925826289068,1.,0.965925826289068,
1.,0.965925826289068,1.,0.965925826289068,1.,0.965925826289068,1.))
REPRESENTATION_ITEM('')
);
#1877=(
BOUNDED_CURVE()
B_SPLINE_CURVE(2,(#32033,#32034,#32035,#32036,#32037,#32038,#32039,#32040,
#32041,#32042,#32043,#32044,#32045),.UNSPECIFIED.,.F.,.F.)
B_SPLINE_CURVE_WITH_KNOTS((3,2,2,2,2,2,3),(0.666666666666666,0.694444444444444,
0.722222222222222,0.75,0.777777777777778,0.805555555555556,0.833333333333333),
 .UNSPECIFIED.)
CURVE()
GEOMETRIC_REPRESENTATION_ITEM()
RATIONAL_B_SPLINE_CURVE((1.,0.965925826289068,1.,0.965925826289068,1.,0.965925826289068,
1.,0.965925826289068,1.,0.965925826289068,1.,0.965925826289068,1.))
REPRESENTATION_ITEM('')
);
#1878=(
BOUNDED_CURVE()
B_SPLINE_CURVE(2,(#32047,#32048,#32049,#32050,#32051,#32052,#32053,#32054,
#32055,#32056,#32057,#32058,#32059),.UNSPECIFIED.,.F.,.F.)
B_SPLINE_CURVE_WITH_KNOTS((3,2,2,2,2,2,3),(0.5,0.527777777777778,0.555555555555556,
0.583333333333333,0.611111111111111,0.638888888888889,0.666666666666666),
 .UNSPECIFIED.)
CURVE()
GEOMETRIC_REPRESENTATION_ITEM()
RATIONAL_B_SPLINE_CURVE((1.,0.965925826289069,1.,0.965925826289068,1.,0.965925826289068,
1.,0.965925826289068,1.,0.965925826289068,1.,0.965925826289069,1.))
REPRESENTATION_ITEM('')
);
#1879=(
BOUNDED_CURVE()
B_SPLINE_CURVE(2,(#32061,#32062,#32063,#32064,#32065,#32066,#32067,#32068,
#32069,#32070,#32071,#32072,#32073),.UNSPECIFIED.,.F.,.F.)
B_SPLINE_CURVE_WITH_KNOTS((3,2,2,2,2,2,3),(0.333333333333333,0.361111111111111,
0.388888888888889,0.416666666666667,0.444444444444444,0.472222222222222,
0.5),.UNSPECIFIED.)
CURVE()
GEOMETRIC_REPRESENTATION_ITEM()
RATIONAL_B_SPLINE_CURVE((1.,0.965925826289068,1.,0.965925826289068,1.,0.965925826289068,
1.,0.965925826289068,1.,0.965925826289068,1.,0.965925826289068,1.))
REPRESENTATION_ITEM('')
);
#1880=(
BOUNDED_CURVE()
B_SPLINE_CURVE(2,(#32075,#32076,#32077,#32078,#32079,#32080,#32081,#32082,
#32083,#32084,#32085,#32086,#32087),.UNSPECIFIED.,.F.,.F.)
B_SPLINE_CURVE_WITH_KNOTS((3,2,2,2,2,2,3),(0.166666666666668,0.194444444444445,
0.222222222222222,0.25,0.277777777777778,0.305555555555555,0.333333333333333),
 .UNSPECIFIED.)
CURVE()
GEOMETRIC_REPRESENTATION_ITEM()
RATIONAL_B_SPLINE_CURVE((1.,0.965925826289069,1.,0.965925826289068,1.,0.965925826289068,
1.,0.965925826289068,1.,0.965925826289068,1.,0.965925826289069,1.))
REPRESENTATION_ITEM('')
);
#1881=(
BOUNDED_CURVE()
B_SPLINE_CURVE(2,(#32089,#32090,#32091,#32092,#32093,#32094,#32095,#32096,
#32097,#32098,#32099,#32100,#32101),.UNSPECIFIED.,.F.,.F.)
B_SPLINE_CURVE_WITH_KNOTS((3,2,2,2,2,2,3),(0.,0.0277777777777779,0.0555555555555558,
0.0833333333333336,0.111111111111111,0.138888888888889,0.166666666666668),
 .UNSPECIFIED.)
CURVE()
GEOMETRIC_REPRESENTATION_ITEM()
RATIONAL_B_SPLINE_CURVE((1.,0.965925826289068,1.,0.965925826289068,1.,0.965925826289068,
1.,0.965925826289068,1.,0.965925826289068,1.,0.965925826289068,1.))
REPRESENTATION_ITEM('')
);
#1882=(
BOUNDED_CURVE()
B_SPLINE_CURVE(2,(#32224,#32225,#32226,#32227,#32228,#32229,#32230,#32231,
#32232,#32233,#32234,#32235,#32236,#32237,#32238,#32239,#32240,#32241,#32242,
#32243,#32244,#32245,#32246,#32247,#32248,#32249,#32250,#32251,#32252,#32253,
#32254,#32255,#32256,#32257,#32258,#32259,#32260,#32261,#32262,#32263,#32264,
#32265,#32266,#32267,#32268,#32269,#32270,#32271,#32272,#32273,#32274,#32275,
#32276,#32277,#32278,#32279,#32280,#32281,#32282),.UNSPECIFIED.,.F.,.F.)
B_SPLINE_CURVE_WITH_KNOTS((3,2,2,2,2,2,2,2,2,2,2,2,2,2,2,2,2,2,2,2,2,2,
2,2,2,2,2,2,2,3),(0.,0.0277777777777778,0.0555555555555556,0.0833333333333333,
0.111111111111111,0.138888888888889,0.166666666666667,0.194444444444445,
0.222222222222222,0.25,0.277777777777778,0.305555555555555,0.333333333333334,
0.361111111111111,0.388888888888889,0.416666666666667,0.444444444444444,
0.472222222222222,0.5,0.527777777777778,0.555555555555556,0.583333333333333,
0.611111111111111,0.638888888888889,0.666666666666667,0.694444444444444,
0.722222222222222,0.75,0.777777777777778,0.791679968730667),
 .UNSPECIFIED.)
CURVE()
GEOMETRIC_REPRESENTATION_ITEM()
RATIONAL_B_SPLINE_CURVE((1.,0.965925826289068,1.,0.965925826289068,1.,0.965925826289068,
1.,0.965925826289068,1.,0.965925826289068,1.,0.965925826289068,1.,0.965925826289068,
1.,0.965925826289068,1.,0.965925826289068,1.,0.965925826289068,1.,0.965925826289068,
1.,0.965925826289068,1.,0.965925826289068,1.,0.965925826289068,1.,0.965925826289068,
1.,0.965925826289068,1.,0.965925826289068,1.,0.965925826289068,1.,0.965925826289068,
1.,0.965925826289068,1.,0.965925826289068,1.,0.965925826289068,1.,0.965925826289068,
1.,0.965925826289068,1.,0.965925826289068,1.,0.965925826289068,1.,0.965925826289068,
1.,0.965925826289068,1.,0.982946595898313,0.982962928772354))
REPRESENTATION_ITEM('')
);
#1883=(
BOUNDED_CURVE()
B_SPLINE_CURVE(2,(#32528,#32529,#32530,#32531,#32532,#32533,#32534,#32535,
#32536,#32537,#32538,#32539,#32540,#32541,#32542,#32543,#32544,#32545,#32546,
#32547,#32548,#32549,#32550,#32551,#32552,#32553,#32554,#32555,#32556,#32557,
#32558,#32559,#32560,#32561,#32562,#32563,#32564,#32565,#32566,#32567,#32568,
#32569,#32570,#32571,#32572,#32573,#32574,#32575,#32576,#32577,#32578,#32579,
#32580,#32581,#32582),.UNSPECIFIED.,.F.,.F.)
B_SPLINE_CURVE_WITH_KNOTS((3,2,2,2,2,2,2,2,2,2,2,2,2,2,2,2,2,2,2,2,2,2,
2,2,2,2,2,3),(0.,0.0277777777777778,0.0555555555555556,0.0833333333333333,
0.111111111111111,0.138888888888889,0.166666666666667,0.194444444444445,
0.222222222222222,0.25,0.277777777777778,0.305555555555555,0.333333333333334,
0.361111111111111,0.388888888888889,0.416666666666667,0.444444444444444,
0.472222222222222,0.5,0.527777777777778,0.555555555555556,0.583333333333333,
0.611111111111111,0.638888888888889,0.666666666666667,0.694444444444444,
0.722222222222222,0.735128599370391),.UNSPECIFIED.)
CURVE()
GEOMETRIC_REPRESENTATION_ITEM()
RATIONAL_B_SPLINE_CURVE((1.,0.965925826289068,1.,0.965925826289068,1.,0.965925826289068,
1.,0.965925826289068,1.,0.965925826289068,1.,0.965925826289068,1.,0.965925826289068,
1.,0.965925826289068,1.,0.965925826289068,1.,0.965925826289068,1.,0.965925826289068,
1.,0.965925826289068,1.,0.965925826289068,1.,0.965925826289068,1.,0.965925826289068,
1.,0.965925826289068,1.,0.965925826289068,1.,0.965925826289068,1.,0.965925826289068,
1.,0.965925826289068,1.,0.965925826289068,1.,0.965925826289068,1.,0.965925826289068,
1.,0.965925826289068,1.,0.965925826289068,1.,0.965925826289068,1.,0.984168131070682,
0.983048171279439))
REPRESENTATION_ITEM('')
);
#1884=(
BOUNDED_CURVE()
B_SPLINE_CURVE(2,(#32592,#32593,#32594,#32595,#32596,#32597,#32598,#32599,
#32600,#32601,#32602,#32603,#32604,#32605,#32606,#32607,#32608,#32609,#32610,
#32611,#32612,#32613,#32614,#32615,#32616,#32617,#32618,#32619,#32620,#32621,
#32622,#32623,#32624,#32625,#32626,#32627,#32628,#32629,#32630,#32631,#32632,
#32633,#32634,#32635,#32636,#32637,#32638,#32639,#32640,#32641,#32642,#32643,
#32644),.UNSPECIFIED.,.F.,.F.)
B_SPLINE_CURVE_WITH_KNOTS((3,2,2,2,2,2,2,2,2,2,2,2,2,2,2,2,2,2,2,2,2,2,
2,2,2,2,3),(0.,0.0277777777777778,0.0555555555555556,0.0833333333333333,
0.111111111111111,0.138888888888889,0.166666666666667,0.194444444444445,
0.222222222222222,0.25,0.277777777777778,0.305555555555555,0.333333333333334,
0.361111111111111,0.388888888888889,0.416666666666667,0.444444444444444,
0.472222222222222,0.5,0.527777777777778,0.555555555555556,0.583333333333333,
0.611111111111111,0.638888888888889,0.666666666666667,0.694444444444444,
0.698457242498421),.UNSPECIFIED.)
CURVE()
GEOMETRIC_REPRESENTATION_ITEM()
RATIONAL_B_SPLINE_CURVE((1.,0.965925826289068,1.,0.965925826289068,1.,0.965925826289068,
1.,0.965925826289068,1.,0.965925826289068,1.,0.965925826289068,1.,0.965925826289068,
1.,0.965925826289068,1.,0.965925826289068,1.,0.965925826289068,1.,0.965925826289068,
1.,0.965925826289068,1.,0.965925826289068,1.,0.965925826289068,1.,0.965925826289068,
1.,0.965925826289068,1.,0.965925826289068,1.,0.965925826289068,1.,0.965925826289068,
1.,0.965925826289068,1.,0.965925826289068,1.,0.965925826289068,1.,0.965925826289068,
1.,0.965925826289068,1.,0.965925826289068,1.,0.995077619993509,0.991577421204609))
REPRESENTATION_ITEM('')
);
#1885=(
BOUNDED_CURVE()
B_SPLINE_CURVE(2,(#32663,#32664,#32665,#32666,#32667,#32668,#32669),
 .UNSPECIFIED.,.F.,.F.)
B_SPLINE_CURVE_WITH_KNOTS((3,2,2,3),(0.560471898984009,0.583333333333333,
0.611111111111111,0.633782023464906),.UNSPECIFIED.)
CURVE()
GEOMETRIC_REPRESENTATION_ITEM()
RATIONAL_B_SPLINE_CURVE((0.990073274378595,0.971956558529202,1.,0.965925826289068,
1.,0.972190266193773,0.989774519102187))
REPRESENTATION_ITEM('')
);
#1886=(
BOUNDED_CURVE()
B_SPLINE_CURVE(2,(#32884,#32885,#32886,#32887,#32888,#32889,#32890,#32891,
#32892,#32893,#32894,#32895,#32896,#32897,#32898,#32899,#32900,#32901,#32902,
#32903,#32904,#32905,#32906,#32907,#32908,#32909,#32910,#32911,#32912,#32913,
#32914,#32915,#32916,#32917,#32918,#32919,#32920,#32921,#32922,#32923,#32924,
#32925,#32926,#32927,#32928,#32929,#32930,#32931,#32932,#32933,#32934),
 .UNSPECIFIED.,.F.,.F.)
B_SPLINE_CURVE_WITH_KNOTS((3,2,2,2,2,2,2,2,2,2,2,2,2,2,2,2,2,2,2,2,2,2,
2,2,2,3),(0.,0.0277777777777778,0.0555555555555556,0.0833333333333333,0.111111111111111,
0.138888888888889,0.166666666666667,0.194444444444445,0.222222222222222,
0.25,0.277777777777778,0.305555555555555,0.333333333333334,0.361111111111111,
0.388888888888889,0.416666666666667,0.444444444444444,0.472222222222222,
0.5,0.527777777777778,0.555555555555556,0.583333333333333,0.611111111111111,
0.638888888888889,0.666666666666667,0.672203650950348),.UNSPECIFIED.)
CURVE()
GEOMETRIC_REPRESENTATION_ITEM()
RATIONAL_B_SPLINE_CURVE((1.,0.965925826289068,1.,0.965925826289068,1.,0.965925826289068,
1.,0.965925826289068,1.,0.965925826289068,1.,0.965925826289068,1.,0.965925826289068,
1.,0.965925826289068,1.,0.965925826289068,1.,0.965925826289068,1.,0.965925826289068,
1.,0.965925826289068,1.,0.965925826289068,1.,0.965925826289068,1.,0.965925826289068,
1.,0.965925826289068,1.,0.965925826289068,1.,0.965925826289068,1.,0.965925826289068,
1.,0.965925826289068,1.,0.965925826289068,1.,0.965925826289068,1.,0.965925826289068,
1.,0.965925826289068,1.,0.993207946084594,0.989123631865601))
REPRESENTATION_ITEM('')
);
#1887=(
BOUNDED_CURVE()
B_SPLINE_CURVE(2,(#33046,#33047,#33048,#33049,#33050,#33051,#33052,#33053,
#33054,#33055,#33056,#33057,#33058,#33059,#33060,#33061,#33062,#33063,#33064,
#33065,#33066,#33067,#33068,#33069,#33070,#33071,#33072,#33073,#33074,#33075,
#33076,#33077,#33078,#33079,#33080,#33081,#33082,#33083,#33084,#33085,#33086,
#33087,#33088,#33089,#33090,#33091,#33092,#33093,#33094),.UNSPECIFIED.,
 .F.,.F.)
B_SPLINE_CURVE_WITH_KNOTS((3,2,2,2,2,2,2,2,2,2,2,2,2,2,2,2,2,2,2,2,2,2,
2,2,3),(0.,0.0277777777777778,0.0555555555555556,0.0833333333333333,0.111111111111111,
0.138888888888889,0.166666666666667,0.194444444444445,0.222222222222222,
0.25,0.277777777777778,0.305555555555555,0.333333333333334,0.361111111111111,
0.388888888888889,0.416666666666667,0.444444444444444,0.472222222222222,
0.5,0.527777777777778,0.555555555555556,0.583333333333333,0.611111111111111,
0.638888888888889,0.660043255494719),.UNSPECIFIED.)
CURVE()
GEOMETRIC_REPRESENTATION_ITEM()
RATIONAL_B_SPLINE_CURVE((1.,0.965925826289068,1.,0.965925826289068,1.,0.965925826289068,
1.,0.965925826289068,1.,0.965925826289068,1.,0.965925826289068,1.,0.965925826289068,
1.,0.965925826289068,1.,0.965925826289068,1.,0.965925826289068,1.,0.965925826289068,
1.,0.965925826289068,1.,0.965925826289068,1.,0.965925826289068,1.,0.965925826289068,
1.,0.965925826289068,1.,0.965925826289068,1.,0.965925826289068,1.,0.965925826289068,
1.,0.965925826289068,1.,0.965925826289068,1.,0.965925826289068,1.,0.965925826289068,
1.,0.974050567751015,0.98762508931862))
REPRESENTATION_ITEM('')
);
#1888=(
BOUNDED_CURVE()
B_SPLINE_CURVE(2,(#33304,#33305,#33306,#33307,#33308,#33309,#33310,#33311,
#33312,#33313,#33314,#33315,#33316),.UNSPECIFIED.,.F.,.F.)
B_SPLINE_CURVE_WITH_KNOTS((3,2,2,2,2,2,3),(0.,0.0277777777777779,0.0555555555555558,
0.0833333333333336,0.111111111111111,0.138888888888889,0.166666666666668),
 .UNSPECIFIED.)
CURVE()
GEOMETRIC_REPRESENTATION_ITEM()
RATIONAL_B_SPLINE_CURVE((1.,0.965925826289068,1.,0.965925826289068,1.,0.965925826289068,
1.,0.965925826289068,1.,0.965925826289068,1.,0.965925826289068,1.))
REPRESENTATION_ITEM('')
);
#1889=(
BOUNDED_CURVE()
B_SPLINE_CURVE(2,(#33318,#33319,#33320,#33321,#33322,#33323,#33324,#33325,
#33326,#33327,#33328,#33329,#33330),.UNSPECIFIED.,.F.,.F.)
B_SPLINE_CURVE_WITH_KNOTS((3,2,2,2,2,2,3),(0.166666666666668,0.194444444444445,
0.222222222222222,0.25,0.277777777777778,0.305555555555555,0.333333333333333),
 .UNSPECIFIED.)
CURVE()
GEOMETRIC_REPRESENTATION_ITEM()
RATIONAL_B_SPLINE_CURVE((1.,0.965925826289069,1.,0.965925826289068,1.,0.965925826289068,
1.,0.965925826289068,1.,0.965925826289068,1.,0.965925826289069,1.))
REPRESENTATION_ITEM('')
);
#1890=(
BOUNDED_CURVE()
B_SPLINE_CURVE(2,(#33332,#33333,#33334,#33335,#33336,#33337,#33338,#33339,
#33340,#33341,#33342,#33343,#33344),.UNSPECIFIED.,.F.,.F.)
B_SPLINE_CURVE_WITH_KNOTS((3,2,2,2,2,2,3),(0.333333333333333,0.361111111111111,
0.388888888888889,0.416666666666667,0.444444444444444,0.472222222222222,
0.5),.UNSPECIFIED.)
CURVE()
GEOMETRIC_REPRESENTATION_ITEM()
RATIONAL_B_SPLINE_CURVE((1.,0.965925826289068,1.,0.965925826289068,1.,0.965925826289068,
1.,0.965925826289068,1.,0.965925826289068,1.,0.965925826289068,1.))
REPRESENTATION_ITEM('')
);
#1891=(
BOUNDED_CURVE()
B_SPLINE_CURVE(2,(#33346,#33347,#33348,#33349,#33350,#33351,#33352),
 .UNSPECIFIED.,.F.,.F.)
B_SPLINE_CURVE_WITH_KNOTS((3,2,2,3),(0.5,0.527777777777778,0.555555555555556,
0.56047189898401),.UNSPECIFIED.)
CURVE()
GEOMETRIC_REPRESENTATION_ITEM()
RATIONAL_B_SPLINE_CURVE((1.,0.965925826289069,1.,0.965925826289068,1.,0.993969267759865,
0.990073274378594))
REPRESENTATION_ITEM('')
);
#1892=(
BOUNDED_CURVE()
B_SPLINE_CURVE(2,(#33398,#33399,#33400,#33401,#33402),.UNSPECIFIED.,.F.,
 .F.)
B_SPLINE_CURVE_WITH_KNOTS((3,2,3),(0.796543286201692,0.805555555555556,
0.833333333333333),.UNSPECIFIED.)
CURVE()
GEOMETRIC_REPRESENTATION_ITEM()
RATIONAL_B_SPLINE_CURVE((0.985063294131948,0.988944917266243,1.,0.965925826289068,
1.))
REPRESENTATION_ITEM('')
);
#1893=(
BOUNDED_CURVE()
B_SPLINE_CURVE(2,(#33413,#33414,#33415,#33416,#33417,#33418,#33419),
 .UNSPECIFIED.,.F.,.F.)
B_SPLINE_CURVE_WITH_KNOTS((3,2,2,3),(0.77026876316387,0.777777777777778,
0.805555555555556,0.833333333333333),.UNSPECIFIED.)
CURVE()
GEOMETRIC_REPRESENTATION_ITEM()
RATIONAL_B_SPLINE_CURVE((0.986557794578313,0.99078891513932,1.,0.965925826289068,
1.,0.965925826289068,1.))
REPRESENTATION_ITEM('')
);
#1894=(
BOUNDED_CURVE()
B_SPLINE_CURVE(2,(#33689,#33690,#33691,#33692,#33693,#33694,#33695,#33696,
#33697),.UNSPECIFIED.,.F.,.F.)
B_SPLINE_CURVE_WITH_KNOTS((3,2,2,2,3),(0.6875,0.71875,0.75,0.78125,0.812500000739054),
 .UNSPECIFIED.)
CURVE()
GEOMETRIC_REPRESENTATION_ITEM()
RATIONAL_B_SPLINE_CURVE((1.,0.923879532511287,1.,0.923879532511287,1.,0.923879532511287,
1.,0.923879532511287,1.))
REPRESENTATION_ITEM('')
);
#1895=(
BOUNDED_CURVE()
B_SPLINE_CURVE(2,(#33699,#33700,#33701,#33702,#33703,#33704,#33705,#33706,
#33707),.UNSPECIFIED.,.F.,.F.)
B_SPLINE_CURVE_WITH_KNOTS((3,2,2,2,3),(0.5625,0.59375,0.625,0.65625,0.6875),
 .UNSPECIFIED.)
CURVE()
GEOMETRIC_REPRESENTATION_ITEM()
RATIONAL_B_SPLINE_CURVE((1.,0.923879532511287,1.,0.923879532511287,1.,0.923879532511287,
1.,0.923879532511287,1.))
REPRESENTATION_ITEM('')
);
#1896=(
BOUNDED_CURVE()
B_SPLINE_CURVE(2,(#33709,#33710,#33711,#33712,#33713,#33714,#33715,#33716,
#33717),.UNSPECIFIED.,.F.,.F.)
B_SPLINE_CURVE_WITH_KNOTS((3,2,2,2,3),(0.4375,0.46875,0.5,0.53125,0.5625),
 .UNSPECIFIED.)
CURVE()
GEOMETRIC_REPRESENTATION_ITEM()
RATIONAL_B_SPLINE_CURVE((1.,0.923879532511287,1.,0.923879532511287,1.,0.923879532511287,
1.,0.923879532511287,1.))
REPRESENTATION_ITEM('')
);
#1897=(
BOUNDED_CURVE()
B_SPLINE_CURVE(2,(#33719,#33720,#33721,#33722,#33723,#33724,#33725,#33726,
#33727),.UNSPECIFIED.,.F.,.F.)
B_SPLINE_CURVE_WITH_KNOTS((3,2,2,2,3),(0.3125,0.34375,0.375,0.40625,0.4375),
 .UNSPECIFIED.)
CURVE()
GEOMETRIC_REPRESENTATION_ITEM()
RATIONAL_B_SPLINE_CURVE((1.,0.923879532511287,1.,0.923879532511287,1.,0.923879532511287,
1.,0.923879532511287,1.))
REPRESENTATION_ITEM('')
);
#1898=(
BOUNDED_CURVE()
B_SPLINE_CURVE(2,(#33729,#33730,#33731,#33732,#33733,#33734,#33735,#33736,
#33737),.UNSPECIFIED.,.F.,.F.)
B_SPLINE_CURVE_WITH_KNOTS((3,2,2,2,3),(0.1875,0.21875,0.25,0.28125,0.3125),
 .UNSPECIFIED.)
CURVE()
GEOMETRIC_REPRESENTATION_ITEM()
RATIONAL_B_SPLINE_CURVE((1.,0.923879532511287,1.,0.923879532511287,1.,0.923879532511287,
1.,0.923879532511287,1.))
REPRESENTATION_ITEM('')
);
#1899=(
BOUNDED_CURVE()
B_SPLINE_CURVE(2,(#33739,#33740,#33741,#33742,#33743,#33744,#33745,#33746,
#33747),.UNSPECIFIED.,.F.,.F.)
B_SPLINE_CURVE_WITH_KNOTS((3,2,2,2,3),(0.0625,0.09375,0.125,0.15625,0.1875),
 .UNSPECIFIED.)
CURVE()
GEOMETRIC_REPRESENTATION_ITEM()
RATIONAL_B_SPLINE_CURVE((1.,0.923879532511287,1.,0.923879532511287,1.,0.923879532511287,
1.,0.923879532511287,1.))
REPRESENTATION_ITEM('')
);
#1900=(
BOUNDED_CURVE()
B_SPLINE_CURVE(2,(#33749,#33750,#33751,#33752,#33753),.UNSPECIFIED.,.F.,
 .F.)
B_SPLINE_CURVE_WITH_KNOTS((3,2,3),(0.,0.03125,0.0625),.UNSPECIFIED.)
CURVE()
GEOMETRIC_REPRESENTATION_ITEM()
RATIONAL_B_SPLINE_CURVE((1.,0.923879532511287,1.,0.923879532511287,1.))
REPRESENTATION_ITEM('')
);
#1901=(
BOUNDED_CURVE()
B_SPLINE_CURVE(2,(#33757,#33758,#33759,#33760,#33761,#33762,#33763,#33764,
#33765,#33766,#33767,#33768,#33769,#33770,#33771,#33772,#33773,#33774,#33775,
#33776,#33777,#33778,#33779,#33780,#33781,#33782,#33783,#33784,#33785,#33786,
#33787,#33788,#33789,#33790,#33791,#33792,#33793,#33794,#33795,#33796,#33797,
#33798,#33799,#33800,#33801,#33802,#33803,#33804,#33805,#33806,#33807,#33808,
#33809,#33810,#33811,#33812,#33813),.UNSPECIFIED.,.F.,.F.)
B_SPLINE_CURVE_WITH_KNOTS((3,2,2,2,2,2,2,2,2,2,2,2,2,2,2,2,2,2,2,2,2,2,
2,2,2,2,2,2,3),(0.,0.03125,0.0625,0.09375,0.125,0.15625,0.1875,0.21875,
0.25,0.28125,0.3125,0.34375,0.375,0.40625,0.4375,0.46875,0.5,0.53125,0.5625,
0.59375,0.625,0.65625,0.6875,0.71875,0.75,0.78125,0.8125,0.84375,0.875),
 .UNSPECIFIED.)
CURVE()
GEOMETRIC_REPRESENTATION_ITEM()
RATIONAL_B_SPLINE_CURVE((1.,0.923879532511287,1.,0.923879532511287,1.,0.923879532511287,
1.,0.923879532511287,1.,0.923879532511287,1.,0.923879532511287,1.,0.923879532511287,
1.,0.923879532511287,1.,0.923879532511287,1.,0.923879532511287,1.,0.923879532511287,
1.,0.923879532511287,1.,0.923879532511287,1.,0.923879532511287,1.,0.923879532511287,
1.,0.923879532511287,1.,0.923879532511287,1.,0.923879532511287,1.,0.923879532511287,
1.,0.923879532511287,1.,0.923879532511287,1.,0.923879532511287,1.,0.923879532511287,
1.,0.923879532511287,1.,0.923879532511287,1.,0.923879532511287,1.,0.923879532511287,
1.,0.923879532511287,1.))
REPRESENTATION_ITEM('')
);
#1902=(
BOUNDED_CURVE()
B_SPLINE_CURVE(2,(#33933,#33934,#33935,#33936,#33937),.UNSPECIFIED.,.F.,
 .F.)
B_SPLINE_CURVE_WITH_KNOTS((3,2,3),(0.,0.03125,0.0625),.UNSPECIFIED.)
CURVE()
GEOMETRIC_REPRESENTATION_ITEM()
RATIONAL_B_SPLINE_CURVE((1.,0.923879532511287,1.,0.923879532511287,1.))
REPRESENTATION_ITEM('')
);
#1903=(
BOUNDED_CURVE()
B_SPLINE_CURVE(2,(#33939,#33940,#33941,#33942,#33943,#33944,#33945,#33946,
#33947),.UNSPECIFIED.,.F.,.F.)
B_SPLINE_CURVE_WITH_KNOTS((3,2,2,2,3),(0.0625,0.09375,0.125,0.15625,0.1875),
 .UNSPECIFIED.)
CURVE()
GEOMETRIC_REPRESENTATION_ITEM()
RATIONAL_B_SPLINE_CURVE((1.,0.923879532511287,1.,0.923879532511287,1.,0.923879532511287,
1.,0.923879532511287,1.))
REPRESENTATION_ITEM('')
);
#1904=(
BOUNDED_CURVE()
B_SPLINE_CURVE(2,(#33949,#33950,#33951,#33952,#33953,#33954,#33955,#33956,
#33957),.UNSPECIFIED.,.F.,.F.)
B_SPLINE_CURVE_WITH_KNOTS((3,2,2,2,3),(0.1875,0.21875,0.25,0.28125,0.3125),
 .UNSPECIFIED.)
CURVE()
GEOMETRIC_REPRESENTATION_ITEM()
RATIONAL_B_SPLINE_CURVE((1.,0.923879532511287,1.,0.923879532511287,1.,0.923879532511287,
1.,0.923879532511287,1.))
REPRESENTATION_ITEM('')
);
#1905=(
BOUNDED_CURVE()
B_SPLINE_CURVE(2,(#33959,#33960,#33961,#33962,#33963,#33964,#33965,#33966,
#33967),.UNSPECIFIED.,.F.,.F.)
B_SPLINE_CURVE_WITH_KNOTS((3,2,2,2,3),(0.3125,0.34375,0.375,0.40625,0.4375),
 .UNSPECIFIED.)
CURVE()
GEOMETRIC_REPRESENTATION_ITEM()
RATIONAL_B_SPLINE_CURVE((1.,0.923879532511287,1.,0.923879532511287,1.,0.923879532511287,
1.,0.923879532511287,1.))
REPRESENTATION_ITEM('')
);
#1906=(
BOUNDED_CURVE()
B_SPLINE_CURVE(2,(#33969,#33970,#33971,#33972,#33973,#33974,#33975,#33976,
#33977),.UNSPECIFIED.,.F.,.F.)
B_SPLINE_CURVE_WITH_KNOTS((3,2,2,2,3),(0.4375,0.46875,0.5,0.53125,0.5625),
 .UNSPECIFIED.)
CURVE()
GEOMETRIC_REPRESENTATION_ITEM()
RATIONAL_B_SPLINE_CURVE((1.,0.923879532511287,1.,0.923879532511287,1.,0.923879532511287,
1.,0.923879532511287,1.))
REPRESENTATION_ITEM('')
);
#1907=(
BOUNDED_CURVE()
B_SPLINE_CURVE(2,(#33979,#33980,#33981,#33982,#33983,#33984,#33985,#33986,
#33987),.UNSPECIFIED.,.F.,.F.)
B_SPLINE_CURVE_WITH_KNOTS((3,2,2,2,3),(0.5625,0.59375,0.625,0.65625,0.6875),
 .UNSPECIFIED.)
CURVE()
GEOMETRIC_REPRESENTATION_ITEM()
RATIONAL_B_SPLINE_CURVE((1.,0.923879532511287,1.,0.923879532511287,1.,0.923879532511287,
1.,0.923879532511287,1.))
REPRESENTATION_ITEM('')
);
#1908=(
BOUNDED_CURVE()
B_SPLINE_CURVE(2,(#33989,#33990,#33991,#33992,#33993,#33994,#33995,#33996,
#33997),.UNSPECIFIED.,.F.,.F.)
B_SPLINE_CURVE_WITH_KNOTS((3,2,2,2,3),(0.6875,0.71875,0.75,0.78125,0.8125),
 .UNSPECIFIED.)
CURVE()
GEOMETRIC_REPRESENTATION_ITEM()
RATIONAL_B_SPLINE_CURVE((1.,0.923879532511287,1.,0.923879532511287,1.,0.923879532511287,
1.,0.923879532511287,1.))
REPRESENTATION_ITEM('')
);
#1909=(
BOUNDED_CURVE()
B_SPLINE_CURVE(2,(#33999,#34000,#34001,#34002,#34003),.UNSPECIFIED.,.F.,
 .F.)
B_SPLINE_CURVE_WITH_KNOTS((3,2,3),(0.8125,0.84375,0.875),.UNSPECIFIED.)
CURVE()
GEOMETRIC_REPRESENTATION_ITEM()
RATIONAL_B_SPLINE_CURVE((1.,0.923879532511287,1.,0.923879532511287,1.))
REPRESENTATION_ITEM('')
);
#1910=(
BOUNDED_CURVE()
B_SPLINE_CURVE(2,(#34007,#34008,#34009,#34010,#34011,#34012,#34013,#34014,
#34015,#34016,#34017,#34018,#34019,#34020,#34021,#34022,#34023,#34024,#34025,
#34026,#34027,#34028,#34029,#34030,#34031,#34032,#34033,#34034,#34035,#34036,
#34037,#34038,#34039,#34040,#34041,#34042,#34043,#34044,#34045,#34046,#34047,
#34048,#34049,#34050,#34051,#34052,#34053,#34054,#34055,#34056,#34057,#34058,
#34059,#34060,#34061,#34062,#34063),.UNSPECIFIED.,.F.,.F.)
B_SPLINE_CURVE_WITH_KNOTS((3,2,2,2,2,2,2,2,2,2,2,2,2,2,2,2,2,2,2,2,2,2,
2,2,2,2,2,2,3),(0.,0.03125,0.0625,0.09375,0.125,0.15625,0.1875,0.21875,
0.25,0.28125,0.3125,0.34375,0.375,0.40625,0.4375,0.46875,0.5,0.53125,0.5625,
0.59375,0.625,0.65625,0.6875,0.71875,0.75,0.78125,0.8125,0.84375,0.875),
 .UNSPECIFIED.)
CURVE()
GEOMETRIC_REPRESENTATION_ITEM()
RATIONAL_B_SPLINE_CURVE((1.,0.923879532511287,1.,0.923879532511287,1.,0.923879532511287,
1.,0.923879532511287,1.,0.923879532511287,1.,0.923879532511287,1.,0.923879532511287,
1.,0.923879532511287,1.,0.923879532511287,1.,0.923879532511287,1.,0.923879532511287,
1.,0.923879532511287,1.,0.923879532511287,1.,0.923879532511287,1.,0.923879532511287,
1.,0.923879532511287,1.,0.923879532511287,1.,0.923879532511287,1.,0.923879532511287,
1.,0.923879532511287,1.,0.923879532511287,1.,0.923879532511287,1.,0.923879532511287,
1.,0.923879532511287,1.,0.923879532511287,1.,0.923879532511287,1.,0.923879532511287,
1.,0.923879532511287,1.))
REPRESENTATION_ITEM('')
);
#1911=(
BOUNDED_CURVE()
B_SPLINE_CURVE(2,(#35726,#35727,#35728,#35729,#35730,#35731,#35732,#35733,
#35734),.UNSPECIFIED.,.F.,.F.)
B_SPLINE_CURVE_WITH_KNOTS((3,2,2,2,3),(0.,0.03125,0.0625,0.09375,0.125),
 .UNSPECIFIED.)
CURVE()
GEOMETRIC_REPRESENTATION_ITEM()
RATIONAL_B_SPLINE_CURVE((1.,0.923879532511287,1.,0.923879532511287,1.,0.923879532511287,
1.,0.923879532511287,1.))
REPRESENTATION_ITEM('')
);
#1912=(
BOUNDED_CURVE()
B_SPLINE_CURVE(2,(#35736,#35737,#35738,#35739,#35740,#35741,#35742,#35743,
#35744),.UNSPECIFIED.,.F.,.F.)
B_SPLINE_CURVE_WITH_KNOTS((3,2,2,2,3),(0.125,0.15625,0.1875,0.21875,0.25),
 .UNSPECIFIED.)
CURVE()
GEOMETRIC_REPRESENTATION_ITEM()
RATIONAL_B_SPLINE_CURVE((1.,0.923879532511287,1.,0.923879532511287,1.,0.923879532511287,
1.,0.923879532511286,1.))
REPRESENTATION_ITEM('')
);
#1913=(
BOUNDED_CURVE()
B_SPLINE_CURVE(2,(#35746,#35747,#35748,#35749,#35750,#35751,#35752,#35753,
#35754),.UNSPECIFIED.,.F.,.F.)
B_SPLINE_CURVE_WITH_KNOTS((3,2,2,2,3),(0.25,0.28125,0.3125,0.34375,0.375),
 .UNSPECIFIED.)
CURVE()
GEOMETRIC_REPRESENTATION_ITEM()
RATIONAL_B_SPLINE_CURVE((1.,0.923879532511287,1.,0.923879532511287,1.,0.923879532511287,
1.,0.923879532511288,1.))
REPRESENTATION_ITEM('')
);
#1914=(
BOUNDED_CURVE()
B_SPLINE_CURVE(2,(#35756,#35757,#35758,#35759,#35760,#35761,#35762,#35763,
#35764),.UNSPECIFIED.,.F.,.F.)
B_SPLINE_CURVE_WITH_KNOTS((3,2,2,2,3),(0.375,0.40625,0.4375,0.46875,0.5),
 .UNSPECIFIED.)
CURVE()
GEOMETRIC_REPRESENTATION_ITEM()
RATIONAL_B_SPLINE_CURVE((1.,0.923879532511286,1.,0.923879532511287,1.,0.923879532511287,
1.,0.923879532511287,1.))
REPRESENTATION_ITEM('')
);
#1915=(
BOUNDED_CURVE()
B_SPLINE_CURVE(2,(#35766,#35767,#35768,#35769,#35770,#35771,#35772,#35773,
#35774),.UNSPECIFIED.,.F.,.F.)
B_SPLINE_CURVE_WITH_KNOTS((3,2,2,2,3),(0.5,0.53125,0.5625,0.59375,0.625),
 .UNSPECIFIED.)
CURVE()
GEOMETRIC_REPRESENTATION_ITEM()
RATIONAL_B_SPLINE_CURVE((1.,0.923879532511286,1.,0.923879532511287,1.,0.923879532511287,
1.,0.923879532511287,1.))
REPRESENTATION_ITEM('')
);
#1916=(
BOUNDED_CURVE()
B_SPLINE_CURVE(2,(#35776,#35777,#35778,#35779,#35780,#35781,#35782,#35783,
#35784),.UNSPECIFIED.,.F.,.F.)
B_SPLINE_CURVE_WITH_KNOTS((3,2,2,2,3),(0.625,0.65625,0.6875,0.71875,0.75),
 .UNSPECIFIED.)
CURVE()
GEOMETRIC_REPRESENTATION_ITEM()
RATIONAL_B_SPLINE_CURVE((1.,0.923879532511287,1.,0.923879532511287,1.,0.923879532511287,
1.,0.923879532511287,1.))
REPRESENTATION_ITEM('')
);
#1917=(
BOUNDED_CURVE()
B_SPLINE_CURVE(2,(#35786,#35787,#35788,#35789,#35790,#35791,#35792,#35793,
#35794),.UNSPECIFIED.,.F.,.F.)
B_SPLINE_CURVE_WITH_KNOTS((3,2,2,2,3),(0.75,0.78125,0.8125,0.84375,0.875),
 .UNSPECIFIED.)
CURVE()
GEOMETRIC_REPRESENTATION_ITEM()
RATIONAL_B_SPLINE_CURVE((1.,0.923879532511287,1.,0.923879532511287,1.,0.923879532511287,
1.,0.923879532511287,1.))
REPRESENTATION_ITEM('')
);
#1918=(
BOUNDED_CURVE()
B_SPLINE_CURVE(2,(#35796,#35797,#35798,#35799,#35800,#35801,#35802,#35803,
#35804),.UNSPECIFIED.,.F.,.F.)
B_SPLINE_CURVE_WITH_KNOTS((3,2,2,2,3),(0.875,0.90625,0.9375,0.96875,1.),
 .UNSPECIFIED.)
CURVE()
GEOMETRIC_REPRESENTATION_ITEM()
RATIONAL_B_SPLINE_CURVE((1.,0.923879532511287,1.,0.923879532511287,1.,0.923879532511287,
1.,0.923879532511287,1.))
REPRESENTATION_ITEM('')
);
#1919=(
BOUNDED_CURVE()
B_SPLINE_CURVE(2,(#35808,#35809,#35810,#35811,#35812,#35813,#35814,#35815,
#35816,#35817,#35818,#35819,#35820,#35821,#35822,#35823,#35824,#35825,#35826,
#35827,#35828,#35829,#35830,#35831,#35832,#35833,#35834,#35835,#35836,#35837,
#35838,#35839,#35840,#35841,#35842,#35843,#35844,#35845,#35846,#35847,#35848,
#35849,#35850,#35851,#35852,#35853,#35854,#35855,#35856,#35857,#35858,#35859,
#35860,#35861,#35862,#35863,#35864,#35865,#35866,#35867,#35868,#35869,#35870,
#35871,#35872),.UNSPECIFIED.,.F.,.F.)
B_SPLINE_CURVE_WITH_KNOTS((3,2,2,2,2,2,2,2,2,2,2,2,2,2,2,2,2,2,2,2,2,2,
2,2,2,2,2,2,2,2,2,2,3),(0.,0.03125,0.0625,0.09375,0.125,0.15625,0.1875,
0.21875,0.25,0.28125,0.3125,0.34375,0.375,0.40625,0.4375,0.46875,0.5,0.53125,
0.5625,0.59375,0.625,0.65625,0.6875,0.71875,0.75,0.78125,0.8125,0.84375,
0.875,0.90625,0.9375,0.96875,1.),.UNSPECIFIED.)
CURVE()
GEOMETRIC_REPRESENTATION_ITEM()
RATIONAL_B_SPLINE_CURVE((1.,0.923879532511287,1.,0.923879532511287,1.,0.923879532511287,
1.,0.923879532511287,1.,0.923879532511287,1.,0.923879532511287,1.,0.923879532511287,
1.,0.923879532511287,1.,0.923879532511287,1.,0.923879532511287,1.,0.923879532511287,
1.,0.923879532511287,1.,0.923879532511287,1.,0.923879532511287,1.,0.923879532511287,
1.,0.923879532511287,1.,0.923879532511287,1.,0.923879532511287,1.,0.923879532511287,
1.,0.923879532511287,1.,0.923879532511287,1.,0.923879532511287,1.,0.923879532511287,
1.,0.923879532511287,1.,0.923879532511287,1.,0.923879532511287,1.,0.923879532511287,
1.,0.923879532511287,1.,0.923879532511287,1.,0.923879532511287,1.,0.923879532511287,
1.,0.923879532511287,1.))
REPRESENTATION_ITEM('')
);
#1920=(
BOUNDED_CURVE()
B_SPLINE_CURVE(2,(#36006,#36007,#36008,#36009,#36010,#36011,#36012,#36013,
#36014,#36015,#36016,#36017,#36018,#36019,#36020,#36021,#36022,#36023,#36024,
#36025,#36026,#36027,#36028,#36029,#36030,#36031,#36032,#36033,#36034,#36035,
#36036,#36037,#36038,#36039,#36040,#36041,#36042,#36043,#36044,#36045,#36046,
#36047,#36048,#36049,#36050,#36051,#36052,#36053,#36054,#36055,#36056,#36057,
#36058,#36059,#36060,#36061,#36062,#36063,#36064,#36065,#36066,#36067,#36068,
#36069,#36070),.UNSPECIFIED.,.F.,.F.)
B_SPLINE_CURVE_WITH_KNOTS((3,2,2,2,2,2,2,2,2,2,2,2,2,2,2,2,2,2,2,2,2,2,
2,2,2,2,2,2,2,2,2,2,3),(0.,0.03125,0.0625,0.09375,0.125,0.15625,0.1875,
0.21875,0.25,0.28125,0.3125,0.34375,0.375,0.40625,0.4375,0.46875,0.5,0.53125,
0.5625,0.59375,0.625,0.65625,0.6875,0.71875,0.75,0.78125,0.8125,0.84375,
0.875,0.90625,0.9375,0.96875,1.),.UNSPECIFIED.)
CURVE()
GEOMETRIC_REPRESENTATION_ITEM()
RATIONAL_B_SPLINE_CURVE((1.,0.923879532511287,1.,0.923879532511287,1.,0.923879532511287,
1.,0.923879532511287,1.,0.923879532511287,1.,0.923879532511287,1.,0.923879532511287,
1.,0.923879532511287,1.,0.923879532511287,1.,0.923879532511287,1.,0.923879532511287,
1.,0.923879532511287,1.,0.923879532511287,1.,0.923879532511287,1.,0.923879532511287,
1.,0.923879532511287,1.,0.923879532511287,1.,0.923879532511287,1.,0.923879532511287,
1.,0.923879532511287,1.,0.923879532511287,1.,0.923879532511287,1.,0.923879532511287,
1.,0.923879532511287,1.,0.923879532511287,1.,0.923879532511287,1.,0.923879532511287,
1.,0.923879532511287,1.,0.923879532511287,1.,0.923879532511287,1.,0.923879532511287,
1.,0.923879532511287,1.))
REPRESENTATION_ITEM('')
);
#1921=(
BOUNDED_CURVE()
B_SPLINE_CURVE(2,(#36074,#36075,#36076,#36077,#36078,#36079,#36080,#36081,
#36082),.UNSPECIFIED.,.F.,.F.)
B_SPLINE_CURVE_WITH_KNOTS((3,2,2,2,3),(0.875,0.90625,0.9375,0.96875,1.),
 .UNSPECIFIED.)
CURVE()
GEOMETRIC_REPRESENTATION_ITEM()
RATIONAL_B_SPLINE_CURVE((1.,0.923879532511287,1.,0.923879532511287,1.,0.923879532511287,
1.,0.923879532511287,1.))
REPRESENTATION_ITEM('')
);
#1922=(
BOUNDED_CURVE()
B_SPLINE_CURVE(2,(#36084,#36085,#36086,#36087,#36088,#36089,#36090,#36091,
#36092),.UNSPECIFIED.,.F.,.F.)
B_SPLINE_CURVE_WITH_KNOTS((3,2,2,2,3),(0.75,0.78125,0.8125,0.84375,0.875),
 .UNSPECIFIED.)
CURVE()
GEOMETRIC_REPRESENTATION_ITEM()
RATIONAL_B_SPLINE_CURVE((1.,0.923879532511287,1.,0.923879532511287,1.,0.923879532511287,
1.,0.923879532511287,1.))
REPRESENTATION_ITEM('')
);
#1923=(
BOUNDED_CURVE()
B_SPLINE_CURVE(2,(#36094,#36095,#36096,#36097,#36098,#36099,#36100,#36101,
#36102),.UNSPECIFIED.,.F.,.F.)
B_SPLINE_CURVE_WITH_KNOTS((3,2,2,2,3),(0.625,0.65625,0.6875,0.71875,0.75),
 .UNSPECIFIED.)
CURVE()
GEOMETRIC_REPRESENTATION_ITEM()
RATIONAL_B_SPLINE_CURVE((1.,0.923879532511287,1.,0.923879532511287,1.,0.923879532511287,
1.,0.923879532511287,1.))
REPRESENTATION_ITEM('')
);
#1924=(
BOUNDED_CURVE()
B_SPLINE_CURVE(2,(#36104,#36105,#36106,#36107,#36108,#36109,#36110,#36111,
#36112),.UNSPECIFIED.,.F.,.F.)
B_SPLINE_CURVE_WITH_KNOTS((3,2,2,2,3),(0.5,0.53125,0.5625,0.59375,0.625),
 .UNSPECIFIED.)
CURVE()
GEOMETRIC_REPRESENTATION_ITEM()
RATIONAL_B_SPLINE_CURVE((1.,0.923879532511286,1.,0.923879532511287,1.,0.923879532511287,
1.,0.923879532511287,1.))
REPRESENTATION_ITEM('')
);
#1925=(
BOUNDED_CURVE()
B_SPLINE_CURVE(2,(#36114,#36115,#36116,#36117,#36118,#36119,#36120,#36121,
#36122),.UNSPECIFIED.,.F.,.F.)
B_SPLINE_CURVE_WITH_KNOTS((3,2,2,2,3),(0.375,0.40625,0.4375,0.46875,0.5),
 .UNSPECIFIED.)
CURVE()
GEOMETRIC_REPRESENTATION_ITEM()
RATIONAL_B_SPLINE_CURVE((1.,0.923879532511287,1.,0.923879532511287,1.,0.923879532511287,
1.,0.923879532511287,1.))
REPRESENTATION_ITEM('')
);
#1926=(
BOUNDED_CURVE()
B_SPLINE_CURVE(2,(#36124,#36125,#36126,#36127,#36128,#36129,#36130,#36131,
#36132),.UNSPECIFIED.,.F.,.F.)
B_SPLINE_CURVE_WITH_KNOTS((3,2,2,2,3),(0.25,0.28125,0.3125,0.34375,0.375),
 .UNSPECIFIED.)
CURVE()
GEOMETRIC_REPRESENTATION_ITEM()
RATIONAL_B_SPLINE_CURVE((1.,0.923879532511287,1.,0.923879532511287,1.,0.923879532511287,
1.,0.923879532511286,1.))
REPRESENTATION_ITEM('')
);
#1927=(
BOUNDED_CURVE()
B_SPLINE_CURVE(2,(#36134,#36135,#36136,#36137,#36138,#36139,#36140,#36141,
#36142),.UNSPECIFIED.,.F.,.F.)
B_SPLINE_CURVE_WITH_KNOTS((3,2,2,2,3),(0.125,0.15625,0.1875,0.21875,0.25),
 .UNSPECIFIED.)
CURVE()
GEOMETRIC_REPRESENTATION_ITEM()
RATIONAL_B_SPLINE_CURVE((1.,0.923879532511287,1.,0.923879532511287,1.,0.923879532511287,
1.,0.923879532511286,1.))
REPRESENTATION_ITEM('')
);
#1928=(
BOUNDED_CURVE()
B_SPLINE_CURVE(2,(#36144,#36145,#36146,#36147,#36148,#36149,#36150,#36151,
#36152),.UNSPECIFIED.,.F.,.F.)
B_SPLINE_CURVE_WITH_KNOTS((3,2,2,2,3),(0.,0.03125,0.0625,0.09375,0.125),
 .UNSPECIFIED.)
CURVE()
GEOMETRIC_REPRESENTATION_ITEM()
RATIONAL_B_SPLINE_CURVE((1.,0.923879532511287,1.,0.923879532511287,1.,0.923879532511287,
1.,0.923879532511287,1.))
REPRESENTATION_ITEM('')
);
#1929=(
BOUNDED_CURVE()
B_SPLINE_CURVE(2,(#39732,#39733,#39734,#39735,#39736,#39737,#39738,#39739,
#39740,#39741,#39742,#39743,#39744,#39745,#39746,#39747,#39748,#39749,#39750,
#39751,#39752,#39753,#39754,#39755,#39756,#39757,#39758,#39759,#39760,#39761,
#39762,#39763,#39764,#39765,#39766,#39767,#39768,#39769,#39770,#39771,#39772,
#39773,#39774,#39775,#39776,#39777,#39778,#39779,#39780,#39781,#39782,#39783,
#39784,#39785,#39786,#39787,#39788,#39789,#39790,#39791,#39792,#39793,#39794,
#39795,#39796,#39797,#39798,#39799,#39800,#39801,#39802,#39803,#39804,#39805,
#39806,#39807,#39808,#39809,#39810),.UNSPECIFIED.,.F.,.F.)
B_SPLINE_CURVE_WITH_KNOTS((3,2,2,2,2,2,2,2,2,2,2,2,2,2,2,2,2,2,2,2,2,2,
2,2,2,2,2,2,2,2,2,2,2,2,2,2,2,2,2,3),(0.,0.025,0.05,0.075,0.1,0.125,0.15,
0.175,0.2,0.225,0.25,0.275,0.3,0.325,0.35,0.375,0.4,0.425,0.45,0.475,0.5,
0.525,0.55,0.575,0.6,0.625,0.65,0.675,0.7,0.725,0.75,0.775,0.8,0.825,0.85,
0.875,0.9,0.925,0.95,0.964550284056263),.UNSPECIFIED.)
CURVE()
GEOMETRIC_REPRESENTATION_ITEM()
RATIONAL_B_SPLINE_CURVE((1.,0.951056516295154,1.,0.951056516295154,1.,0.951056516295154,
1.,0.951056516295154,1.,0.951056516295154,1.,0.951056516295154,1.,0.951056516295154,
1.,0.951056516295154,1.,0.951056516295154,1.,0.951056516295154,1.,0.951056516295154,
1.,0.951056516295154,1.,0.951056516295154,1.,0.951056516295154,1.,0.951056516295154,
1.,0.951056516295154,1.,0.951056516295154,1.,0.951056516295154,1.,0.951056516295154,
1.,0.951056516295154,1.,0.951056516295154,1.,0.951056516295154,1.,0.951056516295154,
1.,0.951056516295154,1.,0.951056516295154,1.,0.951056516295154,1.,0.951056516295154,
1.,0.951056516295154,1.,0.951056516295154,1.,0.951056516295154,1.,0.951056516295154,
1.,0.951056516295154,1.,0.951056516295154,1.,0.951056516295154,1.,0.951056516295154,
1.,0.951056516295154,1.,0.951056516295154,1.,0.951056516295154,1.,0.971514336375656,
0.976186632532541))
REPRESENTATION_ITEM('')
);
#1930=(
BOUNDED_CURVE()
B_SPLINE_CURVE(2,(#39814,#39815,#39816,#39817,#39818),.UNSPECIFIED.,.F.,
 .F.)
B_SPLINE_CURVE_WITH_KNOTS((3,2,3),(0.9375,0.95,0.9645502840563),
 .UNSPECIFIED.)
CURVE()
GEOMETRIC_REPRESENTATION_ITEM()
RATIONAL_B_SPLINE_CURVE((0.975528258147577,0.975528258147577,1.,0.971514336375583,
0.976186632532565))
REPRESENTATION_ITEM('')
);
#1931=(
BOUNDED_CURVE()
B_SPLINE_CURVE(2,(#39820,#39821,#39822,#39823,#39824,#39825,#39826,#39827,
#39828,#39829,#39830,#39831,#39832),.UNSPECIFIED.,.F.,.F.)
B_SPLINE_CURVE_WITH_KNOTS((3,2,2,2,2,2,3),(0.8125,0.825,0.85,0.875,0.9,
0.925,0.9375),.UNSPECIFIED.)
CURVE()
GEOMETRIC_REPRESENTATION_ITEM()
RATIONAL_B_SPLINE_CURVE((0.975528258147577,0.975528258147577,1.,0.951056516295154,
1.,0.951056516295154,1.,0.951056516295154,1.,0.951056516295154,1.,0.975528258147577,
0.975528258147577))
REPRESENTATION_ITEM('')
);
#1932=(
BOUNDED_CURVE()
B_SPLINE_CURVE(2,(#39834,#39835,#39836,#39837,#39838,#39839,#39840,#39841,
#39842,#39843,#39844,#39845,#39846),.UNSPECIFIED.,.F.,.F.)
B_SPLINE_CURVE_WITH_KNOTS((3,2,2,2,2,2,3),(0.6875,0.7,0.725,0.75,0.775,
0.8,0.8125),.UNSPECIFIED.)
CURVE()
GEOMETRIC_REPRESENTATION_ITEM()
RATIONAL_B_SPLINE_CURVE((0.975528258147577,0.975528258147577,1.,0.951056516295154,
1.,0.951056516295154,1.,0.951056516295154,1.,0.951056516295154,1.,0.975528258147577,
0.975528258147577))
REPRESENTATION_ITEM('')
);
#1933=(
BOUNDED_CURVE()
B_SPLINE_CURVE(2,(#39848,#39849,#39850,#39851,#39852,#39853,#39854,#39855,
#39856,#39857,#39858,#39859,#39860),.UNSPECIFIED.,.F.,.F.)
B_SPLINE_CURVE_WITH_KNOTS((3,2,2,2,2,2,3),(0.5625,0.575,0.6,0.625,0.65,
0.675,0.6875),.UNSPECIFIED.)
CURVE()
GEOMETRIC_REPRESENTATION_ITEM()
RATIONAL_B_SPLINE_CURVE((0.975528258147577,0.975528258147577,1.,0.951056516295154,
1.,0.951056516295154,1.,0.951056516295154,1.,0.951056516295154,1.,0.975528258147577,
0.975528258147577))
REPRESENTATION_ITEM('')
);
#1934=(
BOUNDED_CURVE()
B_SPLINE_CURVE(2,(#39862,#39863,#39864,#39865,#39866,#39867,#39868,#39869,
#39870,#39871,#39872,#39873,#39874),.UNSPECIFIED.,.F.,.F.)
B_SPLINE_CURVE_WITH_KNOTS((3,2,2,2,2,2,3),(0.4375,0.45,0.475,0.5,0.525,
0.55,0.5625),.UNSPECIFIED.)
CURVE()
GEOMETRIC_REPRESENTATION_ITEM()
RATIONAL_B_SPLINE_CURVE((0.975528258147577,0.975528258147577,1.,0.951056516295154,
1.,0.951056516295154,1.,0.951056516295154,1.,0.951056516295154,1.,0.975528258147577,
0.975528258147577))
REPRESENTATION_ITEM('')
);
#1935=(
BOUNDED_CURVE()
B_SPLINE_CURVE(2,(#39876,#39877,#39878,#39879,#39880,#39881,#39882,#39883,
#39884,#39885,#39886,#39887,#39888),.UNSPECIFIED.,.F.,.F.)
B_SPLINE_CURVE_WITH_KNOTS((3,2,2,2,2,2,3),(0.3125,0.325,0.35,0.375,0.4,
0.425,0.4375),.UNSPECIFIED.)
CURVE()
GEOMETRIC_REPRESENTATION_ITEM()
RATIONAL_B_SPLINE_CURVE((0.975528258147577,0.975528258147577,1.,0.951056516295154,
1.,0.951056516295154,1.,0.951056516295154,1.,0.951056516295154,1.,0.975528258147577,
0.975528258147577))
REPRESENTATION_ITEM('')
);
#1936=(
BOUNDED_CURVE()
B_SPLINE_CURVE(2,(#39890,#39891,#39892,#39893,#39894,#39895,#39896,#39897,
#39898,#39899,#39900,#39901,#39902),.UNSPECIFIED.,.F.,.F.)
B_SPLINE_CURVE_WITH_KNOTS((3,2,2,2,2,2,3),(0.1875,0.2,0.225,0.25,0.275,
0.3,0.3125),.UNSPECIFIED.)
CURVE()
GEOMETRIC_REPRESENTATION_ITEM()
RATIONAL_B_SPLINE_CURVE((0.975528258147577,0.975528258147577,1.,0.951056516295154,
1.,0.951056516295154,1.,0.951056516295154,1.,0.951056516295154,1.,0.975528258147577,
0.975528258147577))
REPRESENTATION_ITEM('')
);
#1937=(
BOUNDED_CURVE()
B_SPLINE_CURVE(2,(#39904,#39905,#39906,#39907,#39908,#39909,#39910,#39911,
#39912,#39913,#39914,#39915,#39916),.UNSPECIFIED.,.F.,.F.)
B_SPLINE_CURVE_WITH_KNOTS((3,2,2,2,2,2,3),(0.0625,0.075,0.1,0.125,0.15,
0.175,0.1875),.UNSPECIFIED.)
CURVE()
GEOMETRIC_REPRESENTATION_ITEM()
RATIONAL_B_SPLINE_CURVE((0.975528258147577,0.975528258147577,1.,0.951056516295154,
1.,0.951056516295154,1.,0.951056516295154,1.,0.951056516295154,1.,0.975528258147577,
0.975528258147577))
REPRESENTATION_ITEM('')
);
#1938=(
BOUNDED_CURVE()
B_SPLINE_CURVE(2,(#39918,#39919,#39920,#39921,#39922,#39923,#39924),
 .UNSPECIFIED.,.F.,.F.)
B_SPLINE_CURVE_WITH_KNOTS((3,2,2,3),(0.,0.025,0.05,0.0625),
 .UNSPECIFIED.)
CURVE()
GEOMETRIC_REPRESENTATION_ITEM()
RATIONAL_B_SPLINE_CURVE((1.,0.951056516295154,1.,0.951056516295154,1.,0.975528258147577,
0.975528258147577))
REPRESENTATION_ITEM('')
);
#1939=(
BOUNDED_CURVE()
B_SPLINE_CURVE(2,(#40171,#40172,#40173,#40174,#40175,#40176,#40177),
 .UNSPECIFIED.,.F.,.F.)
B_SPLINE_CURVE_WITH_KNOTS((3,2,2,3),(0.,0.00313236994712061,0.00626473989424123,
0.00783092486780153),.UNSPECIFIED.)
CURVE()
GEOMETRIC_REPRESENTATION_ITEM()
RATIONAL_B_SPLINE_CURVE((1.,0.951056516295154,1.,0.951056516295154,1.,0.975528258147577,
0.975528258147577))
REPRESENTATION_ITEM('')
);
#1940=(
BOUNDED_CURVE()
B_SPLINE_CURVE(2,(#40179,#40180,#40181,#40182,#40183,#40184,#40185,#40186,
#40187,#40188,#40189,#40190,#40191),.UNSPECIFIED.,.F.,.F.)
B_SPLINE_CURVE_WITH_KNOTS((3,2,2,2,2,2,3),(0.00783092486780153,0.00939686100434394,
0.0125287332774288,0.0156606055505136,0.0187924778235984,0.0219243500966832,
0.0234902862332256),.UNSPECIFIED.)
CURVE()
GEOMETRIC_REPRESENTATION_ITEM()
RATIONAL_B_SPLINE_CURVE((0.975528258147577,0.975528258147577,1.,0.951056516295154,
1.,0.951056516295154,1.,0.951056516295154,1.,0.951056516295154,1.,0.975528258147577,
0.975528258147577))
REPRESENTATION_ITEM('')
);
#1941=(
BOUNDED_CURVE()
B_SPLINE_CURVE(2,(#40193,#40194,#40195,#40196,#40197,#40198,#40199,#40200,
#40201,#40202,#40203,#40204,#40205),.UNSPECIFIED.,.F.,.F.)
B_SPLINE_CURVE_WITH_KNOTS((3,2,2,2,2,2,3),(0.0234902862332256,0.0250560316219713,
0.0281875223994624,0.0313190131769537,0.0344505039544449,0.0375819947319362,
0.0391477401206671),.UNSPECIFIED.)
CURVE()
GEOMETRIC_REPRESENTATION_ITEM()
RATIONAL_B_SPLINE_CURVE((0.975528258147577,0.975528258147577,1.,0.951056516295154,
1.,0.951056516295154,1.,0.951056516295154,1.,0.951056516295154,1.,0.975528258147807,
0.975528258147577))
REPRESENTATION_ITEM('')
);
#1942=(
BOUNDED_CURVE()
B_SPLINE_CURVE(2,(#40207,#40208,#40209,#40210,#40211,#40212,#40213,#40214,
#40215,#40216,#40217,#40218,#40219),.UNSPECIFIED.,.F.,.F.)
B_SPLINE_CURVE_WITH_KNOTS((3,2,2,2,2,2,3),(0.0391477401206671,0.0407138913050886,
0.0438461936739023,0.0469784960427159,0.0501107984115296,0.0532431007803432,
0.0548092519647501),.UNSPECIFIED.)
CURVE()
GEOMETRIC_REPRESENTATION_ITEM()
RATIONAL_B_SPLINE_CURVE((0.975528258147577,0.975528258147347,1.,0.951056516295154,
1.,0.951056516295154,1.,0.951056516295154,1.,0.951056516295154,1.,0.975528258147577,
0.975528258147577))
REPRESENTATION_ITEM('')
);
#1943=(
BOUNDED_CURVE()
B_SPLINE_CURVE(2,(#40221,#40222,#40223,#40224,#40225,#40226,#40227,#40228,
#40229,#40230,#40231,#40232,#40233),.UNSPECIFIED.,.F.,.F.)
B_SPLINE_CURVE_WITH_KNOTS((3,2,2,2,2,2,3),(0.0548092519647501,0.0563753388810186,
0.0595075127135556,0.0626396865460927,0.0657718603786298,0.0689040342111668,
0.0704701211274353),.UNSPECIFIED.)
CURVE()
GEOMETRIC_REPRESENTATION_ITEM()
RATIONAL_B_SPLINE_CURVE((0.975528258147577,0.975528258147577,1.,0.951056516295154,
1.,0.951056516295154,1.,0.951056516295154,1.,0.951056516295154,1.,0.975528258147577,
0.975528258147577))
REPRESENTATION_ITEM('')
);
#1944=(
BOUNDED_CURVE()
B_SPLINE_CURVE(2,(#40235,#40236,#40237,#40238,#40239,#40240,#40241,#40242,
#40243,#40244,#40245,#40246,#40247),.UNSPECIFIED.,.F.,.F.)
B_SPLINE_CURVE_WITH_KNOTS((3,2,2,2,2,2,3),(0.0704701211274353,0.0720358098879434,
0.0751671874089597,0.0782985649299759,0.0814299424509921,0.0845613199720083,
0.0861270087324948),.UNSPECIFIED.)
CURVE()
GEOMETRIC_REPRESENTATION_ITEM()
RATIONAL_B_SPLINE_CURVE((0.975528258147577,0.975528258147577,1.,0.951056516295154,
1.,0.951056516295154,1.,0.951056516295154,1.,0.951056516295154,1.,0.975528258147915,
0.975528258147577))
REPRESENTATION_ITEM('')
);
#1945=(
BOUNDED_CURVE()
B_SPLINE_CURVE(2,(#40249,#40250,#40251,#40252,#40253,#40254,#40255,#40256,
#40257,#40258,#40259,#40260,#40261),.UNSPECIFIED.,.F.,.F.)
B_SPLINE_CURVE_WITH_KNOTS((3,2,2,2,2,2,3),(0.0861270087324948,0.0876930566782528,
0.0908251525697255,0.0939572484611982,0.0970893443526709,0.100221440244144,
0.10178748818988),.UNSPECIFIED.)
CURVE()
GEOMETRIC_REPRESENTATION_ITEM()
RATIONAL_B_SPLINE_CURVE((0.975528258147577,0.975528258147239,1.,0.951056516295154,
1.,0.951056516295154,1.,0.951056516295154,1.,0.951056516295154,1.,0.975528258147576,
0.975528258147577))
REPRESENTATION_ITEM('')
);
#1946=(
BOUNDED_CURVE()
B_SPLINE_CURVE(2,(#40263,#40264,#40265,#40266,#40267,#40268,#40269,#40270,
#40271,#40272,#40273,#40274,#40275),.UNSPECIFIED.,.F.,.F.)
B_SPLINE_CURVE_WITH_KNOTS((3,2,2,2,2,2,3),(0.10178748818988,0.10335365715109,
0.106485995073509,0.109618332995928,0.112750670918347,0.115883008840766,
0.117449177801976),.UNSPECIFIED.)
CURVE()
GEOMETRIC_REPRESENTATION_ITEM()
RATIONAL_B_SPLINE_CURVE((0.975528258147577,0.975528258147577,1.,0.951056516295154,
1.,0.951056516295154,1.,0.951056516295154,1.,0.951056516295154,1.,0.97552825814758,
0.975528258147577))
REPRESENTATION_ITEM('')
);
#1947=(
BOUNDED_CURVE()
B_SPLINE_CURVE(2,(#40284,#40285,#40286,#40287,#40288,#40289,#40290,#40291,
#40292,#40293,#40294,#40295,#40296,#40297,#40298,#40299,#40300,#40301,#40302,
#40303,#40304,#40305,#40306,#40307,#40308,#40309,#40310,#40311,#40312,#40313,
#40314,#40315,#40316,#40317,#40318,#40319,#40320,#40321,#40322,#40323,#40324,
#40325,#40326,#40327,#40328,#40329,#40330,#40331,#40332,#40333,#40334,#40335,
#40336,#40337,#40338,#40339,#40340,#40341,#40342,#40343,#40344,#40345,#40346,
#40347,#40348,#40349,#40350,#40351,#40352,#40353,#40354,#40355,#40356,#40357,
#40358,#40359,#40360,#40361,#40362),.UNSPECIFIED.,.F.,.F.)
B_SPLINE_CURVE_WITH_KNOTS((3,2,2,2,2,2,2,2,2,2,2,2,2,2,2,2,2,2,2,2,2,2,
2,2,2,2,2,2,2,2,2,2,2,2,2,2,2,2,2,3),(0.,0.0259188146157259,0.0518376292314517,
0.0777564438471776,0.103675258462903,0.129594073078629,0.155512887694355,
0.181431702310081,0.207350516925807,0.233269331541533,0.259188146157258,
0.285106960772985,0.311025775388711,0.336944590004436,0.362863404620162,
0.388782219235888,0.414701033851614,0.440619848467339,0.466538663083066,
0.492457477698791,0.518376292314517,0.544295106930243,0.570213921545969,
0.596132736161695,0.622051550777421,0.647970365393147,0.673889180008872,
0.699807994624598,0.725726809240324,0.75164562385605,0.777564438471776,
0.803483253087502,0.829402067703228,0.855320882318953,0.881239696934679,
0.907158511550405,0.933077326166131,0.958996140781857,0.984914955397583,
1.),.UNSPECIFIED.)
CURVE()
GEOMETRIC_REPRESENTATION_ITEM()
RATIONAL_B_SPLINE_CURVE((1.,0.951056516295154,1.,0.951056516295154,1.,0.951056516295154,
1.,0.951056516295154,1.,0.951056516295154,1.,0.951056516295154,1.,0.951056516295154,
1.,0.951056516295154,1.,0.951056516295154,1.,0.951056516295154,1.,0.951056516295154,
1.,0.951056516295154,1.,0.951056516295154,1.,0.951056516295154,1.,0.951056516295154,
1.,0.951056516295154,1.,0.951056516295154,1.,0.951056516295154,1.,0.951056516295154,
1.,0.951056516295154,1.,0.951056516295154,1.,0.951056516295154,1.,0.951056516295154,
1.,0.951056516295154,1.,0.951056516295154,1.,0.951056516295154,1.,0.951056516295154,
1.,0.951056516295154,1.,0.951056516295154,1.,0.951056516295154,1.,0.951056516295154,
1.,0.951056516295154,1.,0.951056516295154,1.,0.951056516295154,1.,0.951056516295154,
1.,0.951056516295154,1.,0.951056516295154,1.,0.951056516295154,1.,0.971514336375656,
0.976186632532541))
REPRESENTATION_ITEM('')
);
#1948=(
BOUNDED_CURVE()
B_SPLINE_CURVE(2,(#41291,#41292,#41293,#41294,#41295,#41296,#41297,#41298,
#41299,#41300,#41301,#41302,#41303,#41304,#41305,#41306,#41307,#41308,#41309,
#41310,#41311,#41312,#41313,#41314,#41315,#41316,#41317,#41318,#41319,#41320,
#41321,#41322,#41323,#41324,#41325,#41326,#41327,#41328,#41329,#41330,#41331,
#41332,#41333,#41334,#41335,#41336,#41337,#41338,#41339,#41340,#41341,#41342,
#41343,#41344,#41345,#41346,#41347,#41348,#41349,#41350,#41351,#41352,#41353,
#41354,#41355),.UNSPECIFIED.,.F.,.F.)
B_SPLINE_CURVE_WITH_KNOTS((3,2,2,2,2,2,2,2,2,2,2,2,2,2,2,2,2,2,2,2,2,2,
2,2,2,2,2,2,2,2,2,2,3),(0.,0.03125,0.0625,0.09375,0.125,0.15625,0.1875,
0.21875,0.25,0.28125,0.3125,0.34375,0.375,0.40625,0.4375,0.46875,0.5,0.53125,
0.5625,0.59375,0.625,0.65625,0.6875,0.71875,0.75,0.78125,0.8125,0.84375,
0.875,0.90625,0.9375,0.96875,1.),.UNSPECIFIED.)
CURVE()
GEOMETRIC_REPRESENTATION_ITEM()
RATIONAL_B_SPLINE_CURVE((1.,0.923879532511287,1.,0.923879532511287,1.,0.923879532511287,
1.,0.923879532511287,1.,0.923879532511287,1.,0.923879532511287,1.,0.923879532511287,
1.,0.923879532511287,1.,0.923879532511287,1.,0.923879532511287,1.,0.923879532511287,
1.,0.923879532511287,1.,0.923879532511287,1.,0.923879532511287,1.,0.923879532511287,
1.,0.923879532511287,1.,0.923879532511287,1.,0.923879532511287,1.,0.923879532511287,
1.,0.923879532511287,1.,0.923879532511287,1.,0.923879532511287,1.,0.923879532511287,
1.,0.923879532511287,1.,0.923879532511287,1.,0.923879532511287,1.,0.923879532511287,
1.,0.923879532511287,1.,0.923879532511287,1.,0.923879532511287,1.,0.923879532511287,
1.,0.923879532511287,1.))
REPRESENTATION_ITEM('')
);
#1949=(
BOUNDED_CURVE()
B_SPLINE_CURVE(2,(#41359,#41360,#41361,#41362,#41363,#41364,#41365,#41366,
#41367),.UNSPECIFIED.,.F.,.F.)
B_SPLINE_CURVE_WITH_KNOTS((3,2,2,2,3),(0.875,0.90625,0.9375,0.96875,1.),
 .UNSPECIFIED.)
CURVE()
GEOMETRIC_REPRESENTATION_ITEM()
RATIONAL_B_SPLINE_CURVE((1.,0.923879532511287,1.,0.923879532511287,1.,0.923879532511287,
1.,0.923879532511287,1.))
REPRESENTATION_ITEM('')
);
#1950=(
BOUNDED_CURVE()
B_SPLINE_CURVE(2,(#41369,#41370,#41371,#41372,#41373,#41374,#41375,#41376,
#41377),.UNSPECIFIED.,.F.,.F.)
B_SPLINE_CURVE_WITH_KNOTS((3,2,2,2,3),(0.75,0.78125,0.8125,0.84375,0.875),
 .UNSPECIFIED.)
CURVE()
GEOMETRIC_REPRESENTATION_ITEM()
RATIONAL_B_SPLINE_CURVE((1.,0.923879532511287,1.,0.923879532511287,1.,0.923879532511287,
1.,0.923879532511287,1.))
REPRESENTATION_ITEM('')
);
#1951=(
BOUNDED_CURVE()
B_SPLINE_CURVE(2,(#41379,#41380,#41381,#41382,#41383,#41384,#41385,#41386,
#41387),.UNSPECIFIED.,.F.,.F.)
B_SPLINE_CURVE_WITH_KNOTS((3,2,2,2,3),(0.625,0.65625,0.6875,0.71875,0.75),
 .UNSPECIFIED.)
CURVE()
GEOMETRIC_REPRESENTATION_ITEM()
RATIONAL_B_SPLINE_CURVE((1.,0.923879532511287,1.,0.923879532511287,1.,0.923879532511287,
1.,0.923879532511287,1.))
REPRESENTATION_ITEM('')
);
#1952=(
BOUNDED_CURVE()
B_SPLINE_CURVE(2,(#41389,#41390,#41391,#41392,#41393,#41394,#41395,#41396,
#41397),.UNSPECIFIED.,.F.,.F.)
B_SPLINE_CURVE_WITH_KNOTS((3,2,2,2,3),(0.5,0.53125,0.5625,0.59375,0.625),
 .UNSPECIFIED.)
CURVE()
GEOMETRIC_REPRESENTATION_ITEM()
RATIONAL_B_SPLINE_CURVE((1.,0.923879532511286,1.,0.923879532511287,1.,0.923879532511287,
1.,0.923879532511287,1.))
REPRESENTATION_ITEM('')
);
#1953=(
BOUNDED_CURVE()
B_SPLINE_CURVE(2,(#41399,#41400,#41401,#41402,#41403,#41404,#41405,#41406,
#41407),.UNSPECIFIED.,.F.,.F.)
B_SPLINE_CURVE_WITH_KNOTS((3,2,2,2,3),(0.375,0.40625,0.4375,0.46875,0.5),
 .UNSPECIFIED.)
CURVE()
GEOMETRIC_REPRESENTATION_ITEM()
RATIONAL_B_SPLINE_CURVE((1.,0.923879532511286,1.,0.923879532511287,1.,0.923879532511287,
1.,0.923879532511287,1.))
REPRESENTATION_ITEM('')
);
#1954=(
BOUNDED_CURVE()
B_SPLINE_CURVE(2,(#41409,#41410,#41411,#41412,#41413,#41414,#41415,#41416,
#41417),.UNSPECIFIED.,.F.,.F.)
B_SPLINE_CURVE_WITH_KNOTS((3,2,2,2,3),(0.25,0.28125,0.3125,0.34375,0.375),
 .UNSPECIFIED.)
CURVE()
GEOMETRIC_REPRESENTATION_ITEM()
RATIONAL_B_SPLINE_CURVE((1.,0.923879532511287,1.,0.923879532511287,1.,0.923879532511287,
1.,0.923879532511288,1.))
REPRESENTATION_ITEM('')
);
#1955=(
BOUNDED_CURVE()
B_SPLINE_CURVE(2,(#41419,#41420,#41421,#41422,#41423,#41424,#41425,#41426,
#41427),.UNSPECIFIED.,.F.,.F.)
B_SPLINE_CURVE_WITH_KNOTS((3,2,2,2,3),(0.125,0.15625,0.1875,0.21875,0.25),
 .UNSPECIFIED.)
CURVE()
GEOMETRIC_REPRESENTATION_ITEM()
RATIONAL_B_SPLINE_CURVE((1.,0.923879532511287,1.,0.923879532511287,1.,0.923879532511287,
1.,0.923879532511286,1.))
REPRESENTATION_ITEM('')
);
#1956=(
BOUNDED_CURVE()
B_SPLINE_CURVE(2,(#41429,#41430,#41431,#41432,#41433,#41434,#41435,#41436,
#41437),.UNSPECIFIED.,.F.,.F.)
B_SPLINE_CURVE_WITH_KNOTS((3,2,2,2,3),(0.,0.03125,0.0625,0.09375,0.125),
 .UNSPECIFIED.)
CURVE()
GEOMETRIC_REPRESENTATION_ITEM()
RATIONAL_B_SPLINE_CURVE((1.,0.923879532511287,1.,0.923879532511287,1.,0.923879532511287,
1.,0.923879532511287,1.))
REPRESENTATION_ITEM('')
);
#1957=(
BOUNDED_CURVE()
B_SPLINE_CURVE(2,(#41571,#41572,#41573,#41574,#41575,#41576,#41577,#41578,
#41579),.UNSPECIFIED.,.F.,.F.)
B_SPLINE_CURVE_WITH_KNOTS((3,2,2,2,3),(0.,0.03125,0.0625,0.09375,0.125),
 .UNSPECIFIED.)
CURVE()
GEOMETRIC_REPRESENTATION_ITEM()
RATIONAL_B_SPLINE_CURVE((1.,0.923879532511287,1.,0.923879532511287,1.,0.923879532511287,
1.,0.923879532511287,1.))
REPRESENTATION_ITEM('')
);
#1958=(
BOUNDED_CURVE()
B_SPLINE_CURVE(2,(#41581,#41582,#41583,#41584,#41585,#41586,#41587,#41588,
#41589),.UNSPECIFIED.,.F.,.F.)
B_SPLINE_CURVE_WITH_KNOTS((3,2,2,2,3),(0.125,0.15625,0.1875,0.21875,0.25),
 .UNSPECIFIED.)
CURVE()
GEOMETRIC_REPRESENTATION_ITEM()
RATIONAL_B_SPLINE_CURVE((1.,0.923879532511287,1.,0.923879532511287,1.,0.923879532511287,
1.,0.923879532511286,1.))
REPRESENTATION_ITEM('')
);
#1959=(
BOUNDED_CURVE()
B_SPLINE_CURVE(2,(#41591,#41592,#41593,#41594,#41595,#41596,#41597,#41598,
#41599),.UNSPECIFIED.,.F.,.F.)
B_SPLINE_CURVE_WITH_KNOTS((3,2,2,2,3),(0.25,0.28125,0.3125,0.34375,0.375),
 .UNSPECIFIED.)
CURVE()
GEOMETRIC_REPRESENTATION_ITEM()
RATIONAL_B_SPLINE_CURVE((1.,0.923879532511287,1.,0.923879532511287,1.,0.923879532511287,
1.,0.923879532511286,1.))
REPRESENTATION_ITEM('')
);
#1960=(
BOUNDED_CURVE()
B_SPLINE_CURVE(2,(#41601,#41602,#41603,#41604,#41605,#41606,#41607,#41608,
#41609),.UNSPECIFIED.,.F.,.F.)
B_SPLINE_CURVE_WITH_KNOTS((3,2,2,2,3),(0.375,0.40625,0.4375,0.46875,0.5),
 .UNSPECIFIED.)
CURVE()
GEOMETRIC_REPRESENTATION_ITEM()
RATIONAL_B_SPLINE_CURVE((1.,0.923879532511287,1.,0.923879532511287,1.,0.923879532511287,
1.,0.923879532511287,1.))
REPRESENTATION_ITEM('')
);
#1961=(
BOUNDED_CURVE()
B_SPLINE_CURVE(2,(#41611,#41612,#41613,#41614,#41615,#41616,#41617,#41618,
#41619),.UNSPECIFIED.,.F.,.F.)
B_SPLINE_CURVE_WITH_KNOTS((3,2,2,2,3),(0.5,0.53125,0.5625,0.59375,0.625),
 .UNSPECIFIED.)
CURVE()
GEOMETRIC_REPRESENTATION_ITEM()
RATIONAL_B_SPLINE_CURVE((1.,0.923879532511286,1.,0.923879532511287,1.,0.923879532511287,
1.,0.923879532511287,1.))
REPRESENTATION_ITEM('')
);
#1962=(
BOUNDED_CURVE()
B_SPLINE_CURVE(2,(#41621,#41622,#41623,#41624,#41625,#41626,#41627,#41628,
#41629),.UNSPECIFIED.,.F.,.F.)
B_SPLINE_CURVE_WITH_KNOTS((3,2,2,2,3),(0.625,0.65625,0.6875,0.71875,0.75),
 .UNSPECIFIED.)
CURVE()
GEOMETRIC_REPRESENTATION_ITEM()
RATIONAL_B_SPLINE_CURVE((1.,0.923879532511287,1.,0.923879532511287,1.,0.923879532511287,
1.,0.923879532511287,1.))
REPRESENTATION_ITEM('')
);
#1963=(
BOUNDED_CURVE()
B_SPLINE_CURVE(2,(#41631,#41632,#41633,#41634,#41635,#41636,#41637,#41638,
#41639),.UNSPECIFIED.,.F.,.F.)
B_SPLINE_CURVE_WITH_KNOTS((3,2,2,2,3),(0.75,0.78125,0.8125,0.84375,0.875),
 .UNSPECIFIED.)
CURVE()
GEOMETRIC_REPRESENTATION_ITEM()
RATIONAL_B_SPLINE_CURVE((1.,0.923879532511287,1.,0.923879532511287,1.,0.923879532511287,
1.,0.923879532511287,1.))
REPRESENTATION_ITEM('')
);
#1964=(
BOUNDED_CURVE()
B_SPLINE_CURVE(2,(#41641,#41642,#41643,#41644,#41645,#41646,#41647,#41648,
#41649),.UNSPECIFIED.,.F.,.F.)
B_SPLINE_CURVE_WITH_KNOTS((3,2,2,2,3),(0.875,0.90625,0.9375,0.96875,1.),
 .UNSPECIFIED.)
CURVE()
GEOMETRIC_REPRESENTATION_ITEM()
RATIONAL_B_SPLINE_CURVE((1.,0.923879532511287,1.,0.923879532511287,1.,0.923879532511287,
1.,0.923879532511287,1.))
REPRESENTATION_ITEM('')
);
#1965=(
BOUNDED_CURVE()
B_SPLINE_CURVE(2,(#41653,#41654,#41655,#41656,#41657,#41658,#41659,#41660,
#41661,#41662,#41663,#41664,#41665,#41666,#41667,#41668,#41669,#41670,#41671,
#41672,#41673,#41674,#41675,#41676,#41677,#41678,#41679,#41680,#41681,#41682,
#41683,#41684,#41685,#41686,#41687,#41688,#41689,#41690,#41691,#41692,#41693,
#41694,#41695,#41696,#41697,#41698,#41699,#41700,#41701,#41702,#41703,#41704,
#41705,#41706,#41707,#41708,#41709,#41710,#41711,#41712,#41713,#41714,#41715,
#41716,#41717),.UNSPECIFIED.,.F.,.F.)
B_SPLINE_CURVE_WITH_KNOTS((3,2,2,2,2,2,2,2,2,2,2,2,2,2,2,2,2,2,2,2,2,2,
2,2,2,2,2,2,2,2,2,2,3),(0.,0.03125,0.0625,0.09375,0.125,0.15625,0.1875,
0.21875,0.25,0.28125,0.3125,0.34375,0.375,0.40625,0.4375,0.46875,0.5,0.53125,
0.5625,0.59375,0.625,0.65625,0.6875,0.71875,0.75,0.78125,0.8125,0.84375,
0.875,0.90625,0.9375,0.96875,1.),.UNSPECIFIED.)
CURVE()
GEOMETRIC_REPRESENTATION_ITEM()
RATIONAL_B_SPLINE_CURVE((1.,0.923879532511287,1.,0.923879532511287,1.,0.923879532511287,
1.,0.923879532511287,1.,0.923879532511287,1.,0.923879532511287,1.,0.923879532511287,
1.,0.923879532511287,1.,0.923879532511287,1.,0.923879532511287,1.,0.923879532511287,
1.,0.923879532511287,1.,0.923879532511287,1.,0.923879532511287,1.,0.923879532511287,
1.,0.923879532511287,1.,0.923879532511287,1.,0.923879532511287,1.,0.923879532511287,
1.,0.923879532511287,1.,0.923879532511287,1.,0.923879532511287,1.,0.923879532511287,
1.,0.923879532511287,1.,0.923879532511287,1.,0.923879532511287,1.,0.923879532511287,
1.,0.923879532511287,1.,0.923879532511287,1.,0.923879532511287,1.,0.923879532511287,
1.,0.923879532511287,1.))
REPRESENTATION_ITEM('')
);
#1966=ORIENTED_EDGE('',*,*,#5630,.T.);
#1967=ORIENTED_EDGE('',*,*,#5631,.T.);
#1968=ORIENTED_EDGE('',*,*,#5632,.T.);
#1969=ORIENTED_EDGE('',*,*,#5633,.T.);
#1970=ORIENTED_EDGE('',*,*,#5634,.T.);
#1971=ORIENTED_EDGE('',*,*,#5635,.T.);
#1972=ORIENTED_EDGE('',*,*,#5636,.T.);
#1973=ORIENTED_EDGE('',*,*,#5637,.T.);
#1974=ORIENTED_EDGE('',*,*,#5638,.T.);
#1975=ORIENTED_EDGE('',*,*,#5639,.F.);
#1976=ORIENTED_EDGE('',*,*,#5640,.T.);
#1977=ORIENTED_EDGE('',*,*,#5639,.T.);
#1978=ORIENTED_EDGE('',*,*,#5641,.T.);
#1979=ORIENTED_EDGE('',*,*,#5642,.F.);
#1980=ORIENTED_EDGE('',*,*,#5641,.F.);
#1981=ORIENTED_EDGE('',*,*,#5638,.F.);
#1982=ORIENTED_EDGE('',*,*,#5643,.F.);
#1983=ORIENTED_EDGE('',*,*,#5644,.F.);
#1984=ORIENTED_EDGE('',*,*,#5645,.T.);
#1985=ORIENTED_EDGE('',*,*,#5646,.T.);
#1986=ORIENTED_EDGE('',*,*,#5642,.T.);
#1987=ORIENTED_EDGE('',*,*,#5644,.T.);
#1988=ORIENTED_EDGE('',*,*,#5647,.F.);
#1989=ORIENTED_EDGE('',*,*,#5648,.F.);
#1990=ORIENTED_EDGE('',*,*,#5649,.F.);
#1991=ORIENTED_EDGE('',*,*,#5650,.F.);
#1992=ORIENTED_EDGE('',*,*,#5651,.F.);
#1993=ORIENTED_EDGE('',*,*,#5652,.F.);
#1994=ORIENTED_EDGE('',*,*,#5653,.F.);
#1995=ORIENTED_EDGE('',*,*,#5654,.F.);
#1996=ORIENTED_EDGE('',*,*,#5630,.F.);
#1997=ORIENTED_EDGE('',*,*,#5640,.F.);
#1998=ORIENTED_EDGE('',*,*,#5646,.F.);
#1999=ORIENTED_EDGE('',*,*,#5655,.F.);
#2000=ORIENTED_EDGE('',*,*,#5656,.T.);
#2001=ORIENTED_EDGE('',*,*,#5657,.F.);
#2002=ORIENTED_EDGE('',*,*,#5655,.T.);
#2003=ORIENTED_EDGE('',*,*,#5645,.F.);
#2004=ORIENTED_EDGE('',*,*,#5658,.F.);
#2005=ORIENTED_EDGE('',*,*,#5659,.T.);
#2006=ORIENTED_EDGE('',*,*,#5660,.T.);
#2007=ORIENTED_EDGE('',*,*,#5661,.F.);
#2008=ORIENTED_EDGE('',*,*,#5662,.T.);
#2009=ORIENTED_EDGE('',*,*,#5661,.T.);
#2010=ORIENTED_EDGE('',*,*,#5663,.T.);
#2011=ORIENTED_EDGE('',*,*,#5664,.T.);
#2012=ORIENTED_EDGE('',*,*,#5665,.T.);
#2013=ORIENTED_EDGE('',*,*,#5666,.T.);
#2014=ORIENTED_EDGE('',*,*,#5667,.F.);
#2015=ORIENTED_EDGE('',*,*,#5668,.F.);
#2016=ORIENTED_EDGE('',*,*,#5669,.T.);
#2017=ORIENTED_EDGE('',*,*,#5670,.T.);
#2018=ORIENTED_EDGE('',*,*,#5671,.F.);
#2019=ORIENTED_EDGE('',*,*,#5672,.F.);
#2020=ORIENTED_EDGE('',*,*,#5673,.T.);
#2021=ORIENTED_EDGE('',*,*,#5674,.T.);
#2022=ORIENTED_EDGE('',*,*,#5669,.F.);
#2023=ORIENTED_EDGE('',*,*,#5675,.F.);
#2024=ORIENTED_EDGE('',*,*,#5671,.T.);
#2025=ORIENTED_EDGE('',*,*,#5676,.T.);
#2026=ORIENTED_EDGE('',*,*,#5677,.F.);
#2027=ORIENTED_EDGE('',*,*,#5678,.F.);
#2028=ORIENTED_EDGE('',*,*,#5679,.T.);
#2029=ORIENTED_EDGE('',*,*,#5680,.T.);
#2030=ORIENTED_EDGE('',*,*,#5681,.F.);
#2031=ORIENTED_EDGE('',*,*,#5682,.F.);
#2032=ORIENTED_EDGE('',*,*,#5683,.T.);
#2033=ORIENTED_EDGE('',*,*,#5684,.T.);
#2034=ORIENTED_EDGE('',*,*,#5679,.F.);
#2035=ORIENTED_EDGE('',*,*,#5685,.F.);
#2036=ORIENTED_EDGE('',*,*,#5681,.T.);
#2037=ORIENTED_EDGE('',*,*,#5686,.T.);
#2038=ORIENTED_EDGE('',*,*,#5687,.F.);
#2039=ORIENTED_EDGE('',*,*,#5688,.F.);
#2040=ORIENTED_EDGE('',*,*,#5689,.T.);
#2041=ORIENTED_EDGE('',*,*,#5690,.T.);
#2042=ORIENTED_EDGE('',*,*,#5691,.F.);
#2043=ORIENTED_EDGE('',*,*,#5692,.F.);
#2044=ORIENTED_EDGE('',*,*,#5693,.T.);
#2045=ORIENTED_EDGE('',*,*,#5694,.T.);
#2046=ORIENTED_EDGE('',*,*,#5689,.F.);
#2047=ORIENTED_EDGE('',*,*,#5695,.F.);
#2048=ORIENTED_EDGE('',*,*,#5691,.T.);
#2049=ORIENTED_EDGE('',*,*,#5696,.T.);
#2050=ORIENTED_EDGE('',*,*,#5697,.F.);
#2051=ORIENTED_EDGE('',*,*,#5698,.T.);
#2052=ORIENTED_EDGE('',*,*,#5699,.F.);
#2053=ORIENTED_EDGE('',*,*,#5700,.T.);
#2054=ORIENTED_EDGE('',*,*,#5701,.F.);
#2055=ORIENTED_EDGE('',*,*,#5702,.T.);
#2056=ORIENTED_EDGE('',*,*,#5703,.F.);
#2057=ORIENTED_EDGE('',*,*,#5704,.T.);
#2058=ORIENTED_EDGE('',*,*,#5705,.T.);
#2059=ORIENTED_EDGE('',*,*,#5706,.T.);
#2060=ORIENTED_EDGE('',*,*,#5707,.T.);
#2061=ORIENTED_EDGE('',*,*,#5708,.F.);
#2062=ORIENTED_EDGE('',*,*,#5709,.T.);
#2063=ORIENTED_EDGE('',*,*,#5710,.T.);
#2064=ORIENTED_EDGE('',*,*,#5711,.T.);
#2065=ORIENTED_EDGE('',*,*,#5712,.T.);
#2066=ORIENTED_EDGE('',*,*,#5692,.T.);
#2067=ORIENTED_EDGE('',*,*,#5695,.T.);
#2068=ORIENTED_EDGE('',*,*,#5688,.T.);
#2069=ORIENTED_EDGE('',*,*,#5713,.T.);
#2070=ORIENTED_EDGE('',*,*,#5682,.T.);
#2071=ORIENTED_EDGE('',*,*,#5685,.T.);
#2072=ORIENTED_EDGE('',*,*,#5678,.T.);
#2073=ORIENTED_EDGE('',*,*,#5714,.T.);
#2074=ORIENTED_EDGE('',*,*,#5672,.T.);
#2075=ORIENTED_EDGE('',*,*,#5675,.T.);
#2076=ORIENTED_EDGE('',*,*,#5668,.T.);
#2077=ORIENTED_EDGE('',*,*,#5715,.T.);
#2078=ORIENTED_EDGE('',*,*,#5716,.F.);
#2079=ORIENTED_EDGE('',*,*,#5717,.F.);
#2080=ORIENTED_EDGE('',*,*,#5718,.F.);
#2081=ORIENTED_EDGE('',*,*,#5719,.T.);
#2082=ORIENTED_EDGE('',*,*,#5720,.T.);
#2083=ORIENTED_EDGE('',*,*,#5721,.F.);
#2084=ORIENTED_EDGE('',*,*,#5722,.F.);
#2085=ORIENTED_EDGE('',*,*,#5723,.F.);
#2086=ORIENTED_EDGE('',*,*,#5724,.F.);
#2087=ORIENTED_EDGE('',*,*,#5725,.F.);
#2088=ORIENTED_EDGE('',*,*,#5694,.F.);
#2089=ORIENTED_EDGE('',*,*,#5690,.F.);
#2090=ORIENTED_EDGE('',*,*,#5726,.F.);
#2091=ORIENTED_EDGE('',*,*,#5686,.F.);
#2092=ORIENTED_EDGE('',*,*,#5684,.F.);
#2093=ORIENTED_EDGE('',*,*,#5680,.F.);
#2094=ORIENTED_EDGE('',*,*,#5727,.F.);
#2095=ORIENTED_EDGE('',*,*,#5676,.F.);
#2096=ORIENTED_EDGE('',*,*,#5674,.F.);
#2097=ORIENTED_EDGE('',*,*,#5670,.F.);
#2098=ORIENTED_EDGE('',*,*,#5728,.F.);
#2099=ORIENTED_EDGE('',*,*,#5666,.F.);
#2100=ORIENTED_EDGE('',*,*,#5729,.T.);
#2101=ORIENTED_EDGE('',*,*,#5730,.T.);
#2102=ORIENTED_EDGE('',*,*,#5731,.F.);
#2103=ORIENTED_EDGE('',*,*,#5732,.F.);
#2104=ORIENTED_EDGE('',*,*,#5733,.T.);
#2105=ORIENTED_EDGE('',*,*,#5663,.F.);
#2106=ORIENTED_EDGE('',*,*,#5734,.T.);
#2107=ORIENTED_EDGE('',*,*,#5664,.F.);
#2108=ORIENTED_EDGE('',*,*,#5656,.F.);
#2109=ORIENTED_EDGE('',*,*,#5707,.F.);
#2110=ORIENTED_EDGE('',*,*,#5732,.T.);
#2111=ORIENTED_EDGE('',*,*,#5730,.F.);
#2112=ORIENTED_EDGE('',*,*,#5720,.F.);
#2113=ORIENTED_EDGE('',*,*,#5708,.T.);
#2114=ORIENTED_EDGE('',*,*,#5719,.F.);
#2115=ORIENTED_EDGE('',*,*,#5706,.F.);
#2116=ORIENTED_EDGE('',*,*,#5718,.T.);
#2117=ORIENTED_EDGE('',*,*,#5705,.F.);
#2118=ORIENTED_EDGE('',*,*,#5721,.T.);
#2119=ORIENTED_EDGE('',*,*,#5704,.F.);
#2120=ORIENTED_EDGE('',*,*,#5717,.T.);
#2121=ORIENTED_EDGE('',*,*,#5703,.T.);
#2122=ORIENTED_EDGE('',*,*,#5709,.F.);
#2123=ORIENTED_EDGE('',*,*,#5722,.T.);
#2124=ORIENTED_EDGE('',*,*,#5702,.F.);
#2125=ORIENTED_EDGE('',*,*,#5701,.T.);
#2126=ORIENTED_EDGE('',*,*,#5710,.F.);
#2127=ORIENTED_EDGE('',*,*,#5723,.T.);
#2128=ORIENTED_EDGE('',*,*,#5700,.F.);
#2129=ORIENTED_EDGE('',*,*,#5699,.T.);
#2130=ORIENTED_EDGE('',*,*,#5711,.F.);
#2131=ORIENTED_EDGE('',*,*,#5724,.T.);
#2132=ORIENTED_EDGE('',*,*,#5698,.F.);
#2133=ORIENTED_EDGE('',*,*,#5697,.T.);
#2134=ORIENTED_EDGE('',*,*,#5712,.F.);
#2135=ORIENTED_EDGE('',*,*,#5725,.T.);
#2136=ORIENTED_EDGE('',*,*,#5696,.F.);
#2137=ORIENTED_EDGE('',*,*,#5713,.F.);
#2138=ORIENTED_EDGE('',*,*,#5687,.T.);
#2139=ORIENTED_EDGE('',*,*,#5726,.T.);
#2140=ORIENTED_EDGE('',*,*,#5693,.F.);
#2141=ORIENTED_EDGE('',*,*,#5714,.F.);
#2142=ORIENTED_EDGE('',*,*,#5677,.T.);
#2143=ORIENTED_EDGE('',*,*,#5727,.T.);
#2144=ORIENTED_EDGE('',*,*,#5683,.F.);
#2145=ORIENTED_EDGE('',*,*,#5715,.F.);
#2146=ORIENTED_EDGE('',*,*,#5667,.T.);
#2147=ORIENTED_EDGE('',*,*,#5728,.T.);
#2148=ORIENTED_EDGE('',*,*,#5673,.F.);
#2149=ORIENTED_EDGE('',*,*,#5716,.T.);
#2150=ORIENTED_EDGE('',*,*,#5729,.F.);
#2151=ORIENTED_EDGE('',*,*,#5731,.T.);
#2152=ORIENTED_EDGE('',*,*,#5665,.F.);
#2153=ORIENTED_EDGE('',*,*,#5643,.T.);
#2154=ORIENTED_EDGE('',*,*,#5637,.F.);
#2155=ORIENTED_EDGE('',*,*,#5636,.F.);
#2156=ORIENTED_EDGE('',*,*,#5635,.F.);
#2157=ORIENTED_EDGE('',*,*,#5634,.F.);
#2158=ORIENTED_EDGE('',*,*,#5633,.F.);
#2159=ORIENTED_EDGE('',*,*,#5632,.F.);
#2160=ORIENTED_EDGE('',*,*,#5631,.F.);
#2161=ORIENTED_EDGE('',*,*,#5654,.T.);
#2162=ORIENTED_EDGE('',*,*,#5657,.T.);
#2163=ORIENTED_EDGE('',*,*,#5653,.T.);
#2164=ORIENTED_EDGE('',*,*,#5652,.T.);
#2165=ORIENTED_EDGE('',*,*,#5651,.T.);
#2166=ORIENTED_EDGE('',*,*,#5650,.T.);
#2167=ORIENTED_EDGE('',*,*,#5649,.T.);
#2168=ORIENTED_EDGE('',*,*,#5648,.T.);
#2169=ORIENTED_EDGE('',*,*,#5647,.T.);
#2170=ORIENTED_EDGE('',*,*,#5735,.F.);
#2171=ORIENTED_EDGE('',*,*,#5659,.F.);
#2172=ORIENTED_EDGE('',*,*,#5733,.F.);
#2173=ORIENTED_EDGE('',*,*,#5734,.F.);
#2174=ORIENTED_EDGE('',*,*,#5735,.T.);
#2175=ORIENTED_EDGE('',*,*,#5658,.T.);
#2176=ORIENTED_EDGE('',*,*,#5662,.F.);
#2177=ORIENTED_EDGE('',*,*,#5660,.F.);
#2178=ORIENTED_EDGE('',*,*,#5736,.F.);
#2179=ORIENTED_EDGE('',*,*,#5737,.T.);
#2180=ORIENTED_EDGE('',*,*,#5738,.F.);
#2181=ORIENTED_EDGE('',*,*,#5739,.T.);
#2182=ORIENTED_EDGE('',*,*,#5740,.F.);
#2183=ORIENTED_EDGE('',*,*,#5741,.T.);
#2184=ORIENTED_EDGE('',*,*,#5742,.F.);
#2185=ORIENTED_EDGE('',*,*,#5743,.T.);
#2186=ORIENTED_EDGE('',*,*,#5744,.T.);
#2187=ORIENTED_EDGE('',*,*,#5745,.F.);
#2188=ORIENTED_EDGE('',*,*,#5746,.F.);
#2189=ORIENTED_EDGE('',*,*,#5747,.F.);
#2190=ORIENTED_EDGE('',*,*,#5748,.F.);
#2191=ORIENTED_EDGE('',*,*,#5749,.F.);
#2192=ORIENTED_EDGE('',*,*,#5750,.T.);
#2193=ORIENTED_EDGE('',*,*,#5751,.T.);
#2194=ORIENTED_EDGE('',*,*,#5752,.T.);
#2195=ORIENTED_EDGE('',*,*,#5753,.T.);
#2196=ORIENTED_EDGE('',*,*,#5754,.F.);
#2197=ORIENTED_EDGE('',*,*,#5755,.F.);
#2198=ORIENTED_EDGE('',*,*,#5756,.F.);
#2199=ORIENTED_EDGE('',*,*,#5755,.T.);
#2200=ORIENTED_EDGE('',*,*,#5757,.F.);
#2201=ORIENTED_EDGE('',*,*,#5741,.F.);
#2202=ORIENTED_EDGE('',*,*,#5757,.T.);
#2203=ORIENTED_EDGE('',*,*,#5754,.T.);
#2204=ORIENTED_EDGE('',*,*,#5758,.T.);
#2205=ORIENTED_EDGE('',*,*,#5759,.T.);
#2206=ORIENTED_EDGE('',*,*,#5743,.F.);
#2207=ORIENTED_EDGE('',*,*,#5742,.T.);
#2208=ORIENTED_EDGE('',*,*,#5756,.T.);
#2209=ORIENTED_EDGE('',*,*,#5740,.T.);
#2210=ORIENTED_EDGE('',*,*,#5760,.T.);
#2211=ORIENTED_EDGE('',*,*,#5749,.T.);
#2212=ORIENTED_EDGE('',*,*,#5761,.T.);
#2213=ORIENTED_EDGE('',*,*,#5762,.T.);
#2214=ORIENTED_EDGE('',*,*,#5763,.T.);
#2215=ORIENTED_EDGE('',*,*,#5764,.T.);
#2216=ORIENTED_EDGE('',*,*,#5765,.T.);
#2217=ORIENTED_EDGE('',*,*,#5766,.F.);
#2218=ORIENTED_EDGE('',*,*,#5767,.T.);
#2219=ORIENTED_EDGE('',*,*,#5768,.T.);
#2220=ORIENTED_EDGE('',*,*,#5769,.T.);
#2221=ORIENTED_EDGE('',*,*,#5770,.T.);
#2222=ORIENTED_EDGE('',*,*,#5771,.T.);
#2223=ORIENTED_EDGE('',*,*,#5772,.F.);
#2224=ORIENTED_EDGE('',*,*,#5773,.T.);
#2225=ORIENTED_EDGE('',*,*,#5774,.T.);
#2226=ORIENTED_EDGE('',*,*,#5775,.T.);
#2227=ORIENTED_EDGE('',*,*,#5776,.F.);
#2228=ORIENTED_EDGE('',*,*,#5777,.T.);
#2229=ORIENTED_EDGE('',*,*,#5778,.T.);
#2230=ORIENTED_EDGE('',*,*,#5779,.T.);
#2231=ORIENTED_EDGE('',*,*,#5738,.T.);
#2232=ORIENTED_EDGE('',*,*,#5746,.T.);
#2233=ORIENTED_EDGE('',*,*,#5745,.T.);
#2234=ORIENTED_EDGE('',*,*,#5780,.T.);
#2235=ORIENTED_EDGE('',*,*,#5758,.F.);
#2236=ORIENTED_EDGE('',*,*,#5753,.F.);
#2237=ORIENTED_EDGE('',*,*,#5752,.F.);
#2238=ORIENTED_EDGE('',*,*,#5751,.F.);
#2239=ORIENTED_EDGE('',*,*,#5750,.F.);
#2240=ORIENTED_EDGE('',*,*,#5760,.F.);
#2241=ORIENTED_EDGE('',*,*,#5748,.T.);
#2242=ORIENTED_EDGE('',*,*,#5747,.T.);
#2243=ORIENTED_EDGE('',*,*,#5781,.T.);
#2244=ORIENTED_EDGE('',*,*,#5782,.T.);
#2245=ORIENTED_EDGE('',*,*,#5775,.F.);
#2246=ORIENTED_EDGE('',*,*,#5783,.F.);
#2247=ORIENTED_EDGE('',*,*,#5776,.T.);
#2248=ORIENTED_EDGE('',*,*,#5783,.T.);
#2249=ORIENTED_EDGE('',*,*,#5784,.T.);
#2250=ORIENTED_EDGE('',*,*,#5785,.T.);
#2251=ORIENTED_EDGE('',*,*,#5786,.F.);
#2252=ORIENTED_EDGE('',*,*,#5771,.F.);
#2253=ORIENTED_EDGE('',*,*,#5786,.T.);
#2254=ORIENTED_EDGE('',*,*,#5736,.T.);
#2255=ORIENTED_EDGE('',*,*,#5772,.T.);
#2256=ORIENTED_EDGE('',*,*,#5787,.F.);
#2257=ORIENTED_EDGE('',*,*,#5788,.T.);
#2258=ORIENTED_EDGE('',*,*,#5787,.T.);
#2259=ORIENTED_EDGE('',*,*,#5765,.F.);
#2260=ORIENTED_EDGE('',*,*,#5789,.T.);
#2261=ORIENTED_EDGE('',*,*,#5766,.T.);
#2262=ORIENTED_EDGE('',*,*,#5790,.T.);
#2263=ORIENTED_EDGE('',*,*,#5791,.T.);
#2264=ORIENTED_EDGE('',*,*,#5777,.F.);
#2265=ORIENTED_EDGE('',*,*,#5792,.T.);
#2266=ORIENTED_EDGE('',*,*,#5791,.F.);
#2267=ORIENTED_EDGE('',*,*,#5763,.F.);
#2268=ORIENTED_EDGE('',*,*,#5790,.F.);
#2269=ORIENTED_EDGE('',*,*,#5761,.F.);
#2270=ORIENTED_EDGE('',*,*,#5774,.F.);
#2271=ORIENTED_EDGE('',*,*,#5784,.F.);
#2272=ORIENTED_EDGE('',*,*,#5773,.F.);
#2273=ORIENTED_EDGE('',*,*,#5785,.F.);
#2274=ORIENTED_EDGE('',*,*,#5788,.F.);
#2275=ORIENTED_EDGE('',*,*,#5767,.F.);
#2276=ORIENTED_EDGE('',*,*,#5779,.F.);
#2277=ORIENTED_EDGE('',*,*,#5769,.F.);
#2278=ORIENTED_EDGE('',*,*,#5780,.F.);
#2279=ORIENTED_EDGE('',*,*,#5744,.F.);
#2280=ORIENTED_EDGE('',*,*,#5759,.F.);
#2281=ORIENTED_EDGE('',*,*,#5768,.F.);
#2282=ORIENTED_EDGE('',*,*,#5781,.F.);
#2283=ORIENTED_EDGE('',*,*,#5770,.F.);
#2284=ORIENTED_EDGE('',*,*,#5792,.F.);
#2285=ORIENTED_EDGE('',*,*,#5762,.F.);
#2286=ORIENTED_EDGE('',*,*,#5789,.F.);
#2287=ORIENTED_EDGE('',*,*,#5764,.F.);
#2288=ORIENTED_EDGE('',*,*,#5778,.F.);
#2289=ORIENTED_EDGE('',*,*,#5782,.F.);
#2290=ORIENTED_EDGE('',*,*,#5793,.T.);
#2291=ORIENTED_EDGE('',*,*,#5794,.T.);
#2292=ORIENTED_EDGE('',*,*,#5794,.F.);
#2293=ORIENTED_EDGE('',*,*,#5739,.F.);
#2294=ORIENTED_EDGE('',*,*,#5793,.F.);
#2295=ORIENTED_EDGE('',*,*,#5737,.F.);
#2296=ORIENTED_EDGE('',*,*,#5795,.T.);
#2297=ORIENTED_EDGE('',*,*,#5796,.F.);
#2298=ORIENTED_EDGE('',*,*,#5795,.F.);
#2299=ORIENTED_EDGE('',*,*,#5797,.T.);
#2300=ORIENTED_EDGE('',*,*,#5798,.F.);
#2301=ORIENTED_EDGE('',*,*,#5799,.T.);
#2302=ORIENTED_EDGE('',*,*,#5800,.F.);
#2303=ORIENTED_EDGE('',*,*,#5801,.T.);
#2304=ORIENTED_EDGE('',*,*,#5796,.T.);
#2305=ORIENTED_EDGE('',*,*,#5802,.T.);
#2306=ORIENTED_EDGE('',*,*,#5803,.F.);
#2307=ORIENTED_EDGE('',*,*,#5802,.F.);
#2308=ORIENTED_EDGE('',*,*,#5797,.F.);
#2309=ORIENTED_EDGE('',*,*,#5801,.F.);
#2310=ORIENTED_EDGE('',*,*,#5798,.T.);
#2311=ORIENTED_EDGE('',*,*,#5804,.F.);
#2312=ORIENTED_EDGE('',*,*,#5805,.F.);
#2313=ORIENTED_EDGE('',*,*,#5806,.F.);
#2314=ORIENTED_EDGE('',*,*,#5799,.F.);
#2315=ORIENTED_EDGE('',*,*,#5807,.F.);
#2316=ORIENTED_EDGE('',*,*,#5800,.T.);
#2317=ORIENTED_EDGE('',*,*,#5808,.F.);
#2318=ORIENTED_EDGE('',*,*,#5809,.F.);
#2319=ORIENTED_EDGE('',*,*,#5810,.F.);
#2320=ORIENTED_EDGE('',*,*,#5803,.T.);
#2321=ORIENTED_EDGE('',*,*,#5810,.T.);
#2322=ORIENTED_EDGE('',*,*,#5811,.F.);
#2323=ORIENTED_EDGE('',*,*,#5808,.T.);
#2324=ORIENTED_EDGE('',*,*,#5812,.F.);
#2325=ORIENTED_EDGE('',*,*,#5807,.T.);
#2326=ORIENTED_EDGE('',*,*,#5804,.T.);
#2327=ORIENTED_EDGE('',*,*,#5806,.T.);
#2328=ORIENTED_EDGE('',*,*,#5805,.T.);
#2329=ORIENTED_EDGE('',*,*,#5813,.T.);
#2330=ORIENTED_EDGE('',*,*,#5814,.F.);
#2331=ORIENTED_EDGE('',*,*,#5815,.T.);
#2332=ORIENTED_EDGE('',*,*,#5816,.T.);
#2333=ORIENTED_EDGE('',*,*,#5809,.T.);
#2334=ORIENTED_EDGE('',*,*,#5817,.T.);
#2335=ORIENTED_EDGE('',*,*,#5818,.F.);
#2336=ORIENTED_EDGE('',*,*,#5816,.F.);
#2337=ORIENTED_EDGE('',*,*,#5819,.F.);
#2338=ORIENTED_EDGE('',*,*,#5817,.F.);
#2339=ORIENTED_EDGE('',*,*,#5811,.T.);
#2340=ORIENTED_EDGE('',*,*,#5812,.T.);
#2341=ORIENTED_EDGE('',*,*,#5815,.F.);
#2342=ORIENTED_EDGE('',*,*,#5820,.F.);
#2343=ORIENTED_EDGE('',*,*,#5813,.F.);
#2344=ORIENTED_EDGE('',*,*,#5821,.F.);
#2345=ORIENTED_EDGE('',*,*,#5818,.T.);
#2346=ORIENTED_EDGE('',*,*,#5822,.F.);
#2347=ORIENTED_EDGE('',*,*,#5814,.T.);
#2348=ORIENTED_EDGE('',*,*,#5821,.T.);
#2349=ORIENTED_EDGE('',*,*,#5820,.T.);
#2350=ORIENTED_EDGE('',*,*,#5822,.T.);
#2351=ORIENTED_EDGE('',*,*,#5819,.T.);
#2352=ORIENTED_EDGE('',*,*,#5823,.F.);
#2353=ORIENTED_EDGE('',*,*,#5824,.T.);
#2354=ORIENTED_EDGE('',*,*,#5825,.T.);
#2355=ORIENTED_EDGE('',*,*,#5826,.T.);
#2356=ORIENTED_EDGE('',*,*,#5827,.T.);
#2357=ORIENTED_EDGE('',*,*,#5828,.T.);
#2358=ORIENTED_EDGE('',*,*,#5829,.T.);
#2359=ORIENTED_EDGE('',*,*,#5830,.F.);
#2360=ORIENTED_EDGE('',*,*,#5831,.T.);
#2361=ORIENTED_EDGE('',*,*,#5823,.T.);
#2362=ORIENTED_EDGE('',*,*,#5832,.T.);
#2363=ORIENTED_EDGE('',*,*,#5833,.F.);
#2364=ORIENTED_EDGE('',*,*,#5834,.T.);
#2365=ORIENTED_EDGE('',*,*,#5830,.T.);
#2366=ORIENTED_EDGE('',*,*,#5835,.T.);
#2367=ORIENTED_EDGE('',*,*,#5836,.F.);
#2368=ORIENTED_EDGE('',*,*,#5837,.T.);
#2369=ORIENTED_EDGE('',*,*,#5833,.T.);
#2370=ORIENTED_EDGE('',*,*,#5838,.T.);
#2371=ORIENTED_EDGE('',*,*,#5839,.F.);
#2372=ORIENTED_EDGE('',*,*,#5840,.T.);
#2373=ORIENTED_EDGE('',*,*,#5836,.T.);
#2374=ORIENTED_EDGE('',*,*,#5841,.T.);
#2375=ORIENTED_EDGE('',*,*,#5842,.F.);
#2376=ORIENTED_EDGE('',*,*,#5843,.T.);
#2377=ORIENTED_EDGE('',*,*,#5839,.T.);
#2378=ORIENTED_EDGE('',*,*,#5844,.T.);
#2379=ORIENTED_EDGE('',*,*,#5845,.F.);
#2380=ORIENTED_EDGE('',*,*,#5846,.T.);
#2381=ORIENTED_EDGE('',*,*,#5842,.T.);
#2382=ORIENTED_EDGE('',*,*,#5847,.T.);
#2383=ORIENTED_EDGE('',*,*,#5848,.F.);
#2384=ORIENTED_EDGE('',*,*,#5849,.F.);
#2385=ORIENTED_EDGE('',*,*,#5850,.F.);
#2386=ORIENTED_EDGE('',*,*,#5851,.F.);
#2387=ORIENTED_EDGE('',*,*,#5829,.F.);
#2388=ORIENTED_EDGE('',*,*,#5852,.F.);
#2389=ORIENTED_EDGE('',*,*,#5847,.F.);
#2390=ORIENTED_EDGE('',*,*,#5844,.F.);
#2391=ORIENTED_EDGE('',*,*,#5841,.F.);
#2392=ORIENTED_EDGE('',*,*,#5838,.F.);
#2393=ORIENTED_EDGE('',*,*,#5835,.F.);
#2394=ORIENTED_EDGE('',*,*,#5832,.F.);
#2395=ORIENTED_EDGE('',*,*,#5853,.T.);
#2396=ORIENTED_EDGE('',*,*,#5824,.F.);
#2397=ORIENTED_EDGE('',*,*,#5831,.F.);
#2398=ORIENTED_EDGE('',*,*,#5834,.F.);
#2399=ORIENTED_EDGE('',*,*,#5837,.F.);
#2400=ORIENTED_EDGE('',*,*,#5840,.F.);
#2401=ORIENTED_EDGE('',*,*,#5843,.F.);
#2402=ORIENTED_EDGE('',*,*,#5846,.F.);
#2403=ORIENTED_EDGE('',*,*,#5854,.F.);
#2404=ORIENTED_EDGE('',*,*,#5826,.F.);
#2405=ORIENTED_EDGE('',*,*,#5825,.F.);
#2406=ORIENTED_EDGE('',*,*,#5853,.F.);
#2407=ORIENTED_EDGE('',*,*,#5845,.T.);
#2408=ORIENTED_EDGE('',*,*,#5851,.T.);
#2409=ORIENTED_EDGE('',*,*,#5850,.T.);
#2410=ORIENTED_EDGE('',*,*,#5849,.T.);
#2411=ORIENTED_EDGE('',*,*,#5848,.T.);
#2412=ORIENTED_EDGE('',*,*,#5852,.T.);
#2413=ORIENTED_EDGE('',*,*,#5828,.F.);
#2414=ORIENTED_EDGE('',*,*,#5827,.F.);
#2415=ORIENTED_EDGE('',*,*,#5854,.T.);
#2416=ORIENTED_EDGE('',*,*,#5855,.F.);
#2417=ORIENTED_EDGE('',*,*,#5856,.T.);
#2418=ORIENTED_EDGE('',*,*,#5856,.F.);
#2419=ORIENTED_EDGE('',*,*,#5855,.T.);
#2420=ORIENTED_EDGE('',*,*,#5857,.T.);
#2421=ORIENTED_EDGE('',*,*,#5858,.F.);
#2422=ORIENTED_EDGE('',*,*,#5859,.T.);
#2423=ORIENTED_EDGE('',*,*,#5860,.F.);
#2424=ORIENTED_EDGE('',*,*,#5861,.T.);
#2425=ORIENTED_EDGE('',*,*,#5862,.F.);
#2426=ORIENTED_EDGE('',*,*,#5859,.F.);
#2427=ORIENTED_EDGE('',*,*,#5863,.F.);
#2428=ORIENTED_EDGE('',*,*,#5864,.T.);
#2429=ORIENTED_EDGE('',*,*,#5865,.T.);
#2430=ORIENTED_EDGE('',*,*,#5857,.F.);
#2431=ORIENTED_EDGE('',*,*,#5866,.T.);
#2432=ORIENTED_EDGE('',*,*,#5867,.T.);
#2433=ORIENTED_EDGE('',*,*,#5868,.T.);
#2434=ORIENTED_EDGE('',*,*,#5861,.F.);
#2435=ORIENTED_EDGE('',*,*,#5869,.T.);
#2436=ORIENTED_EDGE('',*,*,#5870,.T.);
#2437=ORIENTED_EDGE('',*,*,#5871,.F.);
#2438=ORIENTED_EDGE('',*,*,#5866,.F.);
#2439=ORIENTED_EDGE('',*,*,#5872,.F.);
#2440=ORIENTED_EDGE('',*,*,#5873,.T.);
#2441=ORIENTED_EDGE('',*,*,#5874,.F.);
#2442=ORIENTED_EDGE('',*,*,#5867,.F.);
#2443=ORIENTED_EDGE('',*,*,#5875,.F.);
#2444=ORIENTED_EDGE('',*,*,#5876,.T.);
#2445=ORIENTED_EDGE('',*,*,#5877,.F.);
#2446=ORIENTED_EDGE('',*,*,#5868,.F.);
#2447=ORIENTED_EDGE('',*,*,#5878,.F.);
#2448=ORIENTED_EDGE('',*,*,#5879,.T.);
#2449=ORIENTED_EDGE('',*,*,#5880,.T.);
#2450=ORIENTED_EDGE('',*,*,#5870,.F.);
#2451=ORIENTED_EDGE('',*,*,#5881,.T.);
#2452=ORIENTED_EDGE('',*,*,#5882,.T.);
#2453=ORIENTED_EDGE('',*,*,#5883,.T.);
#2454=ORIENTED_EDGE('',*,*,#5884,.F.);
#2455=ORIENTED_EDGE('',*,*,#5885,.T.);
#2456=ORIENTED_EDGE('',*,*,#5886,.T.);
#2457=ORIENTED_EDGE('',*,*,#5887,.T.);
#2458=ORIENTED_EDGE('',*,*,#5873,.F.);
#2459=ORIENTED_EDGE('',*,*,#5888,.T.);
#2460=ORIENTED_EDGE('',*,*,#5889,.T.);
#2461=ORIENTED_EDGE('',*,*,#5890,.T.);
#2462=ORIENTED_EDGE('',*,*,#5876,.F.);
#2463=ORIENTED_EDGE('',*,*,#5891,.T.);
#2464=ORIENTED_EDGE('',*,*,#5892,.T.);
#2465=ORIENTED_EDGE('',*,*,#5893,.F.);
#2466=ORIENTED_EDGE('',*,*,#5881,.F.);
#2467=ORIENTED_EDGE('',*,*,#5894,.F.);
#2468=ORIENTED_EDGE('',*,*,#5895,.T.);
#2469=ORIENTED_EDGE('',*,*,#5896,.F.);
#2470=ORIENTED_EDGE('',*,*,#5885,.F.);
#2471=ORIENTED_EDGE('',*,*,#5897,.F.);
#2472=ORIENTED_EDGE('',*,*,#5898,.T.);
#2473=ORIENTED_EDGE('',*,*,#5899,.F.);
#2474=ORIENTED_EDGE('',*,*,#5882,.F.);
#2475=ORIENTED_EDGE('',*,*,#5900,.F.);
#2476=ORIENTED_EDGE('',*,*,#5901,.T.);
#2477=ORIENTED_EDGE('',*,*,#5902,.F.);
#2478=ORIENTED_EDGE('',*,*,#5886,.F.);
#2479=ORIENTED_EDGE('',*,*,#5903,.F.);
#2480=ORIENTED_EDGE('',*,*,#5904,.T.);
#2481=ORIENTED_EDGE('',*,*,#5905,.F.);
#2482=ORIENTED_EDGE('',*,*,#5887,.F.);
#2483=ORIENTED_EDGE('',*,*,#5906,.F.);
#2484=ORIENTED_EDGE('',*,*,#5907,.T.);
#2485=ORIENTED_EDGE('',*,*,#5908,.F.);
#2486=ORIENTED_EDGE('',*,*,#5891,.F.);
#2487=ORIENTED_EDGE('',*,*,#5909,.F.);
#2488=ORIENTED_EDGE('',*,*,#5890,.F.);
#2489=ORIENTED_EDGE('',*,*,#5910,.F.);
#2490=ORIENTED_EDGE('',*,*,#5892,.F.);
#2491=ORIENTED_EDGE('',*,*,#5911,.F.);
#2492=ORIENTED_EDGE('',*,*,#5912,.T.);
#2493=ORIENTED_EDGE('',*,*,#5913,.T.);
#2494=ORIENTED_EDGE('',*,*,#5895,.F.);
#2495=ORIENTED_EDGE('',*,*,#5914,.F.);
#2496=ORIENTED_EDGE('',*,*,#5915,.T.);
#2497=ORIENTED_EDGE('',*,*,#5916,.T.);
#2498=ORIENTED_EDGE('',*,*,#5898,.F.);
#2499=ORIENTED_EDGE('',*,*,#5917,.T.);
#2500=ORIENTED_EDGE('',*,*,#5918,.T.);
#2501=ORIENTED_EDGE('',*,*,#5919,.T.);
#2502=ORIENTED_EDGE('',*,*,#5901,.F.);
#2503=ORIENTED_EDGE('',*,*,#5920,.T.);
#2504=ORIENTED_EDGE('',*,*,#5921,.T.);
#2505=ORIENTED_EDGE('',*,*,#5922,.T.);
#2506=ORIENTED_EDGE('',*,*,#5907,.F.);
#2507=ORIENTED_EDGE('',*,*,#5904,.F.);
#2508=ORIENTED_EDGE('',*,*,#5923,.T.);
#2509=ORIENTED_EDGE('',*,*,#5924,.F.);
#2510=ORIENTED_EDGE('',*,*,#5913,.F.);
#2511=ORIENTED_EDGE('',*,*,#5925,.F.);
#2512=ORIENTED_EDGE('',*,*,#5926,.T.);
#2513=ORIENTED_EDGE('',*,*,#5927,.F.);
#2514=ORIENTED_EDGE('',*,*,#5917,.F.);
#2515=ORIENTED_EDGE('',*,*,#5928,.F.);
#2516=ORIENTED_EDGE('',*,*,#5929,.T.);
#2517=ORIENTED_EDGE('',*,*,#5930,.F.);
#2518=ORIENTED_EDGE('',*,*,#5915,.F.);
#2519=ORIENTED_EDGE('',*,*,#5931,.F.);
#2520=ORIENTED_EDGE('',*,*,#5932,.T.);
#2521=ORIENTED_EDGE('',*,*,#5933,.F.);
#2522=ORIENTED_EDGE('',*,*,#5918,.F.);
#2523=ORIENTED_EDGE('',*,*,#5934,.F.);
#2524=ORIENTED_EDGE('',*,*,#5935,.T.);
#2525=ORIENTED_EDGE('',*,*,#5936,.F.);
#2526=ORIENTED_EDGE('',*,*,#5919,.F.);
#2527=ORIENTED_EDGE('',*,*,#5937,.F.);
#2528=ORIENTED_EDGE('',*,*,#5938,.T.);
#2529=ORIENTED_EDGE('',*,*,#5939,.F.);
#2530=ORIENTED_EDGE('',*,*,#5921,.F.);
#2531=ORIENTED_EDGE('',*,*,#5940,.F.);
#2532=ORIENTED_EDGE('',*,*,#5941,.T.);
#2533=ORIENTED_EDGE('',*,*,#5942,.T.);
#2534=ORIENTED_EDGE('',*,*,#5926,.F.);
#2535=ORIENTED_EDGE('',*,*,#5923,.F.);
#2536=ORIENTED_EDGE('',*,*,#5943,.T.);
#2537=ORIENTED_EDGE('',*,*,#5944,.T.);
#2538=ORIENTED_EDGE('',*,*,#5929,.F.);
#2539=ORIENTED_EDGE('',*,*,#5945,.T.);
#2540=ORIENTED_EDGE('',*,*,#5946,.T.);
#2541=ORIENTED_EDGE('',*,*,#5947,.T.);
#2542=ORIENTED_EDGE('',*,*,#5932,.F.);
#2543=ORIENTED_EDGE('',*,*,#5948,.T.);
#2544=ORIENTED_EDGE('',*,*,#5949,.T.);
#2545=ORIENTED_EDGE('',*,*,#5950,.T.);
#2546=ORIENTED_EDGE('',*,*,#5938,.F.);
#2547=ORIENTED_EDGE('',*,*,#5935,.F.);
#2548=ORIENTED_EDGE('',*,*,#5951,.T.);
#2549=ORIENTED_EDGE('',*,*,#5952,.F.);
#2550=ORIENTED_EDGE('',*,*,#5942,.F.);
#2551=ORIENTED_EDGE('',*,*,#5953,.F.);
#2552=ORIENTED_EDGE('',*,*,#5954,.T.);
#2553=ORIENTED_EDGE('',*,*,#5955,.F.);
#2554=ORIENTED_EDGE('',*,*,#5945,.F.);
#2555=ORIENTED_EDGE('',*,*,#5956,.F.);
#2556=ORIENTED_EDGE('',*,*,#5957,.T.);
#2557=ORIENTED_EDGE('',*,*,#5958,.F.);
#2558=ORIENTED_EDGE('',*,*,#5943,.F.);
#2559=ORIENTED_EDGE('',*,*,#5959,.F.);
#2560=ORIENTED_EDGE('',*,*,#5960,.T.);
#2561=ORIENTED_EDGE('',*,*,#5961,.F.);
#2562=ORIENTED_EDGE('',*,*,#5946,.F.);
#2563=ORIENTED_EDGE('',*,*,#5962,.F.);
#2564=ORIENTED_EDGE('',*,*,#5963,.T.);
#2565=ORIENTED_EDGE('',*,*,#5964,.F.);
#2566=ORIENTED_EDGE('',*,*,#5947,.F.);
#2567=ORIENTED_EDGE('',*,*,#5965,.F.);
#2568=ORIENTED_EDGE('',*,*,#5966,.T.);
#2569=ORIENTED_EDGE('',*,*,#5967,.F.);
#2570=ORIENTED_EDGE('',*,*,#5949,.F.);
#2571=ORIENTED_EDGE('',*,*,#5968,.F.);
#2572=ORIENTED_EDGE('',*,*,#5969,.T.);
#2573=ORIENTED_EDGE('',*,*,#5970,.T.);
#2574=ORIENTED_EDGE('',*,*,#5954,.F.);
#2575=ORIENTED_EDGE('',*,*,#5951,.F.);
#2576=ORIENTED_EDGE('',*,*,#5971,.T.);
#2577=ORIENTED_EDGE('',*,*,#5972,.T.);
#2578=ORIENTED_EDGE('',*,*,#5957,.F.);
#2579=ORIENTED_EDGE('',*,*,#5973,.T.);
#2580=ORIENTED_EDGE('',*,*,#5974,.T.);
#2581=ORIENTED_EDGE('',*,*,#5975,.T.);
#2582=ORIENTED_EDGE('',*,*,#5960,.F.);
#2583=ORIENTED_EDGE('',*,*,#5976,.T.);
#2584=ORIENTED_EDGE('',*,*,#5977,.T.);
#2585=ORIENTED_EDGE('',*,*,#5978,.T.);
#2586=ORIENTED_EDGE('',*,*,#5966,.F.);
#2587=ORIENTED_EDGE('',*,*,#5963,.F.);
#2588=ORIENTED_EDGE('',*,*,#5979,.T.);
#2589=ORIENTED_EDGE('',*,*,#5980,.F.);
#2590=ORIENTED_EDGE('',*,*,#5970,.F.);
#2591=ORIENTED_EDGE('',*,*,#5981,.F.);
#2592=ORIENTED_EDGE('',*,*,#5982,.T.);
#2593=ORIENTED_EDGE('',*,*,#5983,.F.);
#2594=ORIENTED_EDGE('',*,*,#5973,.F.);
#2595=ORIENTED_EDGE('',*,*,#5984,.F.);
#2596=ORIENTED_EDGE('',*,*,#5985,.T.);
#2597=ORIENTED_EDGE('',*,*,#5986,.F.);
#2598=ORIENTED_EDGE('',*,*,#5971,.F.);
#2599=ORIENTED_EDGE('',*,*,#5987,.F.);
#2600=ORIENTED_EDGE('',*,*,#5988,.T.);
#2601=ORIENTED_EDGE('',*,*,#5989,.F.);
#2602=ORIENTED_EDGE('',*,*,#5974,.F.);
#2603=ORIENTED_EDGE('',*,*,#5990,.F.);
#2604=ORIENTED_EDGE('',*,*,#5991,.T.);
#2605=ORIENTED_EDGE('',*,*,#5992,.F.);
#2606=ORIENTED_EDGE('',*,*,#5975,.F.);
#2607=ORIENTED_EDGE('',*,*,#5993,.F.);
#2608=ORIENTED_EDGE('',*,*,#5994,.T.);
#2609=ORIENTED_EDGE('',*,*,#5995,.F.);
#2610=ORIENTED_EDGE('',*,*,#5977,.F.);
#2611=ORIENTED_EDGE('',*,*,#5996,.F.);
#2612=ORIENTED_EDGE('',*,*,#5997,.T.);
#2613=ORIENTED_EDGE('',*,*,#5998,.T.);
#2614=ORIENTED_EDGE('',*,*,#5982,.F.);
#2615=ORIENTED_EDGE('',*,*,#5979,.F.);
#2616=ORIENTED_EDGE('',*,*,#5985,.F.);
#2617=ORIENTED_EDGE('',*,*,#5999,.T.);
#2618=ORIENTED_EDGE('',*,*,#5988,.F.);
#2619=ORIENTED_EDGE('',*,*,#6000,.T.);
#2620=ORIENTED_EDGE('',*,*,#6001,.T.);
#2621=ORIENTED_EDGE('',*,*,#6002,.T.);
#2622=ORIENTED_EDGE('',*,*,#5994,.F.);
#2623=ORIENTED_EDGE('',*,*,#5991,.F.);
#2624=ORIENTED_EDGE('',*,*,#6003,.T.);
#2625=ORIENTED_EDGE('',*,*,#6004,.F.);
#2626=ORIENTED_EDGE('',*,*,#5998,.F.);
#2627=ORIENTED_EDGE('',*,*,#6005,.F.);
#2628=ORIENTED_EDGE('',*,*,#6006,.T.);
#2629=ORIENTED_EDGE('',*,*,#6007,.F.);
#2630=ORIENTED_EDGE('',*,*,#5999,.F.);
#2631=ORIENTED_EDGE('',*,*,#6008,.F.);
#2632=ORIENTED_EDGE('',*,*,#6009,.T.);
#2633=ORIENTED_EDGE('',*,*,#6010,.F.);
#2634=ORIENTED_EDGE('',*,*,#6001,.F.);
#2635=ORIENTED_EDGE('',*,*,#6011,.F.);
#2636=ORIENTED_EDGE('',*,*,#6003,.F.);
#2637=ORIENTED_EDGE('',*,*,#6012,.T.);
#2638=ORIENTED_EDGE('',*,*,#6009,.F.);
#2639=ORIENTED_EDGE('',*,*,#6006,.F.);
#2640=ORIENTED_EDGE('',*,*,#6013,.T.);
#2641=ORIENTED_EDGE('',*,*,#6014,.F.);
#2642=ORIENTED_EDGE('',*,*,#6015,.T.);
#2643=ORIENTED_EDGE('',*,*,#6016,.F.);
#2644=ORIENTED_EDGE('',*,*,#6017,.T.);
#2645=ORIENTED_EDGE('',*,*,#6018,.F.);
#2646=ORIENTED_EDGE('',*,*,#6019,.T.);
#2647=ORIENTED_EDGE('',*,*,#6020,.T.);
#2648=ORIENTED_EDGE('',*,*,#6021,.T.);
#2649=ORIENTED_EDGE('',*,*,#6022,.T.);
#2650=ORIENTED_EDGE('',*,*,#6023,.T.);
#2651=ORIENTED_EDGE('',*,*,#6024,.T.);
#2652=ORIENTED_EDGE('',*,*,#6025,.F.);
#2653=ORIENTED_EDGE('',*,*,#6026,.T.);
#2654=ORIENTED_EDGE('',*,*,#6027,.T.);
#2655=ORIENTED_EDGE('',*,*,#6028,.T.);
#2656=ORIENTED_EDGE('',*,*,#6029,.F.);
#2657=ORIENTED_EDGE('',*,*,#6030,.F.);
#2658=ORIENTED_EDGE('',*,*,#6031,.F.);
#2659=ORIENTED_EDGE('',*,*,#6032,.F.);
#2660=ORIENTED_EDGE('',*,*,#6033,.T.);
#2661=ORIENTED_EDGE('',*,*,#6025,.T.);
#2662=ORIENTED_EDGE('',*,*,#6034,.T.);
#2663=ORIENTED_EDGE('',*,*,#6027,.F.);
#2664=ORIENTED_EDGE('',*,*,#6034,.F.);
#2665=ORIENTED_EDGE('',*,*,#6024,.F.);
#2666=ORIENTED_EDGE('',*,*,#6035,.F.);
#2667=ORIENTED_EDGE('',*,*,#6028,.F.);
#2668=ORIENTED_EDGE('',*,*,#6033,.F.);
#2669=ORIENTED_EDGE('',*,*,#6026,.F.);
#2670=ORIENTED_EDGE('',*,*,#6036,.F.);
#2671=ORIENTED_EDGE('',*,*,#6019,.F.);
#2672=ORIENTED_EDGE('',*,*,#6037,.T.);
#2673=ORIENTED_EDGE('',*,*,#6038,.T.);
#2674=ORIENTED_EDGE('',*,*,#6039,.F.);
#2675=ORIENTED_EDGE('',*,*,#6040,.F.);
#2676=ORIENTED_EDGE('',*,*,#6041,.F.);
#2677=ORIENTED_EDGE('',*,*,#5883,.F.);
#2678=ORIENTED_EDGE('',*,*,#5899,.T.);
#2679=ORIENTED_EDGE('',*,*,#5916,.F.);
#2680=ORIENTED_EDGE('',*,*,#5930,.T.);
#2681=ORIENTED_EDGE('',*,*,#5944,.F.);
#2682=ORIENTED_EDGE('',*,*,#5958,.T.);
#2683=ORIENTED_EDGE('',*,*,#5972,.F.);
#2684=ORIENTED_EDGE('',*,*,#5986,.T.);
#2685=ORIENTED_EDGE('',*,*,#6000,.F.);
#2686=ORIENTED_EDGE('',*,*,#5990,.T.);
#2687=ORIENTED_EDGE('',*,*,#5976,.F.);
#2688=ORIENTED_EDGE('',*,*,#5962,.T.);
#2689=ORIENTED_EDGE('',*,*,#5948,.F.);
#2690=ORIENTED_EDGE('',*,*,#5934,.T.);
#2691=ORIENTED_EDGE('',*,*,#5920,.F.);
#2692=ORIENTED_EDGE('',*,*,#5903,.T.);
#2693=ORIENTED_EDGE('',*,*,#5888,.F.);
#2694=ORIENTED_EDGE('',*,*,#5875,.T.);
#2695=ORIENTED_EDGE('',*,*,#5869,.F.);
#2696=ORIENTED_EDGE('',*,*,#5863,.T.);
#2697=ORIENTED_EDGE('',*,*,#5858,.T.);
#2698=ORIENTED_EDGE('',*,*,#5865,.F.);
#2699=ORIENTED_EDGE('',*,*,#6042,.T.);
#2700=ORIENTED_EDGE('',*,*,#6043,.T.);
#2701=ORIENTED_EDGE('',*,*,#5931,.T.);
#2702=ORIENTED_EDGE('',*,*,#5927,.T.);
#2703=ORIENTED_EDGE('',*,*,#5952,.T.);
#2704=ORIENTED_EDGE('',*,*,#5956,.T.);
#2705=ORIENTED_EDGE('',*,*,#5900,.T.);
#2706=ORIENTED_EDGE('',*,*,#5896,.T.);
#2707=ORIENTED_EDGE('',*,*,#5924,.T.);
#2708=ORIENTED_EDGE('',*,*,#5928,.T.);
#2709=ORIENTED_EDGE('',*,*,#5897,.T.);
#2710=ORIENTED_EDGE('',*,*,#6044,.T.);
#2711=ORIENTED_EDGE('',*,*,#5871,.T.);
#2712=ORIENTED_EDGE('',*,*,#6045,.T.);
#2713=ORIENTED_EDGE('',*,*,#5872,.T.);
#2714=ORIENTED_EDGE('',*,*,#5860,.T.);
#2715=ORIENTED_EDGE('',*,*,#6046,.T.);
#2716=ORIENTED_EDGE('',*,*,#5894,.T.);
#2717=ORIENTED_EDGE('',*,*,#6046,.F.);
#2718=ORIENTED_EDGE('',*,*,#5862,.T.);
#2719=ORIENTED_EDGE('',*,*,#5877,.T.);
#2720=ORIENTED_EDGE('',*,*,#5911,.T.);
#2721=ORIENTED_EDGE('',*,*,#5874,.T.);
#2722=ORIENTED_EDGE('',*,*,#5905,.T.);
#2723=ORIENTED_EDGE('',*,*,#5909,.T.);
#2724=ORIENTED_EDGE('',*,*,#5878,.T.);
#2725=ORIENTED_EDGE('',*,*,#5933,.T.);
#2726=ORIENTED_EDGE('',*,*,#5964,.T.);
#2727=ORIENTED_EDGE('',*,*,#5968,.T.);
#2728=ORIENTED_EDGE('',*,*,#5937,.T.);
#2729=ORIENTED_EDGE('',*,*,#5961,.T.);
#2730=ORIENTED_EDGE('',*,*,#5992,.T.);
#2731=ORIENTED_EDGE('',*,*,#5996,.T.);
#2732=ORIENTED_EDGE('',*,*,#5965,.T.);
#2733=ORIENTED_EDGE('',*,*,#5989,.T.);
#2734=ORIENTED_EDGE('',*,*,#6007,.T.);
#2735=ORIENTED_EDGE('',*,*,#6011,.T.);
#2736=ORIENTED_EDGE('',*,*,#5993,.T.);
#2737=ORIENTED_EDGE('',*,*,#5987,.T.);
#2738=ORIENTED_EDGE('',*,*,#5983,.T.);
#2739=ORIENTED_EDGE('',*,*,#6004,.T.);
#2740=ORIENTED_EDGE('',*,*,#6008,.T.);
#2741=ORIENTED_EDGE('',*,*,#5959,.T.);
#2742=ORIENTED_EDGE('',*,*,#5955,.T.);
#2743=ORIENTED_EDGE('',*,*,#5980,.T.);
#2744=ORIENTED_EDGE('',*,*,#5984,.T.);
#2745=ORIENTED_EDGE('',*,*,#6002,.F.);
#2746=ORIENTED_EDGE('',*,*,#6010,.T.);
#2747=ORIENTED_EDGE('',*,*,#6012,.F.);
#2748=ORIENTED_EDGE('',*,*,#6005,.T.);
#2749=ORIENTED_EDGE('',*,*,#5997,.F.);
#2750=ORIENTED_EDGE('',*,*,#5981,.T.);
#2751=ORIENTED_EDGE('',*,*,#5969,.F.);
#2752=ORIENTED_EDGE('',*,*,#5953,.T.);
#2753=ORIENTED_EDGE('',*,*,#5941,.F.);
#2754=ORIENTED_EDGE('',*,*,#5925,.T.);
#2755=ORIENTED_EDGE('',*,*,#5912,.F.);
#2756=ORIENTED_EDGE('',*,*,#6047,.T.);
#2757=ORIENTED_EDGE('',*,*,#5879,.F.);
#2758=ORIENTED_EDGE('',*,*,#5893,.T.);
#2759=ORIENTED_EDGE('',*,*,#5910,.T.);
#2760=ORIENTED_EDGE('',*,*,#5889,.F.);
#2761=ORIENTED_EDGE('',*,*,#5908,.T.);
#2762=ORIENTED_EDGE('',*,*,#5922,.F.);
#2763=ORIENTED_EDGE('',*,*,#5939,.T.);
#2764=ORIENTED_EDGE('',*,*,#5950,.F.);
#2765=ORIENTED_EDGE('',*,*,#5967,.T.);
#2766=ORIENTED_EDGE('',*,*,#5978,.F.);
#2767=ORIENTED_EDGE('',*,*,#5995,.T.);
#2768=ORIENTED_EDGE('',*,*,#6048,.T.);
#2769=ORIENTED_EDGE('',*,*,#6049,.T.);
#2770=ORIENTED_EDGE('',*,*,#6050,.T.);
#2771=ORIENTED_EDGE('',*,*,#6051,.T.);
#2772=ORIENTED_EDGE('',*,*,#6023,.F.);
#2773=ORIENTED_EDGE('',*,*,#6022,.F.);
#2774=ORIENTED_EDGE('',*,*,#6021,.F.);
#2775=ORIENTED_EDGE('',*,*,#6020,.F.);
#2776=ORIENTED_EDGE('',*,*,#6036,.T.);
#2777=ORIENTED_EDGE('',*,*,#6051,.F.);
#2778=ORIENTED_EDGE('',*,*,#6032,.T.);
#2779=ORIENTED_EDGE('',*,*,#6031,.T.);
#2780=ORIENTED_EDGE('',*,*,#6030,.T.);
#2781=ORIENTED_EDGE('',*,*,#6029,.T.);
#2782=ORIENTED_EDGE('',*,*,#6035,.T.);
#2783=ORIENTED_EDGE('',*,*,#6037,.F.);
#2784=ORIENTED_EDGE('',*,*,#5902,.T.);
#2785=ORIENTED_EDGE('',*,*,#5936,.T.);
#2786=ORIENTED_EDGE('',*,*,#5940,.T.);
#2787=ORIENTED_EDGE('',*,*,#5906,.T.);
#2788=ORIENTED_EDGE('',*,*,#6018,.T.);
#2789=ORIENTED_EDGE('',*,*,#6050,.F.);
#2790=ORIENTED_EDGE('',*,*,#6039,.T.);
#2791=ORIENTED_EDGE('',*,*,#6017,.F.);
#2792=ORIENTED_EDGE('',*,*,#6016,.T.);
#2793=ORIENTED_EDGE('',*,*,#6049,.F.);
#2794=ORIENTED_EDGE('',*,*,#6040,.T.);
#2795=ORIENTED_EDGE('',*,*,#6015,.F.);
#2796=ORIENTED_EDGE('',*,*,#6014,.T.);
#2797=ORIENTED_EDGE('',*,*,#6048,.F.);
#2798=ORIENTED_EDGE('',*,*,#6041,.T.);
#2799=ORIENTED_EDGE('',*,*,#6013,.F.);
#2800=ORIENTED_EDGE('',*,*,#6047,.F.);
#2801=ORIENTED_EDGE('',*,*,#5914,.T.);
#2802=ORIENTED_EDGE('',*,*,#6045,.F.);
#2803=ORIENTED_EDGE('',*,*,#5880,.F.);
#2804=ORIENTED_EDGE('',*,*,#6044,.F.);
#2805=ORIENTED_EDGE('',*,*,#5884,.T.);
#2806=ORIENTED_EDGE('',*,*,#6042,.F.);
#2807=ORIENTED_EDGE('',*,*,#5864,.F.);
#2808=ORIENTED_EDGE('',*,*,#6043,.F.);
#2809=ORIENTED_EDGE('',*,*,#6052,.F.);
#2810=ORIENTED_EDGE('',*,*,#6052,.T.);
#2811=ORIENTED_EDGE('',*,*,#6038,.F.);
#2812=ORIENTED_EDGE('',*,*,#6053,.T.);
#2813=ORIENTED_EDGE('',*,*,#6054,.T.);
#2814=ORIENTED_EDGE('',*,*,#6055,.F.);
#2815=ORIENTED_EDGE('',*,*,#6056,.F.);
#2816=ORIENTED_EDGE('',*,*,#6057,.F.);
#2817=ORIENTED_EDGE('',*,*,#6054,.F.);
#2818=ORIENTED_EDGE('',*,*,#6058,.F.);
#2819=ORIENTED_EDGE('',*,*,#6056,.T.);
#2820=ORIENTED_EDGE('',*,*,#6059,.F.);
#2821=ORIENTED_EDGE('',*,*,#6060,.F.);
#2822=ORIENTED_EDGE('',*,*,#6061,.T.);
#2823=ORIENTED_EDGE('',*,*,#6062,.T.);
#2824=ORIENTED_EDGE('',*,*,#6063,.F.);
#2825=ORIENTED_EDGE('',*,*,#6064,.F.);
#2826=ORIENTED_EDGE('',*,*,#6064,.T.);
#2827=ORIENTED_EDGE('',*,*,#6065,.F.);
#2828=ORIENTED_EDGE('',*,*,#6066,.F.);
#2829=ORIENTED_EDGE('',*,*,#6067,.F.);
#2830=ORIENTED_EDGE('',*,*,#6062,.F.);
#2831=ORIENTED_EDGE('',*,*,#6068,.F.);
#2832=ORIENTED_EDGE('',*,*,#6069,.F.);
#2833=ORIENTED_EDGE('',*,*,#6070,.T.);
#2834=ORIENTED_EDGE('',*,*,#6071,.T.);
#2835=ORIENTED_EDGE('',*,*,#6072,.F.);
#2836=ORIENTED_EDGE('',*,*,#6073,.T.);
#2837=ORIENTED_EDGE('',*,*,#6074,.T.);
#2838=ORIENTED_EDGE('',*,*,#6075,.F.);
#2839=ORIENTED_EDGE('',*,*,#6076,.F.);
#2840=ORIENTED_EDGE('',*,*,#6063,.T.);
#2841=ORIENTED_EDGE('',*,*,#6075,.T.);
#2842=ORIENTED_EDGE('',*,*,#6055,.T.);
#2843=ORIENTED_EDGE('',*,*,#6072,.T.);
#2844=ORIENTED_EDGE('',*,*,#6077,.T.);
#2845=ORIENTED_EDGE('',*,*,#6078,.F.);
#2846=ORIENTED_EDGE('',*,*,#6079,.F.);
#2847=ORIENTED_EDGE('',*,*,#6080,.F.);
#2848=ORIENTED_EDGE('',*,*,#6065,.T.);
#2849=ORIENTED_EDGE('',*,*,#6071,.F.);
#2850=ORIENTED_EDGE('',*,*,#6076,.T.);
#2851=ORIENTED_EDGE('',*,*,#6067,.T.);
#2852=ORIENTED_EDGE('',*,*,#6081,.F.);
#2853=ORIENTED_EDGE('',*,*,#6069,.T.);
#2854=ORIENTED_EDGE('',*,*,#6057,.T.);
#2855=ORIENTED_EDGE('',*,*,#6082,.F.);
#2856=ORIENTED_EDGE('',*,*,#6083,.F.);
#2857=ORIENTED_EDGE('',*,*,#6059,.T.);
#2858=ORIENTED_EDGE('',*,*,#6074,.F.);
#2859=ORIENTED_EDGE('',*,*,#6070,.F.);
#2860=ORIENTED_EDGE('',*,*,#6082,.T.);
#2861=ORIENTED_EDGE('',*,*,#6058,.T.);
#2862=ORIENTED_EDGE('',*,*,#6053,.F.);
#2863=ORIENTED_EDGE('',*,*,#6060,.T.);
#2864=ORIENTED_EDGE('',*,*,#6083,.T.);
#2865=ORIENTED_EDGE('',*,*,#6073,.F.);
#2866=ORIENTED_EDGE('',*,*,#6081,.T.);
#2867=ORIENTED_EDGE('',*,*,#6068,.T.);
#2868=ORIENTED_EDGE('',*,*,#6061,.F.);
#2869=ORIENTED_EDGE('',*,*,#6066,.T.);
#2870=ORIENTED_EDGE('',*,*,#6080,.T.);
#2871=ORIENTED_EDGE('',*,*,#6084,.T.);
#2872=ORIENTED_EDGE('',*,*,#6077,.F.);
#2873=ORIENTED_EDGE('',*,*,#6079,.T.);
#2874=ORIENTED_EDGE('',*,*,#6078,.T.);
#2875=ORIENTED_EDGE('',*,*,#6084,.F.);
#2876=ORIENTED_EDGE('',*,*,#6085,.F.);
#2877=ORIENTED_EDGE('',*,*,#6086,.T.);
#2878=ORIENTED_EDGE('',*,*,#6087,.T.);
#2879=ORIENTED_EDGE('',*,*,#6088,.F.);
#2880=ORIENTED_EDGE('',*,*,#6085,.T.);
#2881=ORIENTED_EDGE('',*,*,#6087,.F.);
#2882=ORIENTED_EDGE('',*,*,#6086,.F.);
#2883=ORIENTED_EDGE('',*,*,#6089,.F.);
#2884=ORIENTED_EDGE('',*,*,#6089,.T.);
#2885=ORIENTED_EDGE('',*,*,#6090,.T.);
#2886=ORIENTED_EDGE('',*,*,#6088,.T.);
#2887=ORIENTED_EDGE('',*,*,#6090,.F.);
#2888=ORIENTED_EDGE('',*,*,#6091,.F.);
#2889=ORIENTED_EDGE('',*,*,#6092,.T.);
#2890=ORIENTED_EDGE('',*,*,#6093,.F.);
#2891=ORIENTED_EDGE('',*,*,#6094,.T.);
#2892=ORIENTED_EDGE('',*,*,#6095,.F.);
#2893=ORIENTED_EDGE('',*,*,#6096,.T.);
#2894=ORIENTED_EDGE('',*,*,#6097,.F.);
#2895=ORIENTED_EDGE('',*,*,#6098,.T.);
#2896=ORIENTED_EDGE('',*,*,#6099,.F.);
#2897=ORIENTED_EDGE('',*,*,#6100,.T.);
#2898=ORIENTED_EDGE('',*,*,#6101,.T.);
#2899=ORIENTED_EDGE('',*,*,#6100,.F.);
#2900=ORIENTED_EDGE('',*,*,#6101,.F.);
#2901=ORIENTED_EDGE('',*,*,#6097,.T.);
#2902=ORIENTED_EDGE('',*,*,#6095,.T.);
#2903=ORIENTED_EDGE('',*,*,#6098,.F.);
#2904=ORIENTED_EDGE('',*,*,#6096,.F.);
#2905=ORIENTED_EDGE('',*,*,#6093,.T.);
#2906=ORIENTED_EDGE('',*,*,#6091,.T.);
#2907=ORIENTED_EDGE('',*,*,#6094,.F.);
#2908=ORIENTED_EDGE('',*,*,#6099,.T.);
#2909=ORIENTED_EDGE('',*,*,#6092,.F.);
#2910=ORIENTED_EDGE('',*,*,#6102,.T.);
#2911=ORIENTED_EDGE('',*,*,#6103,.T.);
#2912=ORIENTED_EDGE('',*,*,#6104,.T.);
#2913=ORIENTED_EDGE('',*,*,#6105,.F.);
#2914=ORIENTED_EDGE('',*,*,#6106,.F.);
#2915=ORIENTED_EDGE('',*,*,#6107,.F.);
#2916=ORIENTED_EDGE('',*,*,#6108,.F.);
#2917=ORIENTED_EDGE('',*,*,#6109,.F.);
#2918=ORIENTED_EDGE('',*,*,#6110,.T.);
#2919=ORIENTED_EDGE('',*,*,#6111,.T.);
#2920=ORIENTED_EDGE('',*,*,#6112,.T.);
#2921=ORIENTED_EDGE('',*,*,#6103,.F.);
#2922=ORIENTED_EDGE('',*,*,#6113,.T.);
#2923=ORIENTED_EDGE('',*,*,#6114,.T.);
#2924=ORIENTED_EDGE('',*,*,#6115,.T.);
#2925=ORIENTED_EDGE('',*,*,#6110,.F.);
#2926=ORIENTED_EDGE('',*,*,#6116,.T.);
#2927=ORIENTED_EDGE('',*,*,#6117,.T.);
#2928=ORIENTED_EDGE('',*,*,#6118,.T.);
#2929=ORIENTED_EDGE('',*,*,#6114,.F.);
#2930=ORIENTED_EDGE('',*,*,#6119,.T.);
#2931=ORIENTED_EDGE('',*,*,#6120,.F.);
#2932=ORIENTED_EDGE('',*,*,#6121,.F.);
#2933=ORIENTED_EDGE('',*,*,#6122,.F.);
#2934=ORIENTED_EDGE('',*,*,#6119,.F.);
#2935=ORIENTED_EDGE('',*,*,#6116,.F.);
#2936=ORIENTED_EDGE('',*,*,#6113,.F.);
#2937=ORIENTED_EDGE('',*,*,#6102,.F.);
#2938=ORIENTED_EDGE('',*,*,#6123,.F.);
#2939=ORIENTED_EDGE('',*,*,#6124,.T.);
#2940=ORIENTED_EDGE('',*,*,#6125,.T.);
#2941=ORIENTED_EDGE('',*,*,#6126,.F.);
#2942=ORIENTED_EDGE('',*,*,#6127,.T.);
#2943=ORIENTED_EDGE('',*,*,#6128,.T.);
#2944=ORIENTED_EDGE('',*,*,#6129,.T.);
#2945=ORIENTED_EDGE('',*,*,#6117,.F.);
#2946=ORIENTED_EDGE('',*,*,#6122,.T.);
#2947=ORIENTED_EDGE('',*,*,#6130,.T.);
#2948=ORIENTED_EDGE('',*,*,#6131,.T.);
#2949=ORIENTED_EDGE('',*,*,#6128,.F.);
#2950=ORIENTED_EDGE('',*,*,#6121,.T.);
#2951=ORIENTED_EDGE('',*,*,#6126,.T.);
#2952=ORIENTED_EDGE('',*,*,#6132,.T.);
#2953=ORIENTED_EDGE('',*,*,#6130,.F.);
#2954=ORIENTED_EDGE('',*,*,#6120,.T.);
#2955=ORIENTED_EDGE('',*,*,#6133,.T.);
#2956=ORIENTED_EDGE('',*,*,#6134,.T.);
#2957=ORIENTED_EDGE('',*,*,#6135,.T.);
#2958=ORIENTED_EDGE('',*,*,#6136,.T.);
#2959=ORIENTED_EDGE('',*,*,#6112,.F.);
#2960=ORIENTED_EDGE('',*,*,#6137,.T.);
#2961=ORIENTED_EDGE('',*,*,#6124,.F.);
#2962=ORIENTED_EDGE('',*,*,#6138,.F.);
#2963=ORIENTED_EDGE('',*,*,#6104,.F.);
#2964=ORIENTED_EDGE('',*,*,#6139,.F.);
#2965=ORIENTED_EDGE('',*,*,#6140,.T.);
#2966=ORIENTED_EDGE('',*,*,#6141,.F.);
#2967=ORIENTED_EDGE('',*,*,#6142,.F.);
#2968=ORIENTED_EDGE('',*,*,#6143,.F.);
#2969=ORIENTED_EDGE('',*,*,#6144,.F.);
#2970=ORIENTED_EDGE('',*,*,#6145,.T.);
#2971=ORIENTED_EDGE('',*,*,#6146,.T.);
#2972=ORIENTED_EDGE('',*,*,#6143,.T.);
#2973=ORIENTED_EDGE('',*,*,#6147,.F.);
#2974=ORIENTED_EDGE('',*,*,#6148,.T.);
#2975=ORIENTED_EDGE('',*,*,#6144,.T.);
#2976=ORIENTED_EDGE('',*,*,#6142,.T.);
#2977=ORIENTED_EDGE('',*,*,#6141,.T.);
#2978=ORIENTED_EDGE('',*,*,#6149,.T.);
#2979=ORIENTED_EDGE('',*,*,#6147,.T.);
#2980=ORIENTED_EDGE('',*,*,#6146,.F.);
#2981=ORIENTED_EDGE('',*,*,#6150,.T.);
#2982=ORIENTED_EDGE('',*,*,#6139,.T.);
#2983=ORIENTED_EDGE('',*,*,#6151,.F.);
#2984=ORIENTED_EDGE('',*,*,#6152,.F.);
#2985=ORIENTED_EDGE('',*,*,#6153,.T.);
#2986=ORIENTED_EDGE('',*,*,#6148,.F.);
#2987=ORIENTED_EDGE('',*,*,#6149,.F.);
#2988=ORIENTED_EDGE('',*,*,#6140,.F.);
#2989=ORIENTED_EDGE('',*,*,#6150,.F.);
#2990=ORIENTED_EDGE('',*,*,#6145,.F.);
#2991=ORIENTED_EDGE('',*,*,#6154,.T.);
#2992=ORIENTED_EDGE('',*,*,#6127,.F.);
#2993=ORIENTED_EDGE('',*,*,#6155,.F.);
#2994=ORIENTED_EDGE('',*,*,#6156,.T.);
#2995=ORIENTED_EDGE('',*,*,#6157,.T.);
#2996=ORIENTED_EDGE('',*,*,#6158,.F.);
#2997=ORIENTED_EDGE('',*,*,#6131,.F.);
#2998=ORIENTED_EDGE('',*,*,#6132,.F.);
#2999=ORIENTED_EDGE('',*,*,#6125,.F.);
#3000=ORIENTED_EDGE('',*,*,#6137,.F.);
#3001=ORIENTED_EDGE('',*,*,#6111,.F.);
#3002=ORIENTED_EDGE('',*,*,#6115,.F.);
#3003=ORIENTED_EDGE('',*,*,#6118,.F.);
#3004=ORIENTED_EDGE('',*,*,#6129,.F.);
#3005=ORIENTED_EDGE('',*,*,#6157,.F.);
#3006=ORIENTED_EDGE('',*,*,#6155,.T.);
#3007=ORIENTED_EDGE('',*,*,#6156,.F.);
#3008=ORIENTED_EDGE('',*,*,#6158,.T.);
#3009=ORIENTED_EDGE('',*,*,#6106,.T.);
#3010=ORIENTED_EDGE('',*,*,#6105,.T.);
#3011=ORIENTED_EDGE('',*,*,#6138,.T.);
#3012=ORIENTED_EDGE('',*,*,#6154,.F.);
#3013=ORIENTED_EDGE('',*,*,#6136,.F.);
#3014=ORIENTED_EDGE('',*,*,#6135,.F.);
#3015=ORIENTED_EDGE('',*,*,#6134,.F.);
#3016=ORIENTED_EDGE('',*,*,#6133,.F.);
#3017=ORIENTED_EDGE('',*,*,#6123,.T.);
#3018=ORIENTED_EDGE('',*,*,#6151,.T.);
#3019=ORIENTED_EDGE('',*,*,#6109,.T.);
#3020=ORIENTED_EDGE('',*,*,#6108,.T.);
#3021=ORIENTED_EDGE('',*,*,#6107,.T.);
#3022=ORIENTED_EDGE('',*,*,#6152,.T.);
#3023=ORIENTED_EDGE('',*,*,#6153,.F.);
#3024=ORIENTED_EDGE('',*,*,#6159,.F.);
#3025=ORIENTED_EDGE('',*,*,#6160,.T.);
#3026=ORIENTED_EDGE('',*,*,#6161,.F.);
#3027=ORIENTED_EDGE('',*,*,#6162,.T.);
#3028=ORIENTED_EDGE('',*,*,#6163,.T.);
#3029=ORIENTED_EDGE('',*,*,#6164,.T.);
#3030=ORIENTED_EDGE('',*,*,#6165,.T.);
#3031=ORIENTED_EDGE('',*,*,#6166,.T.);
#3032=ORIENTED_EDGE('',*,*,#6167,.T.);
#3033=ORIENTED_EDGE('',*,*,#6168,.T.);
#3034=ORIENTED_EDGE('',*,*,#6162,.F.);
#3035=ORIENTED_EDGE('',*,*,#6169,.T.);
#3036=ORIENTED_EDGE('',*,*,#6170,.F.);
#3037=ORIENTED_EDGE('',*,*,#6161,.T.);
#3038=ORIENTED_EDGE('',*,*,#6171,.F.);
#3039=ORIENTED_EDGE('',*,*,#6170,.T.);
#3040=ORIENTED_EDGE('',*,*,#6171,.T.);
#3041=ORIENTED_EDGE('',*,*,#6172,.F.);
#3042=ORIENTED_EDGE('',*,*,#6172,.T.);
#3043=ORIENTED_EDGE('',*,*,#6173,.F.);
#3044=ORIENTED_EDGE('',*,*,#6160,.F.);
#3045=ORIENTED_EDGE('',*,*,#6173,.T.);
#3046=ORIENTED_EDGE('',*,*,#6159,.T.);
#3047=ORIENTED_EDGE('',*,*,#6174,.T.);
#3048=ORIENTED_EDGE('',*,*,#6175,.T.);
#3049=ORIENTED_EDGE('',*,*,#6176,.T.);
#3050=ORIENTED_EDGE('',*,*,#6177,.F.);
#3051=ORIENTED_EDGE('',*,*,#6178,.T.);
#3052=ORIENTED_EDGE('',*,*,#6177,.T.);
#3053=ORIENTED_EDGE('',*,*,#6179,.F.);
#3054=ORIENTED_EDGE('',*,*,#6179,.T.);
#3055=ORIENTED_EDGE('',*,*,#6180,.T.);
#3056=ORIENTED_EDGE('',*,*,#6163,.F.);
#3057=ORIENTED_EDGE('',*,*,#6167,.F.);
#3058=ORIENTED_EDGE('',*,*,#6164,.F.);
#3059=ORIENTED_EDGE('',*,*,#6169,.F.);
#3060=ORIENTED_EDGE('',*,*,#6166,.F.);
#3061=ORIENTED_EDGE('',*,*,#6168,.F.);
#3062=ORIENTED_EDGE('',*,*,#6180,.F.);
#3063=ORIENTED_EDGE('',*,*,#6165,.F.);
#3064=ORIENTED_EDGE('',*,*,#6175,.F.);
#3065=ORIENTED_EDGE('',*,*,#6178,.F.);
#3066=ORIENTED_EDGE('',*,*,#6174,.F.);
#3067=ORIENTED_EDGE('',*,*,#6176,.F.);
#3068=ORIENTED_EDGE('',*,*,#6181,.F.);
#3069=ORIENTED_EDGE('',*,*,#6182,.F.);
#3070=ORIENTED_EDGE('',*,*,#6183,.F.);
#3071=ORIENTED_EDGE('',*,*,#6184,.F.);
#3072=ORIENTED_EDGE('',*,*,#6185,.F.);
#3073=ORIENTED_EDGE('',*,*,#6186,.F.);
#3074=ORIENTED_EDGE('',*,*,#6187,.F.);
#3075=ORIENTED_EDGE('',*,*,#6188,.F.);
#3076=ORIENTED_EDGE('',*,*,#6189,.F.);
#3077=ORIENTED_EDGE('',*,*,#6190,.F.);
#3078=ORIENTED_EDGE('',*,*,#6191,.F.);
#3079=ORIENTED_EDGE('',*,*,#6192,.T.);
#3080=ORIENTED_EDGE('',*,*,#6193,.F.);
#3081=ORIENTED_EDGE('',*,*,#6194,.F.);
#3082=ORIENTED_EDGE('',*,*,#6195,.T.);
#3083=ORIENTED_EDGE('',*,*,#6196,.T.);
#3084=ORIENTED_EDGE('',*,*,#6197,.T.);
#3085=ORIENTED_EDGE('',*,*,#6198,.T.);
#3086=ORIENTED_EDGE('',*,*,#6199,.T.);
#3087=ORIENTED_EDGE('',*,*,#6200,.T.);
#3088=ORIENTED_EDGE('',*,*,#6201,.T.);
#3089=ORIENTED_EDGE('',*,*,#6202,.T.);
#3090=ORIENTED_EDGE('',*,*,#6203,.F.);
#3091=ORIENTED_EDGE('',*,*,#6204,.F.);
#3092=ORIENTED_EDGE('',*,*,#6205,.F.);
#3093=ORIENTED_EDGE('',*,*,#6204,.T.);
#3094=ORIENTED_EDGE('',*,*,#6206,.F.);
#3095=ORIENTED_EDGE('',*,*,#6192,.F.);
#3096=ORIENTED_EDGE('',*,*,#6207,.F.);
#3097=ORIENTED_EDGE('',*,*,#6193,.T.);
#3098=ORIENTED_EDGE('',*,*,#6206,.T.);
#3099=ORIENTED_EDGE('',*,*,#6203,.T.);
#3100=ORIENTED_EDGE('',*,*,#6208,.T.);
#3101=ORIENTED_EDGE('',*,*,#6205,.T.);
#3102=ORIENTED_EDGE('',*,*,#6191,.T.);
#3103=ORIENTED_EDGE('',*,*,#6209,.T.);
#3104=ORIENTED_EDGE('',*,*,#6194,.T.);
#3105=ORIENTED_EDGE('',*,*,#6210,.T.);
#3106=ORIENTED_EDGE('',*,*,#6211,.T.);
#3107=ORIENTED_EDGE('',*,*,#6212,.F.);
#3108=ORIENTED_EDGE('',*,*,#6213,.F.);
#3109=ORIENTED_EDGE('',*,*,#6214,.F.);
#3110=ORIENTED_EDGE('',*,*,#6215,.F.);
#3111=ORIENTED_EDGE('',*,*,#6216,.F.);
#3112=ORIENTED_EDGE('',*,*,#6217,.F.);
#3113=ORIENTED_EDGE('',*,*,#6218,.F.);
#3114=ORIENTED_EDGE('',*,*,#6219,.F.);
#3115=ORIENTED_EDGE('',*,*,#6220,.F.);
#3116=ORIENTED_EDGE('',*,*,#6221,.F.);
#3117=ORIENTED_EDGE('',*,*,#6222,.F.);
#3118=ORIENTED_EDGE('',*,*,#6223,.F.);
#3119=ORIENTED_EDGE('',*,*,#6224,.F.);
#3120=ORIENTED_EDGE('',*,*,#6225,.F.);
#3121=ORIENTED_EDGE('',*,*,#6226,.F.);
#3122=ORIENTED_EDGE('',*,*,#6227,.F.);
#3123=ORIENTED_EDGE('',*,*,#6228,.F.);
#3124=ORIENTED_EDGE('',*,*,#6229,.F.);
#3125=ORIENTED_EDGE('',*,*,#6230,.F.);
#3126=ORIENTED_EDGE('',*,*,#6231,.F.);
#3127=ORIENTED_EDGE('',*,*,#6232,.F.);
#3128=ORIENTED_EDGE('',*,*,#6233,.F.);
#3129=ORIENTED_EDGE('',*,*,#6234,.F.);
#3130=ORIENTED_EDGE('',*,*,#6235,.F.);
#3131=ORIENTED_EDGE('',*,*,#6236,.F.);
#3132=ORIENTED_EDGE('',*,*,#6237,.F.);
#3133=ORIENTED_EDGE('',*,*,#6238,.F.);
#3134=ORIENTED_EDGE('',*,*,#6239,.F.);
#3135=ORIENTED_EDGE('',*,*,#6240,.F.);
#3136=ORIENTED_EDGE('',*,*,#6241,.F.);
#3137=ORIENTED_EDGE('',*,*,#6242,.F.);
#3138=ORIENTED_EDGE('',*,*,#6243,.F.);
#3139=ORIENTED_EDGE('',*,*,#6244,.F.);
#3140=ORIENTED_EDGE('',*,*,#6245,.F.);
#3141=ORIENTED_EDGE('',*,*,#6246,.F.);
#3142=ORIENTED_EDGE('',*,*,#6247,.F.);
#3143=ORIENTED_EDGE('',*,*,#6248,.F.);
#3144=ORIENTED_EDGE('',*,*,#6249,.F.);
#3145=ORIENTED_EDGE('',*,*,#6250,.F.);
#3146=ORIENTED_EDGE('',*,*,#6251,.F.);
#3147=ORIENTED_EDGE('',*,*,#6252,.F.);
#3148=ORIENTED_EDGE('',*,*,#6253,.F.);
#3149=ORIENTED_EDGE('',*,*,#6254,.F.);
#3150=ORIENTED_EDGE('',*,*,#6255,.F.);
#3151=ORIENTED_EDGE('',*,*,#6256,.F.);
#3152=ORIENTED_EDGE('',*,*,#6257,.F.);
#3153=ORIENTED_EDGE('',*,*,#6258,.F.);
#3154=ORIENTED_EDGE('',*,*,#6259,.F.);
#3155=ORIENTED_EDGE('',*,*,#6260,.F.);
#3156=ORIENTED_EDGE('',*,*,#6261,.F.);
#3157=ORIENTED_EDGE('',*,*,#6262,.F.);
#3158=ORIENTED_EDGE('',*,*,#6263,.F.);
#3159=ORIENTED_EDGE('',*,*,#6264,.F.);
#3160=ORIENTED_EDGE('',*,*,#6265,.F.);
#3161=ORIENTED_EDGE('',*,*,#6266,.F.);
#3162=ORIENTED_EDGE('',*,*,#6267,.F.);
#3163=ORIENTED_EDGE('',*,*,#6268,.F.);
#3164=ORIENTED_EDGE('',*,*,#6269,.F.);
#3165=ORIENTED_EDGE('',*,*,#6270,.F.);
#3166=ORIENTED_EDGE('',*,*,#6271,.F.);
#3167=ORIENTED_EDGE('',*,*,#6272,.F.);
#3168=ORIENTED_EDGE('',*,*,#6273,.F.);
#3169=ORIENTED_EDGE('',*,*,#6274,.F.);
#3170=ORIENTED_EDGE('',*,*,#6275,.F.);
#3171=ORIENTED_EDGE('',*,*,#6276,.F.);
#3172=ORIENTED_EDGE('',*,*,#6277,.F.);
#3173=ORIENTED_EDGE('',*,*,#6278,.F.);
#3174=ORIENTED_EDGE('',*,*,#6279,.F.);
#3175=ORIENTED_EDGE('',*,*,#6280,.F.);
#3176=ORIENTED_EDGE('',*,*,#6281,.F.);
#3177=ORIENTED_EDGE('',*,*,#6282,.F.);
#3178=ORIENTED_EDGE('',*,*,#6283,.F.);
#3179=ORIENTED_EDGE('',*,*,#6284,.F.);
#3180=ORIENTED_EDGE('',*,*,#6285,.F.);
#3181=ORIENTED_EDGE('',*,*,#6286,.F.);
#3182=ORIENTED_EDGE('',*,*,#6287,.F.);
#3183=ORIENTED_EDGE('',*,*,#6288,.F.);
#3184=ORIENTED_EDGE('',*,*,#6289,.F.);
#3185=ORIENTED_EDGE('',*,*,#6290,.F.);
#3186=ORIENTED_EDGE('',*,*,#6291,.F.);
#3187=ORIENTED_EDGE('',*,*,#6292,.F.);
#3188=ORIENTED_EDGE('',*,*,#6293,.F.);
#3189=ORIENTED_EDGE('',*,*,#6294,.F.);
#3190=ORIENTED_EDGE('',*,*,#6295,.F.);
#3191=ORIENTED_EDGE('',*,*,#6296,.F.);
#3192=ORIENTED_EDGE('',*,*,#6297,.F.);
#3193=ORIENTED_EDGE('',*,*,#6298,.F.);
#3194=ORIENTED_EDGE('',*,*,#6299,.F.);
#3195=ORIENTED_EDGE('',*,*,#6300,.F.);
#3196=ORIENTED_EDGE('',*,*,#6301,.F.);
#3197=ORIENTED_EDGE('',*,*,#6302,.F.);
#3198=ORIENTED_EDGE('',*,*,#6303,.F.);
#3199=ORIENTED_EDGE('',*,*,#6304,.F.);
#3200=ORIENTED_EDGE('',*,*,#6305,.F.);
#3201=ORIENTED_EDGE('',*,*,#6306,.F.);
#3202=ORIENTED_EDGE('',*,*,#6307,.F.);
#3203=ORIENTED_EDGE('',*,*,#6308,.F.);
#3204=ORIENTED_EDGE('',*,*,#6309,.F.);
#3205=ORIENTED_EDGE('',*,*,#6310,.F.);
#3206=ORIENTED_EDGE('',*,*,#6311,.F.);
#3207=ORIENTED_EDGE('',*,*,#6312,.F.);
#3208=ORIENTED_EDGE('',*,*,#6313,.F.);
#3209=ORIENTED_EDGE('',*,*,#6314,.F.);
#3210=ORIENTED_EDGE('',*,*,#6315,.F.);
#3211=ORIENTED_EDGE('',*,*,#6316,.F.);
#3212=ORIENTED_EDGE('',*,*,#6317,.F.);
#3213=ORIENTED_EDGE('',*,*,#6318,.F.);
#3214=ORIENTED_EDGE('',*,*,#6319,.F.);
#3215=ORIENTED_EDGE('',*,*,#6320,.F.);
#3216=ORIENTED_EDGE('',*,*,#6321,.F.);
#3217=ORIENTED_EDGE('',*,*,#6322,.F.);
#3218=ORIENTED_EDGE('',*,*,#6323,.F.);
#3219=ORIENTED_EDGE('',*,*,#6324,.F.);
#3220=ORIENTED_EDGE('',*,*,#6325,.F.);
#3221=ORIENTED_EDGE('',*,*,#6326,.F.);
#3222=ORIENTED_EDGE('',*,*,#6327,.F.);
#3223=ORIENTED_EDGE('',*,*,#6328,.F.);
#3224=ORIENTED_EDGE('',*,*,#6329,.F.);
#3225=ORIENTED_EDGE('',*,*,#6330,.F.);
#3226=ORIENTED_EDGE('',*,*,#6331,.F.);
#3227=ORIENTED_EDGE('',*,*,#6332,.F.);
#3228=ORIENTED_EDGE('',*,*,#6333,.F.);
#3229=ORIENTED_EDGE('',*,*,#6334,.F.);
#3230=ORIENTED_EDGE('',*,*,#6335,.F.);
#3231=ORIENTED_EDGE('',*,*,#6336,.F.);
#3232=ORIENTED_EDGE('',*,*,#6337,.F.);
#3233=ORIENTED_EDGE('',*,*,#6338,.F.);
#3234=ORIENTED_EDGE('',*,*,#6339,.F.);
#3235=ORIENTED_EDGE('',*,*,#6340,.F.);
#3236=ORIENTED_EDGE('',*,*,#6341,.F.);
#3237=ORIENTED_EDGE('',*,*,#6342,.F.);
#3238=ORIENTED_EDGE('',*,*,#6343,.F.);
#3239=ORIENTED_EDGE('',*,*,#6344,.F.);
#3240=ORIENTED_EDGE('',*,*,#6345,.F.);
#3241=ORIENTED_EDGE('',*,*,#6346,.F.);
#3242=ORIENTED_EDGE('',*,*,#6347,.F.);
#3243=ORIENTED_EDGE('',*,*,#6348,.F.);
#3244=ORIENTED_EDGE('',*,*,#6349,.F.);
#3245=ORIENTED_EDGE('',*,*,#6350,.F.);
#3246=ORIENTED_EDGE('',*,*,#6351,.F.);
#3247=ORIENTED_EDGE('',*,*,#6352,.F.);
#3248=ORIENTED_EDGE('',*,*,#6353,.F.);
#3249=ORIENTED_EDGE('',*,*,#6354,.F.);
#3250=ORIENTED_EDGE('',*,*,#6355,.F.);
#3251=ORIENTED_EDGE('',*,*,#6356,.T.);
#3252=ORIENTED_EDGE('',*,*,#6357,.T.);
#3253=ORIENTED_EDGE('',*,*,#6358,.T.);
#3254=ORIENTED_EDGE('',*,*,#6359,.T.);
#3255=ORIENTED_EDGE('',*,*,#6360,.T.);
#3256=ORIENTED_EDGE('',*,*,#6361,.T.);
#3257=ORIENTED_EDGE('',*,*,#6362,.T.);
#3258=ORIENTED_EDGE('',*,*,#6363,.T.);
#3259=ORIENTED_EDGE('',*,*,#6364,.T.);
#3260=ORIENTED_EDGE('',*,*,#6365,.T.);
#3261=ORIENTED_EDGE('',*,*,#6366,.T.);
#3262=ORIENTED_EDGE('',*,*,#6367,.T.);
#3263=ORIENTED_EDGE('',*,*,#6368,.T.);
#3264=ORIENTED_EDGE('',*,*,#6369,.T.);
#3265=ORIENTED_EDGE('',*,*,#6370,.T.);
#3266=ORIENTED_EDGE('',*,*,#6371,.T.);
#3267=ORIENTED_EDGE('',*,*,#6372,.T.);
#3268=ORIENTED_EDGE('',*,*,#6373,.T.);
#3269=ORIENTED_EDGE('',*,*,#6374,.T.);
#3270=ORIENTED_EDGE('',*,*,#6375,.T.);
#3271=ORIENTED_EDGE('',*,*,#6376,.T.);
#3272=ORIENTED_EDGE('',*,*,#6377,.T.);
#3273=ORIENTED_EDGE('',*,*,#6378,.T.);
#3274=ORIENTED_EDGE('',*,*,#6379,.T.);
#3275=ORIENTED_EDGE('',*,*,#6380,.T.);
#3276=ORIENTED_EDGE('',*,*,#6381,.T.);
#3277=ORIENTED_EDGE('',*,*,#6382,.T.);
#3278=ORIENTED_EDGE('',*,*,#6383,.T.);
#3279=ORIENTED_EDGE('',*,*,#6384,.T.);
#3280=ORIENTED_EDGE('',*,*,#6385,.T.);
#3281=ORIENTED_EDGE('',*,*,#6386,.T.);
#3282=ORIENTED_EDGE('',*,*,#6387,.T.);
#3283=ORIENTED_EDGE('',*,*,#6388,.T.);
#3284=ORIENTED_EDGE('',*,*,#6389,.T.);
#3285=ORIENTED_EDGE('',*,*,#6390,.T.);
#3286=ORIENTED_EDGE('',*,*,#6391,.T.);
#3287=ORIENTED_EDGE('',*,*,#6392,.T.);
#3288=ORIENTED_EDGE('',*,*,#6393,.T.);
#3289=ORIENTED_EDGE('',*,*,#6394,.T.);
#3290=ORIENTED_EDGE('',*,*,#6395,.T.);
#3291=ORIENTED_EDGE('',*,*,#6396,.T.);
#3292=ORIENTED_EDGE('',*,*,#6397,.T.);
#3293=ORIENTED_EDGE('',*,*,#6398,.T.);
#3294=ORIENTED_EDGE('',*,*,#6399,.T.);
#3295=ORIENTED_EDGE('',*,*,#6400,.T.);
#3296=ORIENTED_EDGE('',*,*,#6401,.T.);
#3297=ORIENTED_EDGE('',*,*,#6402,.T.);
#3298=ORIENTED_EDGE('',*,*,#6403,.T.);
#3299=ORIENTED_EDGE('',*,*,#6404,.T.);
#3300=ORIENTED_EDGE('',*,*,#6405,.T.);
#3301=ORIENTED_EDGE('',*,*,#6406,.T.);
#3302=ORIENTED_EDGE('',*,*,#6407,.T.);
#3303=ORIENTED_EDGE('',*,*,#6408,.T.);
#3304=ORIENTED_EDGE('',*,*,#6409,.T.);
#3305=ORIENTED_EDGE('',*,*,#6410,.T.);
#3306=ORIENTED_EDGE('',*,*,#6411,.T.);
#3307=ORIENTED_EDGE('',*,*,#6412,.T.);
#3308=ORIENTED_EDGE('',*,*,#6413,.T.);
#3309=ORIENTED_EDGE('',*,*,#6414,.T.);
#3310=ORIENTED_EDGE('',*,*,#6415,.T.);
#3311=ORIENTED_EDGE('',*,*,#6416,.T.);
#3312=ORIENTED_EDGE('',*,*,#6417,.T.);
#3313=ORIENTED_EDGE('',*,*,#6418,.T.);
#3314=ORIENTED_EDGE('',*,*,#6419,.T.);
#3315=ORIENTED_EDGE('',*,*,#6420,.T.);
#3316=ORIENTED_EDGE('',*,*,#6421,.T.);
#3317=ORIENTED_EDGE('',*,*,#6422,.T.);
#3318=ORIENTED_EDGE('',*,*,#6423,.T.);
#3319=ORIENTED_EDGE('',*,*,#6424,.T.);
#3320=ORIENTED_EDGE('',*,*,#6425,.T.);
#3321=ORIENTED_EDGE('',*,*,#6426,.T.);
#3322=ORIENTED_EDGE('',*,*,#6427,.T.);
#3323=ORIENTED_EDGE('',*,*,#6428,.T.);
#3324=ORIENTED_EDGE('',*,*,#6429,.T.);
#3325=ORIENTED_EDGE('',*,*,#6430,.T.);
#3326=ORIENTED_EDGE('',*,*,#6431,.T.);
#3327=ORIENTED_EDGE('',*,*,#6432,.T.);
#3328=ORIENTED_EDGE('',*,*,#6433,.T.);
#3329=ORIENTED_EDGE('',*,*,#6434,.T.);
#3330=ORIENTED_EDGE('',*,*,#6435,.T.);
#3331=ORIENTED_EDGE('',*,*,#6436,.T.);
#3332=ORIENTED_EDGE('',*,*,#6437,.T.);
#3333=ORIENTED_EDGE('',*,*,#6438,.T.);
#3334=ORIENTED_EDGE('',*,*,#6439,.T.);
#3335=ORIENTED_EDGE('',*,*,#6440,.T.);
#3336=ORIENTED_EDGE('',*,*,#6441,.T.);
#3337=ORIENTED_EDGE('',*,*,#6442,.T.);
#3338=ORIENTED_EDGE('',*,*,#6443,.T.);
#3339=ORIENTED_EDGE('',*,*,#6444,.T.);
#3340=ORIENTED_EDGE('',*,*,#6445,.T.);
#3341=ORIENTED_EDGE('',*,*,#6446,.T.);
#3342=ORIENTED_EDGE('',*,*,#6447,.T.);
#3343=ORIENTED_EDGE('',*,*,#6448,.T.);
#3344=ORIENTED_EDGE('',*,*,#6449,.T.);
#3345=ORIENTED_EDGE('',*,*,#6450,.T.);
#3346=ORIENTED_EDGE('',*,*,#6451,.T.);
#3347=ORIENTED_EDGE('',*,*,#6452,.T.);
#3348=ORIENTED_EDGE('',*,*,#6453,.T.);
#3349=ORIENTED_EDGE('',*,*,#6454,.T.);
#3350=ORIENTED_EDGE('',*,*,#6455,.T.);
#3351=ORIENTED_EDGE('',*,*,#6456,.T.);
#3352=ORIENTED_EDGE('',*,*,#6457,.T.);
#3353=ORIENTED_EDGE('',*,*,#6458,.T.);
#3354=ORIENTED_EDGE('',*,*,#6459,.T.);
#3355=ORIENTED_EDGE('',*,*,#6460,.T.);
#3356=ORIENTED_EDGE('',*,*,#6461,.T.);
#3357=ORIENTED_EDGE('',*,*,#6462,.T.);
#3358=ORIENTED_EDGE('',*,*,#6463,.T.);
#3359=ORIENTED_EDGE('',*,*,#6464,.T.);
#3360=ORIENTED_EDGE('',*,*,#6465,.T.);
#3361=ORIENTED_EDGE('',*,*,#6466,.T.);
#3362=ORIENTED_EDGE('',*,*,#6467,.T.);
#3363=ORIENTED_EDGE('',*,*,#6468,.T.);
#3364=ORIENTED_EDGE('',*,*,#6469,.T.);
#3365=ORIENTED_EDGE('',*,*,#6470,.T.);
#3366=ORIENTED_EDGE('',*,*,#6471,.T.);
#3367=ORIENTED_EDGE('',*,*,#6472,.T.);
#3368=ORIENTED_EDGE('',*,*,#6473,.T.);
#3369=ORIENTED_EDGE('',*,*,#6474,.T.);
#3370=ORIENTED_EDGE('',*,*,#6475,.T.);
#3371=ORIENTED_EDGE('',*,*,#6476,.T.);
#3372=ORIENTED_EDGE('',*,*,#6477,.T.);
#3373=ORIENTED_EDGE('',*,*,#6478,.T.);
#3374=ORIENTED_EDGE('',*,*,#6479,.T.);
#3375=ORIENTED_EDGE('',*,*,#6480,.T.);
#3376=ORIENTED_EDGE('',*,*,#6481,.T.);
#3377=ORIENTED_EDGE('',*,*,#6482,.T.);
#3378=ORIENTED_EDGE('',*,*,#6483,.T.);
#3379=ORIENTED_EDGE('',*,*,#6484,.T.);
#3380=ORIENTED_EDGE('',*,*,#6485,.T.);
#3381=ORIENTED_EDGE('',*,*,#6486,.T.);
#3382=ORIENTED_EDGE('',*,*,#6487,.T.);
#3383=ORIENTED_EDGE('',*,*,#6488,.T.);
#3384=ORIENTED_EDGE('',*,*,#6489,.T.);
#3385=ORIENTED_EDGE('',*,*,#6490,.T.);
#3386=ORIENTED_EDGE('',*,*,#6491,.T.);
#3387=ORIENTED_EDGE('',*,*,#6492,.T.);
#3388=ORIENTED_EDGE('',*,*,#6493,.T.);
#3389=ORIENTED_EDGE('',*,*,#6494,.T.);
#3390=ORIENTED_EDGE('',*,*,#6495,.T.);
#3391=ORIENTED_EDGE('',*,*,#6496,.T.);
#3392=ORIENTED_EDGE('',*,*,#6497,.T.);
#3393=ORIENTED_EDGE('',*,*,#6498,.T.);
#3394=ORIENTED_EDGE('',*,*,#6499,.F.);
#3395=ORIENTED_EDGE('',*,*,#6213,.T.);
#3396=ORIENTED_EDGE('',*,*,#6500,.F.);
#3397=ORIENTED_EDGE('',*,*,#6498,.F.);
#3398=ORIENTED_EDGE('',*,*,#6501,.T.);
#3399=ORIENTED_EDGE('',*,*,#6214,.T.);
#3400=ORIENTED_EDGE('',*,*,#6501,.F.);
#3401=ORIENTED_EDGE('',*,*,#6497,.F.);
#3402=ORIENTED_EDGE('',*,*,#6502,.T.);
#3403=ORIENTED_EDGE('',*,*,#6215,.T.);
#3404=ORIENTED_EDGE('',*,*,#6502,.F.);
#3405=ORIENTED_EDGE('',*,*,#6496,.F.);
#3406=ORIENTED_EDGE('',*,*,#6503,.T.);
#3407=ORIENTED_EDGE('',*,*,#6216,.T.);
#3408=ORIENTED_EDGE('',*,*,#6503,.F.);
#3409=ORIENTED_EDGE('',*,*,#6495,.F.);
#3410=ORIENTED_EDGE('',*,*,#6504,.T.);
#3411=ORIENTED_EDGE('',*,*,#6217,.T.);
#3412=ORIENTED_EDGE('',*,*,#6504,.F.);
#3413=ORIENTED_EDGE('',*,*,#6494,.F.);
#3414=ORIENTED_EDGE('',*,*,#6505,.T.);
#3415=ORIENTED_EDGE('',*,*,#6218,.T.);
#3416=ORIENTED_EDGE('',*,*,#6505,.F.);
#3417=ORIENTED_EDGE('',*,*,#6493,.F.);
#3418=ORIENTED_EDGE('',*,*,#6506,.T.);
#3419=ORIENTED_EDGE('',*,*,#6219,.T.);
#3420=ORIENTED_EDGE('',*,*,#6506,.F.);
#3421=ORIENTED_EDGE('',*,*,#6492,.F.);
#3422=ORIENTED_EDGE('',*,*,#6507,.T.);
#3423=ORIENTED_EDGE('',*,*,#6220,.T.);
#3424=ORIENTED_EDGE('',*,*,#6507,.F.);
#3425=ORIENTED_EDGE('',*,*,#6491,.F.);
#3426=ORIENTED_EDGE('',*,*,#6508,.T.);
#3427=ORIENTED_EDGE('',*,*,#6221,.T.);
#3428=ORIENTED_EDGE('',*,*,#6508,.F.);
#3429=ORIENTED_EDGE('',*,*,#6490,.F.);
#3430=ORIENTED_EDGE('',*,*,#6509,.T.);
#3431=ORIENTED_EDGE('',*,*,#6222,.T.);
#3432=ORIENTED_EDGE('',*,*,#6509,.F.);
#3433=ORIENTED_EDGE('',*,*,#6489,.F.);
#3434=ORIENTED_EDGE('',*,*,#6510,.T.);
#3435=ORIENTED_EDGE('',*,*,#6223,.T.);
#3436=ORIENTED_EDGE('',*,*,#6510,.F.);
#3437=ORIENTED_EDGE('',*,*,#6488,.F.);
#3438=ORIENTED_EDGE('',*,*,#6511,.T.);
#3439=ORIENTED_EDGE('',*,*,#6224,.T.);
#3440=ORIENTED_EDGE('',*,*,#6511,.F.);
#3441=ORIENTED_EDGE('',*,*,#6487,.F.);
#3442=ORIENTED_EDGE('',*,*,#6512,.T.);
#3443=ORIENTED_EDGE('',*,*,#6225,.T.);
#3444=ORIENTED_EDGE('',*,*,#6512,.F.);
#3445=ORIENTED_EDGE('',*,*,#6486,.F.);
#3446=ORIENTED_EDGE('',*,*,#6513,.T.);
#3447=ORIENTED_EDGE('',*,*,#6226,.T.);
#3448=ORIENTED_EDGE('',*,*,#6513,.F.);
#3449=ORIENTED_EDGE('',*,*,#6485,.F.);
#3450=ORIENTED_EDGE('',*,*,#6514,.T.);
#3451=ORIENTED_EDGE('',*,*,#6227,.T.);
#3452=ORIENTED_EDGE('',*,*,#6514,.F.);
#3453=ORIENTED_EDGE('',*,*,#6484,.F.);
#3454=ORIENTED_EDGE('',*,*,#6515,.T.);
#3455=ORIENTED_EDGE('',*,*,#6228,.T.);
#3456=ORIENTED_EDGE('',*,*,#6515,.F.);
#3457=ORIENTED_EDGE('',*,*,#6483,.F.);
#3458=ORIENTED_EDGE('',*,*,#6516,.T.);
#3459=ORIENTED_EDGE('',*,*,#6229,.T.);
#3460=ORIENTED_EDGE('',*,*,#6516,.F.);
#3461=ORIENTED_EDGE('',*,*,#6482,.F.);
#3462=ORIENTED_EDGE('',*,*,#6517,.T.);
#3463=ORIENTED_EDGE('',*,*,#6230,.T.);
#3464=ORIENTED_EDGE('',*,*,#6517,.F.);
#3465=ORIENTED_EDGE('',*,*,#6481,.F.);
#3466=ORIENTED_EDGE('',*,*,#6518,.T.);
#3467=ORIENTED_EDGE('',*,*,#6231,.T.);
#3468=ORIENTED_EDGE('',*,*,#6518,.F.);
#3469=ORIENTED_EDGE('',*,*,#6480,.F.);
#3470=ORIENTED_EDGE('',*,*,#6519,.T.);
#3471=ORIENTED_EDGE('',*,*,#6232,.T.);
#3472=ORIENTED_EDGE('',*,*,#6519,.F.);
#3473=ORIENTED_EDGE('',*,*,#6479,.F.);
#3474=ORIENTED_EDGE('',*,*,#6520,.T.);
#3475=ORIENTED_EDGE('',*,*,#6233,.T.);
#3476=ORIENTED_EDGE('',*,*,#6520,.F.);
#3477=ORIENTED_EDGE('',*,*,#6478,.F.);
#3478=ORIENTED_EDGE('',*,*,#6521,.T.);
#3479=ORIENTED_EDGE('',*,*,#6234,.T.);
#3480=ORIENTED_EDGE('',*,*,#6521,.F.);
#3481=ORIENTED_EDGE('',*,*,#6477,.F.);
#3482=ORIENTED_EDGE('',*,*,#6522,.T.);
#3483=ORIENTED_EDGE('',*,*,#6235,.T.);
#3484=ORIENTED_EDGE('',*,*,#6522,.F.);
#3485=ORIENTED_EDGE('',*,*,#6476,.F.);
#3486=ORIENTED_EDGE('',*,*,#6523,.T.);
#3487=ORIENTED_EDGE('',*,*,#6236,.T.);
#3488=ORIENTED_EDGE('',*,*,#6523,.F.);
#3489=ORIENTED_EDGE('',*,*,#6475,.F.);
#3490=ORIENTED_EDGE('',*,*,#6524,.T.);
#3491=ORIENTED_EDGE('',*,*,#6237,.T.);
#3492=ORIENTED_EDGE('',*,*,#6524,.F.);
#3493=ORIENTED_EDGE('',*,*,#6474,.F.);
#3494=ORIENTED_EDGE('',*,*,#6525,.T.);
#3495=ORIENTED_EDGE('',*,*,#6238,.T.);
#3496=ORIENTED_EDGE('',*,*,#6525,.F.);
#3497=ORIENTED_EDGE('',*,*,#6473,.F.);
#3498=ORIENTED_EDGE('',*,*,#6526,.T.);
#3499=ORIENTED_EDGE('',*,*,#6239,.T.);
#3500=ORIENTED_EDGE('',*,*,#6526,.F.);
#3501=ORIENTED_EDGE('',*,*,#6472,.F.);
#3502=ORIENTED_EDGE('',*,*,#6527,.T.);
#3503=ORIENTED_EDGE('',*,*,#6240,.T.);
#3504=ORIENTED_EDGE('',*,*,#6527,.F.);
#3505=ORIENTED_EDGE('',*,*,#6471,.F.);
#3506=ORIENTED_EDGE('',*,*,#6528,.T.);
#3507=ORIENTED_EDGE('',*,*,#6241,.T.);
#3508=ORIENTED_EDGE('',*,*,#6528,.F.);
#3509=ORIENTED_EDGE('',*,*,#6470,.F.);
#3510=ORIENTED_EDGE('',*,*,#6529,.T.);
#3511=ORIENTED_EDGE('',*,*,#6242,.T.);
#3512=ORIENTED_EDGE('',*,*,#6529,.F.);
#3513=ORIENTED_EDGE('',*,*,#6469,.F.);
#3514=ORIENTED_EDGE('',*,*,#6530,.T.);
#3515=ORIENTED_EDGE('',*,*,#6243,.T.);
#3516=ORIENTED_EDGE('',*,*,#6530,.F.);
#3517=ORIENTED_EDGE('',*,*,#6468,.F.);
#3518=ORIENTED_EDGE('',*,*,#6531,.T.);
#3519=ORIENTED_EDGE('',*,*,#6244,.T.);
#3520=ORIENTED_EDGE('',*,*,#6531,.F.);
#3521=ORIENTED_EDGE('',*,*,#6467,.F.);
#3522=ORIENTED_EDGE('',*,*,#6532,.T.);
#3523=ORIENTED_EDGE('',*,*,#6245,.T.);
#3524=ORIENTED_EDGE('',*,*,#6532,.F.);
#3525=ORIENTED_EDGE('',*,*,#6466,.F.);
#3526=ORIENTED_EDGE('',*,*,#6533,.T.);
#3527=ORIENTED_EDGE('',*,*,#6246,.T.);
#3528=ORIENTED_EDGE('',*,*,#6533,.F.);
#3529=ORIENTED_EDGE('',*,*,#6465,.F.);
#3530=ORIENTED_EDGE('',*,*,#6534,.T.);
#3531=ORIENTED_EDGE('',*,*,#6247,.T.);
#3532=ORIENTED_EDGE('',*,*,#6534,.F.);
#3533=ORIENTED_EDGE('',*,*,#6464,.F.);
#3534=ORIENTED_EDGE('',*,*,#6535,.T.);
#3535=ORIENTED_EDGE('',*,*,#6248,.T.);
#3536=ORIENTED_EDGE('',*,*,#6535,.F.);
#3537=ORIENTED_EDGE('',*,*,#6463,.F.);
#3538=ORIENTED_EDGE('',*,*,#6536,.T.);
#3539=ORIENTED_EDGE('',*,*,#6249,.T.);
#3540=ORIENTED_EDGE('',*,*,#6536,.F.);
#3541=ORIENTED_EDGE('',*,*,#6462,.F.);
#3542=ORIENTED_EDGE('',*,*,#6537,.T.);
#3543=ORIENTED_EDGE('',*,*,#6250,.T.);
#3544=ORIENTED_EDGE('',*,*,#6537,.F.);
#3545=ORIENTED_EDGE('',*,*,#6461,.F.);
#3546=ORIENTED_EDGE('',*,*,#6538,.T.);
#3547=ORIENTED_EDGE('',*,*,#6251,.T.);
#3548=ORIENTED_EDGE('',*,*,#6538,.F.);
#3549=ORIENTED_EDGE('',*,*,#6460,.F.);
#3550=ORIENTED_EDGE('',*,*,#6539,.T.);
#3551=ORIENTED_EDGE('',*,*,#6252,.T.);
#3552=ORIENTED_EDGE('',*,*,#6539,.F.);
#3553=ORIENTED_EDGE('',*,*,#6459,.F.);
#3554=ORIENTED_EDGE('',*,*,#6540,.T.);
#3555=ORIENTED_EDGE('',*,*,#6253,.T.);
#3556=ORIENTED_EDGE('',*,*,#6540,.F.);
#3557=ORIENTED_EDGE('',*,*,#6458,.F.);
#3558=ORIENTED_EDGE('',*,*,#6541,.T.);
#3559=ORIENTED_EDGE('',*,*,#6254,.T.);
#3560=ORIENTED_EDGE('',*,*,#6541,.F.);
#3561=ORIENTED_EDGE('',*,*,#6457,.F.);
#3562=ORIENTED_EDGE('',*,*,#6542,.T.);
#3563=ORIENTED_EDGE('',*,*,#6255,.T.);
#3564=ORIENTED_EDGE('',*,*,#6542,.F.);
#3565=ORIENTED_EDGE('',*,*,#6456,.F.);
#3566=ORIENTED_EDGE('',*,*,#6543,.T.);
#3567=ORIENTED_EDGE('',*,*,#6256,.T.);
#3568=ORIENTED_EDGE('',*,*,#6543,.F.);
#3569=ORIENTED_EDGE('',*,*,#6455,.F.);
#3570=ORIENTED_EDGE('',*,*,#6544,.T.);
#3571=ORIENTED_EDGE('',*,*,#6257,.T.);
#3572=ORIENTED_EDGE('',*,*,#6544,.F.);
#3573=ORIENTED_EDGE('',*,*,#6454,.F.);
#3574=ORIENTED_EDGE('',*,*,#6545,.T.);
#3575=ORIENTED_EDGE('',*,*,#6258,.T.);
#3576=ORIENTED_EDGE('',*,*,#6545,.F.);
#3577=ORIENTED_EDGE('',*,*,#6453,.F.);
#3578=ORIENTED_EDGE('',*,*,#6546,.T.);
#3579=ORIENTED_EDGE('',*,*,#6259,.T.);
#3580=ORIENTED_EDGE('',*,*,#6546,.F.);
#3581=ORIENTED_EDGE('',*,*,#6452,.F.);
#3582=ORIENTED_EDGE('',*,*,#6547,.T.);
#3583=ORIENTED_EDGE('',*,*,#6260,.T.);
#3584=ORIENTED_EDGE('',*,*,#6547,.F.);
#3585=ORIENTED_EDGE('',*,*,#6451,.F.);
#3586=ORIENTED_EDGE('',*,*,#6548,.T.);
#3587=ORIENTED_EDGE('',*,*,#6261,.T.);
#3588=ORIENTED_EDGE('',*,*,#6548,.F.);
#3589=ORIENTED_EDGE('',*,*,#6450,.F.);
#3590=ORIENTED_EDGE('',*,*,#6549,.T.);
#3591=ORIENTED_EDGE('',*,*,#6262,.T.);
#3592=ORIENTED_EDGE('',*,*,#6549,.F.);
#3593=ORIENTED_EDGE('',*,*,#6449,.F.);
#3594=ORIENTED_EDGE('',*,*,#6550,.T.);
#3595=ORIENTED_EDGE('',*,*,#6263,.T.);
#3596=ORIENTED_EDGE('',*,*,#6550,.F.);
#3597=ORIENTED_EDGE('',*,*,#6448,.F.);
#3598=ORIENTED_EDGE('',*,*,#6551,.T.);
#3599=ORIENTED_EDGE('',*,*,#6264,.T.);
#3600=ORIENTED_EDGE('',*,*,#6551,.F.);
#3601=ORIENTED_EDGE('',*,*,#6447,.F.);
#3602=ORIENTED_EDGE('',*,*,#6552,.T.);
#3603=ORIENTED_EDGE('',*,*,#6265,.T.);
#3604=ORIENTED_EDGE('',*,*,#6552,.F.);
#3605=ORIENTED_EDGE('',*,*,#6446,.F.);
#3606=ORIENTED_EDGE('',*,*,#6553,.T.);
#3607=ORIENTED_EDGE('',*,*,#6266,.T.);
#3608=ORIENTED_EDGE('',*,*,#6553,.F.);
#3609=ORIENTED_EDGE('',*,*,#6445,.F.);
#3610=ORIENTED_EDGE('',*,*,#6554,.T.);
#3611=ORIENTED_EDGE('',*,*,#6267,.T.);
#3612=ORIENTED_EDGE('',*,*,#6554,.F.);
#3613=ORIENTED_EDGE('',*,*,#6444,.F.);
#3614=ORIENTED_EDGE('',*,*,#6555,.T.);
#3615=ORIENTED_EDGE('',*,*,#6268,.T.);
#3616=ORIENTED_EDGE('',*,*,#6555,.F.);
#3617=ORIENTED_EDGE('',*,*,#6443,.F.);
#3618=ORIENTED_EDGE('',*,*,#6556,.T.);
#3619=ORIENTED_EDGE('',*,*,#6269,.T.);
#3620=ORIENTED_EDGE('',*,*,#6556,.F.);
#3621=ORIENTED_EDGE('',*,*,#6442,.F.);
#3622=ORIENTED_EDGE('',*,*,#6557,.T.);
#3623=ORIENTED_EDGE('',*,*,#6270,.T.);
#3624=ORIENTED_EDGE('',*,*,#6557,.F.);
#3625=ORIENTED_EDGE('',*,*,#6441,.F.);
#3626=ORIENTED_EDGE('',*,*,#6558,.T.);
#3627=ORIENTED_EDGE('',*,*,#6271,.T.);
#3628=ORIENTED_EDGE('',*,*,#6558,.F.);
#3629=ORIENTED_EDGE('',*,*,#6440,.F.);
#3630=ORIENTED_EDGE('',*,*,#6559,.T.);
#3631=ORIENTED_EDGE('',*,*,#6272,.T.);
#3632=ORIENTED_EDGE('',*,*,#6559,.F.);
#3633=ORIENTED_EDGE('',*,*,#6439,.F.);
#3634=ORIENTED_EDGE('',*,*,#6560,.T.);
#3635=ORIENTED_EDGE('',*,*,#6273,.T.);
#3636=ORIENTED_EDGE('',*,*,#6560,.F.);
#3637=ORIENTED_EDGE('',*,*,#6438,.F.);
#3638=ORIENTED_EDGE('',*,*,#6561,.T.);
#3639=ORIENTED_EDGE('',*,*,#6274,.T.);
#3640=ORIENTED_EDGE('',*,*,#6561,.F.);
#3641=ORIENTED_EDGE('',*,*,#6437,.F.);
#3642=ORIENTED_EDGE('',*,*,#6562,.T.);
#3643=ORIENTED_EDGE('',*,*,#6275,.T.);
#3644=ORIENTED_EDGE('',*,*,#6562,.F.);
#3645=ORIENTED_EDGE('',*,*,#6436,.F.);
#3646=ORIENTED_EDGE('',*,*,#6563,.T.);
#3647=ORIENTED_EDGE('',*,*,#6276,.T.);
#3648=ORIENTED_EDGE('',*,*,#6563,.F.);
#3649=ORIENTED_EDGE('',*,*,#6435,.F.);
#3650=ORIENTED_EDGE('',*,*,#6564,.T.);
#3651=ORIENTED_EDGE('',*,*,#6277,.T.);
#3652=ORIENTED_EDGE('',*,*,#6564,.F.);
#3653=ORIENTED_EDGE('',*,*,#6434,.F.);
#3654=ORIENTED_EDGE('',*,*,#6565,.T.);
#3655=ORIENTED_EDGE('',*,*,#6278,.T.);
#3656=ORIENTED_EDGE('',*,*,#6565,.F.);
#3657=ORIENTED_EDGE('',*,*,#6433,.F.);
#3658=ORIENTED_EDGE('',*,*,#6566,.T.);
#3659=ORIENTED_EDGE('',*,*,#6279,.T.);
#3660=ORIENTED_EDGE('',*,*,#6566,.F.);
#3661=ORIENTED_EDGE('',*,*,#6432,.F.);
#3662=ORIENTED_EDGE('',*,*,#6567,.T.);
#3663=ORIENTED_EDGE('',*,*,#6280,.T.);
#3664=ORIENTED_EDGE('',*,*,#6567,.F.);
#3665=ORIENTED_EDGE('',*,*,#6431,.F.);
#3666=ORIENTED_EDGE('',*,*,#6568,.T.);
#3667=ORIENTED_EDGE('',*,*,#6281,.T.);
#3668=ORIENTED_EDGE('',*,*,#6568,.F.);
#3669=ORIENTED_EDGE('',*,*,#6430,.F.);
#3670=ORIENTED_EDGE('',*,*,#6569,.T.);
#3671=ORIENTED_EDGE('',*,*,#6282,.T.);
#3672=ORIENTED_EDGE('',*,*,#6569,.F.);
#3673=ORIENTED_EDGE('',*,*,#6429,.F.);
#3674=ORIENTED_EDGE('',*,*,#6570,.T.);
#3675=ORIENTED_EDGE('',*,*,#6283,.T.);
#3676=ORIENTED_EDGE('',*,*,#6570,.F.);
#3677=ORIENTED_EDGE('',*,*,#6428,.F.);
#3678=ORIENTED_EDGE('',*,*,#6571,.T.);
#3679=ORIENTED_EDGE('',*,*,#6284,.T.);
#3680=ORIENTED_EDGE('',*,*,#6571,.F.);
#3681=ORIENTED_EDGE('',*,*,#6427,.F.);
#3682=ORIENTED_EDGE('',*,*,#6572,.T.);
#3683=ORIENTED_EDGE('',*,*,#6285,.T.);
#3684=ORIENTED_EDGE('',*,*,#6572,.F.);
#3685=ORIENTED_EDGE('',*,*,#6426,.F.);
#3686=ORIENTED_EDGE('',*,*,#6573,.T.);
#3687=ORIENTED_EDGE('',*,*,#6286,.T.);
#3688=ORIENTED_EDGE('',*,*,#6573,.F.);
#3689=ORIENTED_EDGE('',*,*,#6425,.F.);
#3690=ORIENTED_EDGE('',*,*,#6574,.T.);
#3691=ORIENTED_EDGE('',*,*,#6287,.T.);
#3692=ORIENTED_EDGE('',*,*,#6574,.F.);
#3693=ORIENTED_EDGE('',*,*,#6424,.F.);
#3694=ORIENTED_EDGE('',*,*,#6575,.T.);
#3695=ORIENTED_EDGE('',*,*,#6288,.T.);
#3696=ORIENTED_EDGE('',*,*,#6575,.F.);
#3697=ORIENTED_EDGE('',*,*,#6423,.F.);
#3698=ORIENTED_EDGE('',*,*,#6576,.T.);
#3699=ORIENTED_EDGE('',*,*,#6289,.T.);
#3700=ORIENTED_EDGE('',*,*,#6576,.F.);
#3701=ORIENTED_EDGE('',*,*,#6422,.F.);
#3702=ORIENTED_EDGE('',*,*,#6577,.T.);
#3703=ORIENTED_EDGE('',*,*,#6290,.T.);
#3704=ORIENTED_EDGE('',*,*,#6577,.F.);
#3705=ORIENTED_EDGE('',*,*,#6421,.F.);
#3706=ORIENTED_EDGE('',*,*,#6578,.T.);
#3707=ORIENTED_EDGE('',*,*,#6291,.T.);
#3708=ORIENTED_EDGE('',*,*,#6578,.F.);
#3709=ORIENTED_EDGE('',*,*,#6420,.F.);
#3710=ORIENTED_EDGE('',*,*,#6579,.T.);
#3711=ORIENTED_EDGE('',*,*,#6292,.T.);
#3712=ORIENTED_EDGE('',*,*,#6579,.F.);
#3713=ORIENTED_EDGE('',*,*,#6419,.F.);
#3714=ORIENTED_EDGE('',*,*,#6580,.T.);
#3715=ORIENTED_EDGE('',*,*,#6293,.T.);
#3716=ORIENTED_EDGE('',*,*,#6580,.F.);
#3717=ORIENTED_EDGE('',*,*,#6418,.F.);
#3718=ORIENTED_EDGE('',*,*,#6581,.T.);
#3719=ORIENTED_EDGE('',*,*,#6294,.T.);
#3720=ORIENTED_EDGE('',*,*,#6581,.F.);
#3721=ORIENTED_EDGE('',*,*,#6417,.F.);
#3722=ORIENTED_EDGE('',*,*,#6582,.T.);
#3723=ORIENTED_EDGE('',*,*,#6295,.T.);
#3724=ORIENTED_EDGE('',*,*,#6582,.F.);
#3725=ORIENTED_EDGE('',*,*,#6416,.F.);
#3726=ORIENTED_EDGE('',*,*,#6583,.T.);
#3727=ORIENTED_EDGE('',*,*,#6296,.T.);
#3728=ORIENTED_EDGE('',*,*,#6583,.F.);
#3729=ORIENTED_EDGE('',*,*,#6415,.F.);
#3730=ORIENTED_EDGE('',*,*,#6584,.T.);
#3731=ORIENTED_EDGE('',*,*,#6297,.T.);
#3732=ORIENTED_EDGE('',*,*,#6584,.F.);
#3733=ORIENTED_EDGE('',*,*,#6414,.F.);
#3734=ORIENTED_EDGE('',*,*,#6585,.T.);
#3735=ORIENTED_EDGE('',*,*,#6298,.T.);
#3736=ORIENTED_EDGE('',*,*,#6585,.F.);
#3737=ORIENTED_EDGE('',*,*,#6413,.F.);
#3738=ORIENTED_EDGE('',*,*,#6586,.T.);
#3739=ORIENTED_EDGE('',*,*,#6299,.T.);
#3740=ORIENTED_EDGE('',*,*,#6586,.F.);
#3741=ORIENTED_EDGE('',*,*,#6412,.F.);
#3742=ORIENTED_EDGE('',*,*,#6587,.T.);
#3743=ORIENTED_EDGE('',*,*,#6300,.T.);
#3744=ORIENTED_EDGE('',*,*,#6587,.F.);
#3745=ORIENTED_EDGE('',*,*,#6411,.F.);
#3746=ORIENTED_EDGE('',*,*,#6588,.T.);
#3747=ORIENTED_EDGE('',*,*,#6301,.T.);
#3748=ORIENTED_EDGE('',*,*,#6588,.F.);
#3749=ORIENTED_EDGE('',*,*,#6410,.F.);
#3750=ORIENTED_EDGE('',*,*,#6589,.T.);
#3751=ORIENTED_EDGE('',*,*,#6302,.T.);
#3752=ORIENTED_EDGE('',*,*,#6589,.F.);
#3753=ORIENTED_EDGE('',*,*,#6409,.F.);
#3754=ORIENTED_EDGE('',*,*,#6590,.T.);
#3755=ORIENTED_EDGE('',*,*,#6303,.T.);
#3756=ORIENTED_EDGE('',*,*,#6590,.F.);
#3757=ORIENTED_EDGE('',*,*,#6408,.F.);
#3758=ORIENTED_EDGE('',*,*,#6591,.T.);
#3759=ORIENTED_EDGE('',*,*,#6304,.T.);
#3760=ORIENTED_EDGE('',*,*,#6591,.F.);
#3761=ORIENTED_EDGE('',*,*,#6407,.F.);
#3762=ORIENTED_EDGE('',*,*,#6592,.T.);
#3763=ORIENTED_EDGE('',*,*,#6305,.T.);
#3764=ORIENTED_EDGE('',*,*,#6592,.F.);
#3765=ORIENTED_EDGE('',*,*,#6406,.F.);
#3766=ORIENTED_EDGE('',*,*,#6593,.T.);
#3767=ORIENTED_EDGE('',*,*,#6306,.T.);
#3768=ORIENTED_EDGE('',*,*,#6593,.F.);
#3769=ORIENTED_EDGE('',*,*,#6405,.F.);
#3770=ORIENTED_EDGE('',*,*,#6594,.T.);
#3771=ORIENTED_EDGE('',*,*,#6307,.T.);
#3772=ORIENTED_EDGE('',*,*,#6594,.F.);
#3773=ORIENTED_EDGE('',*,*,#6404,.F.);
#3774=ORIENTED_EDGE('',*,*,#6595,.T.);
#3775=ORIENTED_EDGE('',*,*,#6308,.T.);
#3776=ORIENTED_EDGE('',*,*,#6595,.F.);
#3777=ORIENTED_EDGE('',*,*,#6403,.F.);
#3778=ORIENTED_EDGE('',*,*,#6596,.T.);
#3779=ORIENTED_EDGE('',*,*,#6309,.T.);
#3780=ORIENTED_EDGE('',*,*,#6596,.F.);
#3781=ORIENTED_EDGE('',*,*,#6402,.F.);
#3782=ORIENTED_EDGE('',*,*,#6597,.T.);
#3783=ORIENTED_EDGE('',*,*,#6310,.T.);
#3784=ORIENTED_EDGE('',*,*,#6597,.F.);
#3785=ORIENTED_EDGE('',*,*,#6401,.F.);
#3786=ORIENTED_EDGE('',*,*,#6598,.T.);
#3787=ORIENTED_EDGE('',*,*,#6311,.T.);
#3788=ORIENTED_EDGE('',*,*,#6598,.F.);
#3789=ORIENTED_EDGE('',*,*,#6400,.F.);
#3790=ORIENTED_EDGE('',*,*,#6599,.T.);
#3791=ORIENTED_EDGE('',*,*,#6312,.T.);
#3792=ORIENTED_EDGE('',*,*,#6599,.F.);
#3793=ORIENTED_EDGE('',*,*,#6399,.F.);
#3794=ORIENTED_EDGE('',*,*,#6600,.T.);
#3795=ORIENTED_EDGE('',*,*,#6313,.T.);
#3796=ORIENTED_EDGE('',*,*,#6600,.F.);
#3797=ORIENTED_EDGE('',*,*,#6398,.F.);
#3798=ORIENTED_EDGE('',*,*,#6601,.T.);
#3799=ORIENTED_EDGE('',*,*,#6314,.T.);
#3800=ORIENTED_EDGE('',*,*,#6601,.F.);
#3801=ORIENTED_EDGE('',*,*,#6397,.F.);
#3802=ORIENTED_EDGE('',*,*,#6602,.T.);
#3803=ORIENTED_EDGE('',*,*,#6315,.T.);
#3804=ORIENTED_EDGE('',*,*,#6602,.F.);
#3805=ORIENTED_EDGE('',*,*,#6396,.F.);
#3806=ORIENTED_EDGE('',*,*,#6603,.T.);
#3807=ORIENTED_EDGE('',*,*,#6316,.T.);
#3808=ORIENTED_EDGE('',*,*,#6603,.F.);
#3809=ORIENTED_EDGE('',*,*,#6395,.F.);
#3810=ORIENTED_EDGE('',*,*,#6604,.T.);
#3811=ORIENTED_EDGE('',*,*,#6317,.T.);
#3812=ORIENTED_EDGE('',*,*,#6604,.F.);
#3813=ORIENTED_EDGE('',*,*,#6394,.F.);
#3814=ORIENTED_EDGE('',*,*,#6605,.T.);
#3815=ORIENTED_EDGE('',*,*,#6318,.T.);
#3816=ORIENTED_EDGE('',*,*,#6605,.F.);
#3817=ORIENTED_EDGE('',*,*,#6393,.F.);
#3818=ORIENTED_EDGE('',*,*,#6606,.T.);
#3819=ORIENTED_EDGE('',*,*,#6319,.T.);
#3820=ORIENTED_EDGE('',*,*,#6606,.F.);
#3821=ORIENTED_EDGE('',*,*,#6392,.F.);
#3822=ORIENTED_EDGE('',*,*,#6607,.T.);
#3823=ORIENTED_EDGE('',*,*,#6320,.T.);
#3824=ORIENTED_EDGE('',*,*,#6607,.F.);
#3825=ORIENTED_EDGE('',*,*,#6391,.F.);
#3826=ORIENTED_EDGE('',*,*,#6608,.T.);
#3827=ORIENTED_EDGE('',*,*,#6321,.T.);
#3828=ORIENTED_EDGE('',*,*,#6608,.F.);
#3829=ORIENTED_EDGE('',*,*,#6390,.F.);
#3830=ORIENTED_EDGE('',*,*,#6609,.T.);
#3831=ORIENTED_EDGE('',*,*,#6322,.T.);
#3832=ORIENTED_EDGE('',*,*,#6609,.F.);
#3833=ORIENTED_EDGE('',*,*,#6389,.F.);
#3834=ORIENTED_EDGE('',*,*,#6610,.T.);
#3835=ORIENTED_EDGE('',*,*,#6323,.T.);
#3836=ORIENTED_EDGE('',*,*,#6610,.F.);
#3837=ORIENTED_EDGE('',*,*,#6388,.F.);
#3838=ORIENTED_EDGE('',*,*,#6611,.T.);
#3839=ORIENTED_EDGE('',*,*,#6324,.T.);
#3840=ORIENTED_EDGE('',*,*,#6611,.F.);
#3841=ORIENTED_EDGE('',*,*,#6387,.F.);
#3842=ORIENTED_EDGE('',*,*,#6612,.T.);
#3843=ORIENTED_EDGE('',*,*,#6325,.T.);
#3844=ORIENTED_EDGE('',*,*,#6612,.F.);
#3845=ORIENTED_EDGE('',*,*,#6386,.F.);
#3846=ORIENTED_EDGE('',*,*,#6613,.T.);
#3847=ORIENTED_EDGE('',*,*,#6326,.T.);
#3848=ORIENTED_EDGE('',*,*,#6613,.F.);
#3849=ORIENTED_EDGE('',*,*,#6385,.F.);
#3850=ORIENTED_EDGE('',*,*,#6614,.T.);
#3851=ORIENTED_EDGE('',*,*,#6327,.T.);
#3852=ORIENTED_EDGE('',*,*,#6614,.F.);
#3853=ORIENTED_EDGE('',*,*,#6384,.F.);
#3854=ORIENTED_EDGE('',*,*,#6615,.T.);
#3855=ORIENTED_EDGE('',*,*,#6328,.T.);
#3856=ORIENTED_EDGE('',*,*,#6615,.F.);
#3857=ORIENTED_EDGE('',*,*,#6383,.F.);
#3858=ORIENTED_EDGE('',*,*,#6616,.T.);
#3859=ORIENTED_EDGE('',*,*,#6329,.T.);
#3860=ORIENTED_EDGE('',*,*,#6616,.F.);
#3861=ORIENTED_EDGE('',*,*,#6382,.F.);
#3862=ORIENTED_EDGE('',*,*,#6617,.T.);
#3863=ORIENTED_EDGE('',*,*,#6330,.T.);
#3864=ORIENTED_EDGE('',*,*,#6617,.F.);
#3865=ORIENTED_EDGE('',*,*,#6381,.F.);
#3866=ORIENTED_EDGE('',*,*,#6618,.T.);
#3867=ORIENTED_EDGE('',*,*,#6331,.T.);
#3868=ORIENTED_EDGE('',*,*,#6618,.F.);
#3869=ORIENTED_EDGE('',*,*,#6380,.F.);
#3870=ORIENTED_EDGE('',*,*,#6619,.T.);
#3871=ORIENTED_EDGE('',*,*,#6332,.T.);
#3872=ORIENTED_EDGE('',*,*,#6619,.F.);
#3873=ORIENTED_EDGE('',*,*,#6379,.F.);
#3874=ORIENTED_EDGE('',*,*,#6620,.T.);
#3875=ORIENTED_EDGE('',*,*,#6333,.T.);
#3876=ORIENTED_EDGE('',*,*,#6620,.F.);
#3877=ORIENTED_EDGE('',*,*,#6378,.F.);
#3878=ORIENTED_EDGE('',*,*,#6621,.T.);
#3879=ORIENTED_EDGE('',*,*,#6334,.T.);
#3880=ORIENTED_EDGE('',*,*,#6621,.F.);
#3881=ORIENTED_EDGE('',*,*,#6377,.F.);
#3882=ORIENTED_EDGE('',*,*,#6622,.T.);
#3883=ORIENTED_EDGE('',*,*,#6335,.T.);
#3884=ORIENTED_EDGE('',*,*,#6622,.F.);
#3885=ORIENTED_EDGE('',*,*,#6376,.F.);
#3886=ORIENTED_EDGE('',*,*,#6623,.T.);
#3887=ORIENTED_EDGE('',*,*,#6336,.T.);
#3888=ORIENTED_EDGE('',*,*,#6623,.F.);
#3889=ORIENTED_EDGE('',*,*,#6375,.F.);
#3890=ORIENTED_EDGE('',*,*,#6624,.T.);
#3891=ORIENTED_EDGE('',*,*,#6337,.T.);
#3892=ORIENTED_EDGE('',*,*,#6624,.F.);
#3893=ORIENTED_EDGE('',*,*,#6374,.F.);
#3894=ORIENTED_EDGE('',*,*,#6625,.T.);
#3895=ORIENTED_EDGE('',*,*,#6338,.T.);
#3896=ORIENTED_EDGE('',*,*,#6625,.F.);
#3897=ORIENTED_EDGE('',*,*,#6373,.F.);
#3898=ORIENTED_EDGE('',*,*,#6626,.T.);
#3899=ORIENTED_EDGE('',*,*,#6339,.T.);
#3900=ORIENTED_EDGE('',*,*,#6626,.F.);
#3901=ORIENTED_EDGE('',*,*,#6372,.F.);
#3902=ORIENTED_EDGE('',*,*,#6627,.T.);
#3903=ORIENTED_EDGE('',*,*,#6340,.T.);
#3904=ORIENTED_EDGE('',*,*,#6627,.F.);
#3905=ORIENTED_EDGE('',*,*,#6371,.F.);
#3906=ORIENTED_EDGE('',*,*,#6628,.T.);
#3907=ORIENTED_EDGE('',*,*,#6341,.T.);
#3908=ORIENTED_EDGE('',*,*,#6628,.F.);
#3909=ORIENTED_EDGE('',*,*,#6370,.F.);
#3910=ORIENTED_EDGE('',*,*,#6629,.T.);
#3911=ORIENTED_EDGE('',*,*,#6342,.T.);
#3912=ORIENTED_EDGE('',*,*,#6629,.F.);
#3913=ORIENTED_EDGE('',*,*,#6369,.F.);
#3914=ORIENTED_EDGE('',*,*,#6630,.T.);
#3915=ORIENTED_EDGE('',*,*,#6343,.T.);
#3916=ORIENTED_EDGE('',*,*,#6630,.F.);
#3917=ORIENTED_EDGE('',*,*,#6368,.F.);
#3918=ORIENTED_EDGE('',*,*,#6631,.T.);
#3919=ORIENTED_EDGE('',*,*,#6344,.T.);
#3920=ORIENTED_EDGE('',*,*,#6631,.F.);
#3921=ORIENTED_EDGE('',*,*,#6367,.F.);
#3922=ORIENTED_EDGE('',*,*,#6632,.T.);
#3923=ORIENTED_EDGE('',*,*,#6345,.T.);
#3924=ORIENTED_EDGE('',*,*,#6632,.F.);
#3925=ORIENTED_EDGE('',*,*,#6366,.F.);
#3926=ORIENTED_EDGE('',*,*,#6633,.T.);
#3927=ORIENTED_EDGE('',*,*,#6346,.T.);
#3928=ORIENTED_EDGE('',*,*,#6633,.F.);
#3929=ORIENTED_EDGE('',*,*,#6365,.F.);
#3930=ORIENTED_EDGE('',*,*,#6634,.T.);
#3931=ORIENTED_EDGE('',*,*,#6347,.T.);
#3932=ORIENTED_EDGE('',*,*,#6634,.F.);
#3933=ORIENTED_EDGE('',*,*,#6364,.F.);
#3934=ORIENTED_EDGE('',*,*,#6635,.T.);
#3935=ORIENTED_EDGE('',*,*,#6348,.T.);
#3936=ORIENTED_EDGE('',*,*,#6635,.F.);
#3937=ORIENTED_EDGE('',*,*,#6363,.F.);
#3938=ORIENTED_EDGE('',*,*,#6636,.T.);
#3939=ORIENTED_EDGE('',*,*,#6349,.T.);
#3940=ORIENTED_EDGE('',*,*,#6636,.F.);
#3941=ORIENTED_EDGE('',*,*,#6362,.F.);
#3942=ORIENTED_EDGE('',*,*,#6637,.T.);
#3943=ORIENTED_EDGE('',*,*,#6350,.T.);
#3944=ORIENTED_EDGE('',*,*,#6637,.F.);
#3945=ORIENTED_EDGE('',*,*,#6361,.F.);
#3946=ORIENTED_EDGE('',*,*,#6638,.T.);
#3947=ORIENTED_EDGE('',*,*,#6351,.T.);
#3948=ORIENTED_EDGE('',*,*,#6638,.F.);
#3949=ORIENTED_EDGE('',*,*,#6360,.F.);
#3950=ORIENTED_EDGE('',*,*,#6639,.T.);
#3951=ORIENTED_EDGE('',*,*,#6352,.T.);
#3952=ORIENTED_EDGE('',*,*,#6639,.F.);
#3953=ORIENTED_EDGE('',*,*,#6359,.F.);
#3954=ORIENTED_EDGE('',*,*,#6640,.T.);
#3955=ORIENTED_EDGE('',*,*,#6353,.T.);
#3956=ORIENTED_EDGE('',*,*,#6640,.F.);
#3957=ORIENTED_EDGE('',*,*,#6358,.F.);
#3958=ORIENTED_EDGE('',*,*,#6641,.T.);
#3959=ORIENTED_EDGE('',*,*,#6354,.T.);
#3960=ORIENTED_EDGE('',*,*,#6641,.F.);
#3961=ORIENTED_EDGE('',*,*,#6357,.F.);
#3962=ORIENTED_EDGE('',*,*,#6642,.T.);
#3963=ORIENTED_EDGE('',*,*,#6212,.T.);
#3964=ORIENTED_EDGE('',*,*,#6642,.F.);
#3965=ORIENTED_EDGE('',*,*,#6356,.F.);
#3966=ORIENTED_EDGE('',*,*,#6500,.T.);
#3967=ORIENTED_EDGE('',*,*,#6183,.T.);
#3968=ORIENTED_EDGE('',*,*,#6207,.T.);
#3969=ORIENTED_EDGE('',*,*,#6643,.F.);
#3970=ORIENTED_EDGE('',*,*,#6644,.T.);
#3971=ORIENTED_EDGE('',*,*,#6185,.T.);
#3972=ORIENTED_EDGE('',*,*,#6184,.T.);
#3973=ORIENTED_EDGE('',*,*,#6643,.T.);
#3974=ORIENTED_EDGE('',*,*,#6208,.F.);
#3975=ORIENTED_EDGE('',*,*,#6202,.F.);
#3976=ORIENTED_EDGE('',*,*,#6201,.F.);
#3977=ORIENTED_EDGE('',*,*,#6200,.F.);
#3978=ORIENTED_EDGE('',*,*,#6199,.F.);
#3979=ORIENTED_EDGE('',*,*,#6198,.F.);
#3980=ORIENTED_EDGE('',*,*,#6197,.F.);
#3981=ORIENTED_EDGE('',*,*,#6196,.F.);
#3982=ORIENTED_EDGE('',*,*,#6195,.F.);
#3983=ORIENTED_EDGE('',*,*,#6210,.F.);
#3984=ORIENTED_EDGE('',*,*,#6209,.F.);
#3985=ORIENTED_EDGE('',*,*,#6190,.T.);
#3986=ORIENTED_EDGE('',*,*,#6189,.T.);
#3987=ORIENTED_EDGE('',*,*,#6188,.T.);
#3988=ORIENTED_EDGE('',*,*,#6187,.T.);
#3989=ORIENTED_EDGE('',*,*,#6186,.T.);
#3990=ORIENTED_EDGE('',*,*,#6499,.T.);
#3991=ORIENTED_EDGE('',*,*,#6644,.F.);
#3992=ORIENTED_EDGE('',*,*,#6355,.T.);
#3993=ORIENTED_EDGE('',*,*,#6645,.T.);
#3994=ORIENTED_EDGE('',*,*,#6181,.T.);
#3995=ORIENTED_EDGE('',*,*,#6646,.T.);
#3996=ORIENTED_EDGE('',*,*,#6646,.F.);
#3997=ORIENTED_EDGE('',*,*,#6211,.F.);
#3998=ORIENTED_EDGE('',*,*,#6645,.F.);
#3999=ORIENTED_EDGE('',*,*,#6182,.T.);
#4000=ORIENTED_EDGE('',*,*,#6647,.F.);
#4001=ORIENTED_EDGE('',*,*,#6648,.T.);
#4002=ORIENTED_EDGE('',*,*,#6649,.F.);
#4003=ORIENTED_EDGE('',*,*,#6650,.T.);
#4004=ORIENTED_EDGE('',*,*,#6648,.F.);
#4005=ORIENTED_EDGE('',*,*,#6649,.T.);
#4006=ORIENTED_EDGE('',*,*,#6647,.T.);
#4007=ORIENTED_EDGE('',*,*,#6650,.F.);
#4008=ORIENTED_EDGE('',*,*,#6651,.T.);
#4009=ORIENTED_EDGE('',*,*,#6652,.F.);
#4010=ORIENTED_EDGE('',*,*,#6653,.F.);
#4011=ORIENTED_EDGE('',*,*,#6654,.T.);
#4012=ORIENTED_EDGE('',*,*,#6652,.T.);
#4013=ORIENTED_EDGE('',*,*,#6654,.F.);
#4014=ORIENTED_EDGE('',*,*,#6651,.F.);
#4015=ORIENTED_EDGE('',*,*,#6653,.T.);
#4016=ORIENTED_EDGE('',*,*,#6655,.F.);
#4017=ORIENTED_EDGE('',*,*,#6656,.F.);
#4018=ORIENTED_EDGE('',*,*,#6657,.F.);
#4019=ORIENTED_EDGE('',*,*,#6658,.F.);
#4020=ORIENTED_EDGE('',*,*,#6659,.F.);
#4021=ORIENTED_EDGE('',*,*,#6660,.F.);
#4022=ORIENTED_EDGE('',*,*,#6657,.T.);
#4023=ORIENTED_EDGE('',*,*,#6661,.T.);
#4024=ORIENTED_EDGE('',*,*,#6662,.F.);
#4025=ORIENTED_EDGE('',*,*,#6663,.F.);
#4026=ORIENTED_EDGE('',*,*,#6655,.T.);
#4027=ORIENTED_EDGE('',*,*,#6664,.T.);
#4028=ORIENTED_EDGE('',*,*,#6665,.F.);
#4029=ORIENTED_EDGE('',*,*,#6666,.F.);
#4030=ORIENTED_EDGE('',*,*,#6667,.F.);
#4031=ORIENTED_EDGE('',*,*,#6668,.F.);
#4032=ORIENTED_EDGE('',*,*,#6669,.F.);
#4033=ORIENTED_EDGE('',*,*,#6670,.F.);
#4034=ORIENTED_EDGE('',*,*,#6668,.T.);
#4035=ORIENTED_EDGE('',*,*,#6671,.T.);
#4036=ORIENTED_EDGE('',*,*,#6672,.F.);
#4037=ORIENTED_EDGE('',*,*,#6673,.F.);
#4038=ORIENTED_EDGE('',*,*,#6666,.T.);
#4039=ORIENTED_EDGE('',*,*,#6674,.T.);
#4040=ORIENTED_EDGE('',*,*,#6675,.T.);
#4041=ORIENTED_EDGE('',*,*,#6676,.F.);
#4042=ORIENTED_EDGE('',*,*,#6677,.T.);
#4043=ORIENTED_EDGE('',*,*,#6662,.T.);
#4044=ORIENTED_EDGE('',*,*,#6678,.T.);
#4045=ORIENTED_EDGE('',*,*,#6659,.T.);
#4046=ORIENTED_EDGE('',*,*,#6679,.F.);
#4047=ORIENTED_EDGE('',*,*,#6680,.T.);
#4048=ORIENTED_EDGE('',*,*,#6672,.T.);
#4049=ORIENTED_EDGE('',*,*,#6681,.T.);
#4050=ORIENTED_EDGE('',*,*,#6669,.T.);
#4051=ORIENTED_EDGE('',*,*,#6682,.T.);
#4052=ORIENTED_EDGE('',*,*,#6680,.F.);
#4053=ORIENTED_EDGE('',*,*,#6676,.T.);
#4054=ORIENTED_EDGE('',*,*,#6679,.T.);
#4055=ORIENTED_EDGE('',*,*,#6675,.F.);
#4056=ORIENTED_EDGE('',*,*,#6665,.T.);
#4057=ORIENTED_EDGE('',*,*,#6670,.T.);
#4058=ORIENTED_EDGE('',*,*,#6681,.F.);
#4059=ORIENTED_EDGE('',*,*,#6674,.F.);
#4060=ORIENTED_EDGE('',*,*,#6667,.T.);
#4061=ORIENTED_EDGE('',*,*,#6673,.T.);
#4062=ORIENTED_EDGE('',*,*,#6682,.F.);
#4063=ORIENTED_EDGE('',*,*,#6671,.F.);
#4064=ORIENTED_EDGE('',*,*,#6656,.T.);
#4065=ORIENTED_EDGE('',*,*,#6663,.T.);
#4066=ORIENTED_EDGE('',*,*,#6677,.F.);
#4067=ORIENTED_EDGE('',*,*,#6661,.F.);
#4068=ORIENTED_EDGE('',*,*,#6658,.T.);
#4069=ORIENTED_EDGE('',*,*,#6660,.T.);
#4070=ORIENTED_EDGE('',*,*,#6678,.F.);
#4071=ORIENTED_EDGE('',*,*,#6664,.F.);
#4072=ORIENTED_EDGE('',*,*,#6683,.T.);
#4073=ORIENTED_EDGE('',*,*,#6684,.T.);
#4074=ORIENTED_EDGE('',*,*,#6685,.F.);
#4075=ORIENTED_EDGE('',*,*,#6686,.F.);
#4076=ORIENTED_EDGE('',*,*,#6685,.T.);
#4077=ORIENTED_EDGE('',*,*,#6687,.T.);
#4078=ORIENTED_EDGE('',*,*,#6688,.F.);
#4079=ORIENTED_EDGE('',*,*,#6689,.F.);
#4080=ORIENTED_EDGE('',*,*,#6688,.T.);
#4081=ORIENTED_EDGE('',*,*,#6690,.T.);
#4082=ORIENTED_EDGE('',*,*,#6691,.F.);
#4083=ORIENTED_EDGE('',*,*,#6692,.F.);
#4084=ORIENTED_EDGE('',*,*,#6693,.T.);
#4085=ORIENTED_EDGE('',*,*,#6694,.T.);
#4086=ORIENTED_EDGE('',*,*,#6695,.F.);
#4087=ORIENTED_EDGE('',*,*,#6696,.F.);
#4088=ORIENTED_EDGE('',*,*,#6697,.T.);
#4089=ORIENTED_EDGE('',*,*,#6698,.T.);
#4090=ORIENTED_EDGE('',*,*,#6699,.F.);
#4091=ORIENTED_EDGE('',*,*,#6700,.F.);
#4092=ORIENTED_EDGE('',*,*,#6699,.T.);
#4093=ORIENTED_EDGE('',*,*,#6701,.T.);
#4094=ORIENTED_EDGE('',*,*,#6693,.F.);
#4095=ORIENTED_EDGE('',*,*,#6702,.F.);
#4096=ORIENTED_EDGE('',*,*,#6703,.T.);
#4097=ORIENTED_EDGE('',*,*,#6704,.T.);
#4098=ORIENTED_EDGE('',*,*,#6705,.F.);
#4099=ORIENTED_EDGE('',*,*,#6706,.F.);
#4100=ORIENTED_EDGE('',*,*,#6707,.T.);
#4101=ORIENTED_EDGE('',*,*,#6708,.T.);
#4102=ORIENTED_EDGE('',*,*,#6709,.F.);
#4103=ORIENTED_EDGE('',*,*,#6710,.F.);
#4104=ORIENTED_EDGE('',*,*,#6709,.T.);
#4105=ORIENTED_EDGE('',*,*,#6711,.T.);
#4106=ORIENTED_EDGE('',*,*,#6703,.F.);
#4107=ORIENTED_EDGE('',*,*,#6712,.F.);
#4108=ORIENTED_EDGE('',*,*,#6713,.T.);
#4109=ORIENTED_EDGE('',*,*,#6714,.F.);
#4110=ORIENTED_EDGE('',*,*,#6715,.T.);
#4111=ORIENTED_EDGE('',*,*,#6716,.F.);
#4112=ORIENTED_EDGE('',*,*,#6717,.T.);
#4113=ORIENTED_EDGE('',*,*,#6718,.F.);
#4114=ORIENTED_EDGE('',*,*,#6719,.F.);
#4115=ORIENTED_EDGE('',*,*,#6720,.F.);
#4116=ORIENTED_EDGE('',*,*,#6721,.F.);
#4117=ORIENTED_EDGE('',*,*,#6711,.F.);
#4118=ORIENTED_EDGE('',*,*,#6708,.F.);
#4119=ORIENTED_EDGE('',*,*,#6722,.F.);
#4120=ORIENTED_EDGE('',*,*,#6704,.F.);
#4121=ORIENTED_EDGE('',*,*,#6701,.F.);
#4122=ORIENTED_EDGE('',*,*,#6698,.F.);
#4123=ORIENTED_EDGE('',*,*,#6723,.F.);
#4124=ORIENTED_EDGE('',*,*,#6694,.F.);
#4125=ORIENTED_EDGE('',*,*,#6724,.F.);
#4126=ORIENTED_EDGE('',*,*,#6690,.F.);
#4127=ORIENTED_EDGE('',*,*,#6687,.F.);
#4128=ORIENTED_EDGE('',*,*,#6684,.F.);
#4129=ORIENTED_EDGE('',*,*,#6725,.T.);
#4130=ORIENTED_EDGE('',*,*,#6726,.T.);
#4131=ORIENTED_EDGE('',*,*,#6727,.T.);
#4132=ORIENTED_EDGE('',*,*,#6728,.T.);
#4133=ORIENTED_EDGE('',*,*,#6729,.T.);
#4134=ORIENTED_EDGE('',*,*,#6710,.T.);
#4135=ORIENTED_EDGE('',*,*,#6712,.T.);
#4136=ORIENTED_EDGE('',*,*,#6706,.T.);
#4137=ORIENTED_EDGE('',*,*,#6730,.T.);
#4138=ORIENTED_EDGE('',*,*,#6700,.T.);
#4139=ORIENTED_EDGE('',*,*,#6702,.T.);
#4140=ORIENTED_EDGE('',*,*,#6696,.T.);
#4141=ORIENTED_EDGE('',*,*,#6731,.T.);
#4142=ORIENTED_EDGE('',*,*,#6692,.T.);
#4143=ORIENTED_EDGE('',*,*,#6732,.T.);
#4144=ORIENTED_EDGE('',*,*,#6686,.T.);
#4145=ORIENTED_EDGE('',*,*,#6689,.T.);
#4146=ORIENTED_EDGE('',*,*,#6733,.T.);
#4147=ORIENTED_EDGE('',*,*,#6734,.T.);
#4148=ORIENTED_EDGE('',*,*,#6735,.T.);
#4149=ORIENTED_EDGE('',*,*,#6736,.T.);
#4150=ORIENTED_EDGE('',*,*,#6737,.T.);
#4151=ORIENTED_EDGE('',*,*,#6738,.T.);
#4152=ORIENTED_EDGE('',*,*,#6718,.T.);
#4153=ORIENTED_EDGE('',*,*,#6727,.F.);
#4154=ORIENTED_EDGE('',*,*,#6719,.T.);
#4155=ORIENTED_EDGE('',*,*,#6717,.F.);
#4156=ORIENTED_EDGE('',*,*,#6716,.T.);
#4157=ORIENTED_EDGE('',*,*,#6728,.F.);
#4158=ORIENTED_EDGE('',*,*,#6720,.T.);
#4159=ORIENTED_EDGE('',*,*,#6715,.F.);
#4160=ORIENTED_EDGE('',*,*,#6714,.T.);
#4161=ORIENTED_EDGE('',*,*,#6729,.F.);
#4162=ORIENTED_EDGE('',*,*,#6721,.T.);
#4163=ORIENTED_EDGE('',*,*,#6713,.F.);
#4164=ORIENTED_EDGE('',*,*,#6730,.F.);
#4165=ORIENTED_EDGE('',*,*,#6705,.T.);
#4166=ORIENTED_EDGE('',*,*,#6722,.T.);
#4167=ORIENTED_EDGE('',*,*,#6707,.F.);
#4168=ORIENTED_EDGE('',*,*,#6731,.F.);
#4169=ORIENTED_EDGE('',*,*,#6695,.T.);
#4170=ORIENTED_EDGE('',*,*,#6723,.T.);
#4171=ORIENTED_EDGE('',*,*,#6697,.F.);
#4172=ORIENTED_EDGE('',*,*,#6732,.F.);
#4173=ORIENTED_EDGE('',*,*,#6691,.T.);
#4174=ORIENTED_EDGE('',*,*,#6724,.T.);
#4175=ORIENTED_EDGE('',*,*,#6683,.F.);
#4176=ORIENTED_EDGE('',*,*,#6734,.F.);
#4177=ORIENTED_EDGE('',*,*,#6738,.F.);
#4178=ORIENTED_EDGE('',*,*,#6736,.F.);
#4179=ORIENTED_EDGE('',*,*,#6733,.F.);
#4180=ORIENTED_EDGE('',*,*,#6726,.F.);
#4181=ORIENTED_EDGE('',*,*,#6735,.F.);
#4182=ORIENTED_EDGE('',*,*,#6737,.F.);
#4183=ORIENTED_EDGE('',*,*,#6725,.F.);
#4184=ORIENTED_EDGE('',*,*,#6739,.T.);
#4185=ORIENTED_EDGE('',*,*,#6740,.T.);
#4186=ORIENTED_EDGE('',*,*,#6741,.T.);
#4187=ORIENTED_EDGE('',*,*,#6742,.T.);
#4188=ORIENTED_EDGE('',*,*,#6742,.F.);
#4189=ORIENTED_EDGE('',*,*,#6743,.T.);
#4190=ORIENTED_EDGE('',*,*,#6744,.F.);
#4191=ORIENTED_EDGE('',*,*,#6745,.F.);
#4192=ORIENTED_EDGE('',*,*,#6740,.F.);
#4193=ORIENTED_EDGE('',*,*,#6746,.T.);
#4194=ORIENTED_EDGE('',*,*,#6747,.F.);
#4195=ORIENTED_EDGE('',*,*,#6748,.F.);
#4196=ORIENTED_EDGE('',*,*,#6739,.F.);
#4197=ORIENTED_EDGE('',*,*,#6745,.T.);
#4198=ORIENTED_EDGE('',*,*,#6749,.F.);
#4199=ORIENTED_EDGE('',*,*,#6746,.F.);
#4200=ORIENTED_EDGE('',*,*,#6750,.T.);
#4201=ORIENTED_EDGE('',*,*,#6751,.T.);
#4202=ORIENTED_EDGE('',*,*,#6752,.T.);
#4203=ORIENTED_EDGE('',*,*,#6753,.T.);
#4204=ORIENTED_EDGE('',*,*,#6753,.F.);
#4205=ORIENTED_EDGE('',*,*,#6754,.T.);
#4206=ORIENTED_EDGE('',*,*,#6755,.F.);
#4207=ORIENTED_EDGE('',*,*,#6756,.F.);
#4208=ORIENTED_EDGE('',*,*,#6751,.F.);
#4209=ORIENTED_EDGE('',*,*,#6757,.T.);
#4210=ORIENTED_EDGE('',*,*,#6758,.F.);
#4211=ORIENTED_EDGE('',*,*,#6759,.F.);
#4212=ORIENTED_EDGE('',*,*,#6750,.F.);
#4213=ORIENTED_EDGE('',*,*,#6756,.T.);
#4214=ORIENTED_EDGE('',*,*,#6760,.F.);
#4215=ORIENTED_EDGE('',*,*,#6757,.F.);
#4216=ORIENTED_EDGE('',*,*,#6761,.T.);
#4217=ORIENTED_EDGE('',*,*,#6762,.T.);
#4218=ORIENTED_EDGE('',*,*,#6763,.T.);
#4219=ORIENTED_EDGE('',*,*,#6764,.T.);
#4220=ORIENTED_EDGE('',*,*,#6764,.F.);
#4221=ORIENTED_EDGE('',*,*,#6765,.T.);
#4222=ORIENTED_EDGE('',*,*,#6766,.F.);
#4223=ORIENTED_EDGE('',*,*,#6767,.F.);
#4224=ORIENTED_EDGE('',*,*,#6762,.F.);
#4225=ORIENTED_EDGE('',*,*,#6768,.T.);
#4226=ORIENTED_EDGE('',*,*,#6769,.F.);
#4227=ORIENTED_EDGE('',*,*,#6770,.F.);
#4228=ORIENTED_EDGE('',*,*,#6761,.F.);
#4229=ORIENTED_EDGE('',*,*,#6767,.T.);
#4230=ORIENTED_EDGE('',*,*,#6771,.F.);
#4231=ORIENTED_EDGE('',*,*,#6768,.F.);
#4232=ORIENTED_EDGE('',*,*,#6772,.T.);
#4233=ORIENTED_EDGE('',*,*,#6773,.F.);
#4234=ORIENTED_EDGE('',*,*,#6769,.T.);
#4235=ORIENTED_EDGE('',*,*,#6771,.T.);
#4236=ORIENTED_EDGE('',*,*,#6766,.T.);
#4237=ORIENTED_EDGE('',*,*,#6774,.T.);
#4238=ORIENTED_EDGE('',*,*,#6758,.T.);
#4239=ORIENTED_EDGE('',*,*,#6760,.T.);
#4240=ORIENTED_EDGE('',*,*,#6755,.T.);
#4241=ORIENTED_EDGE('',*,*,#6775,.T.);
#4242=ORIENTED_EDGE('',*,*,#6747,.T.);
#4243=ORIENTED_EDGE('',*,*,#6749,.T.);
#4244=ORIENTED_EDGE('',*,*,#6744,.T.);
#4245=ORIENTED_EDGE('',*,*,#6776,.T.);
#4246=ORIENTED_EDGE('',*,*,#6777,.F.);
#4247=ORIENTED_EDGE('',*,*,#6778,.T.);
#4248=ORIENTED_EDGE('',*,*,#6773,.T.);
#4249=ORIENTED_EDGE('',*,*,#6778,.F.);
#4250=ORIENTED_EDGE('',*,*,#6772,.F.);
#4251=ORIENTED_EDGE('',*,*,#6777,.T.);
#4252=ORIENTED_EDGE('',*,*,#6763,.F.);
#4253=ORIENTED_EDGE('',*,*,#6770,.T.);
#4254=ORIENTED_EDGE('',*,*,#6774,.F.);
#4255=ORIENTED_EDGE('',*,*,#6765,.F.);
#4256=ORIENTED_EDGE('',*,*,#6752,.F.);
#4257=ORIENTED_EDGE('',*,*,#6759,.T.);
#4258=ORIENTED_EDGE('',*,*,#6775,.F.);
#4259=ORIENTED_EDGE('',*,*,#6754,.F.);
#4260=ORIENTED_EDGE('',*,*,#6741,.F.);
#4261=ORIENTED_EDGE('',*,*,#6748,.T.);
#4262=ORIENTED_EDGE('',*,*,#6776,.F.);
#4263=ORIENTED_EDGE('',*,*,#6743,.F.);
#4264=ORIENTED_EDGE('',*,*,#6779,.T.);
#4265=ORIENTED_EDGE('',*,*,#6780,.T.);
#4266=ORIENTED_EDGE('',*,*,#6781,.T.);
#4267=ORIENTED_EDGE('',*,*,#6782,.F.);
#4268=ORIENTED_EDGE('',*,*,#6783,.T.);
#4269=ORIENTED_EDGE('',*,*,#6784,.T.);
#4270=ORIENTED_EDGE('',*,*,#6785,.T.);
#4271=ORIENTED_EDGE('',*,*,#6786,.F.);
#4272=ORIENTED_EDGE('',*,*,#6787,.T.);
#4273=ORIENTED_EDGE('',*,*,#6788,.T.);
#4274=ORIENTED_EDGE('',*,*,#6789,.T.);
#4275=ORIENTED_EDGE('',*,*,#6790,.F.);
#4276=ORIENTED_EDGE('',*,*,#6791,.T.);
#4277=ORIENTED_EDGE('',*,*,#6792,.T.);
#4278=ORIENTED_EDGE('',*,*,#6793,.T.);
#4279=ORIENTED_EDGE('',*,*,#6794,.F.);
#4280=ORIENTED_EDGE('',*,*,#6795,.F.);
#4281=ORIENTED_EDGE('',*,*,#6796,.F.);
#4282=ORIENTED_EDGE('',*,*,#6797,.F.);
#4283=ORIENTED_EDGE('',*,*,#6798,.F.);
#4284=ORIENTED_EDGE('',*,*,#6799,.F.);
#4285=ORIENTED_EDGE('',*,*,#6800,.F.);
#4286=ORIENTED_EDGE('',*,*,#6797,.T.);
#4287=ORIENTED_EDGE('',*,*,#6801,.T.);
#4288=ORIENTED_EDGE('',*,*,#6802,.F.);
#4289=ORIENTED_EDGE('',*,*,#6803,.F.);
#4290=ORIENTED_EDGE('',*,*,#6795,.T.);
#4291=ORIENTED_EDGE('',*,*,#6804,.T.);
#4292=ORIENTED_EDGE('',*,*,#6805,.F.);
#4293=ORIENTED_EDGE('',*,*,#6806,.F.);
#4294=ORIENTED_EDGE('',*,*,#6807,.F.);
#4295=ORIENTED_EDGE('',*,*,#6808,.F.);
#4296=ORIENTED_EDGE('',*,*,#6809,.F.);
#4297=ORIENTED_EDGE('',*,*,#6810,.F.);
#4298=ORIENTED_EDGE('',*,*,#6808,.T.);
#4299=ORIENTED_EDGE('',*,*,#6811,.T.);
#4300=ORIENTED_EDGE('',*,*,#6812,.F.);
#4301=ORIENTED_EDGE('',*,*,#6813,.F.);
#4302=ORIENTED_EDGE('',*,*,#6806,.T.);
#4303=ORIENTED_EDGE('',*,*,#6814,.T.);
#4304=ORIENTED_EDGE('',*,*,#6783,.F.);
#4305=ORIENTED_EDGE('',*,*,#6815,.F.);
#4306=ORIENTED_EDGE('',*,*,#6779,.F.);
#4307=ORIENTED_EDGE('',*,*,#6816,.T.);
#4308=ORIENTED_EDGE('',*,*,#6791,.F.);
#4309=ORIENTED_EDGE('',*,*,#6817,.F.);
#4310=ORIENTED_EDGE('',*,*,#6787,.F.);
#4311=ORIENTED_EDGE('',*,*,#6818,.T.);
#4312=ORIENTED_EDGE('',*,*,#6819,.F.);
#4313=ORIENTED_EDGE('',*,*,#6820,.F.);
#4314=ORIENTED_EDGE('',*,*,#6781,.F.);
#4315=ORIENTED_EDGE('',*,*,#6821,.T.);
#4316=ORIENTED_EDGE('',*,*,#6793,.F.);
#4317=ORIENTED_EDGE('',*,*,#6812,.T.);
#4318=ORIENTED_EDGE('',*,*,#6822,.T.);
#4319=ORIENTED_EDGE('',*,*,#6809,.T.);
#4320=ORIENTED_EDGE('',*,*,#6823,.T.);
#4321=ORIENTED_EDGE('',*,*,#6824,.T.);
#4322=ORIENTED_EDGE('',*,*,#6784,.F.);
#4323=ORIENTED_EDGE('',*,*,#6818,.F.);
#4324=ORIENTED_EDGE('',*,*,#6790,.T.);
#4325=ORIENTED_EDGE('',*,*,#6789,.F.);
#4326=ORIENTED_EDGE('',*,*,#6825,.T.);
#4327=ORIENTED_EDGE('',*,*,#6785,.F.);
#4328=ORIENTED_EDGE('',*,*,#6824,.F.);
#4329=ORIENTED_EDGE('',*,*,#6826,.T.);
#4330=ORIENTED_EDGE('',*,*,#6802,.T.);
#4331=ORIENTED_EDGE('',*,*,#6827,.T.);
#4332=ORIENTED_EDGE('',*,*,#6799,.T.);
#4333=ORIENTED_EDGE('',*,*,#6825,.F.);
#4334=ORIENTED_EDGE('',*,*,#6788,.F.);
#4335=ORIENTED_EDGE('',*,*,#6817,.T.);
#4336=ORIENTED_EDGE('',*,*,#6794,.T.);
#4337=ORIENTED_EDGE('',*,*,#6821,.F.);
#4338=ORIENTED_EDGE('',*,*,#6780,.F.);
#4339=ORIENTED_EDGE('',*,*,#6815,.T.);
#4340=ORIENTED_EDGE('',*,*,#6786,.T.);
#4341=ORIENTED_EDGE('',*,*,#6819,.T.);
#4342=ORIENTED_EDGE('',*,*,#6816,.F.);
#4343=ORIENTED_EDGE('',*,*,#6782,.T.);
#4344=ORIENTED_EDGE('',*,*,#6820,.T.);
#4345=ORIENTED_EDGE('',*,*,#6792,.F.);
#4346=ORIENTED_EDGE('',*,*,#6805,.T.);
#4347=ORIENTED_EDGE('',*,*,#6810,.T.);
#4348=ORIENTED_EDGE('',*,*,#6822,.F.);
#4349=ORIENTED_EDGE('',*,*,#6814,.F.);
#4350=ORIENTED_EDGE('',*,*,#6807,.T.);
#4351=ORIENTED_EDGE('',*,*,#6813,.T.);
#4352=ORIENTED_EDGE('',*,*,#6823,.F.);
#4353=ORIENTED_EDGE('',*,*,#6811,.F.);
#4354=ORIENTED_EDGE('',*,*,#6796,.T.);
#4355=ORIENTED_EDGE('',*,*,#6803,.T.);
#4356=ORIENTED_EDGE('',*,*,#6826,.F.);
#4357=ORIENTED_EDGE('',*,*,#6801,.F.);
#4358=ORIENTED_EDGE('',*,*,#6798,.T.);
#4359=ORIENTED_EDGE('',*,*,#6800,.T.);
#4360=ORIENTED_EDGE('',*,*,#6827,.F.);
#4361=ORIENTED_EDGE('',*,*,#6804,.F.);
#4362=ORIENTED_EDGE('',*,*,#6828,.F.);
#4363=ORIENTED_EDGE('',*,*,#6829,.T.);
#4364=ORIENTED_EDGE('',*,*,#6830,.F.);
#4365=ORIENTED_EDGE('',*,*,#6831,.F.);
#4366=ORIENTED_EDGE('',*,*,#6832,.F.);
#4367=ORIENTED_EDGE('',*,*,#6833,.F.);
#4368=ORIENTED_EDGE('',*,*,#6834,.T.);
#4369=ORIENTED_EDGE('',*,*,#6835,.F.);
#4370=ORIENTED_EDGE('',*,*,#6836,.T.);
#4371=ORIENTED_EDGE('',*,*,#6837,.F.);
#4372=ORIENTED_EDGE('',*,*,#6838,.F.);
#4373=ORIENTED_EDGE('',*,*,#6839,.T.);
#4374=ORIENTED_EDGE('',*,*,#6840,.F.);
#4375=ORIENTED_EDGE('',*,*,#6832,.T.);
#4376=ORIENTED_EDGE('',*,*,#6841,.T.);
#4377=ORIENTED_EDGE('',*,*,#6842,.F.);
#4378=ORIENTED_EDGE('',*,*,#6843,.F.);
#4379=ORIENTED_EDGE('',*,*,#6839,.F.);
#4380=ORIENTED_EDGE('',*,*,#6844,.F.);
#4381=ORIENTED_EDGE('',*,*,#6845,.F.);
#4382=ORIENTED_EDGE('',*,*,#6846,.T.);
#4383=ORIENTED_EDGE('',*,*,#6847,.F.);
#4384=ORIENTED_EDGE('',*,*,#6830,.T.);
#4385=ORIENTED_EDGE('',*,*,#6848,.T.);
#4386=ORIENTED_EDGE('',*,*,#6842,.T.);
#4387=ORIENTED_EDGE('',*,*,#6849,.T.);
#4388=ORIENTED_EDGE('',*,*,#6850,.T.);
#4389=ORIENTED_EDGE('',*,*,#6851,.F.);
#4390=ORIENTED_EDGE('',*,*,#6852,.T.);
#4391=ORIENTED_EDGE('',*,*,#6853,.F.);
#4392=ORIENTED_EDGE('',*,*,#6854,.T.);
#4393=ORIENTED_EDGE('',*,*,#6855,.F.);
#4394=ORIENTED_EDGE('',*,*,#6856,.F.);
#4395=ORIENTED_EDGE('',*,*,#6857,.T.);
#4396=ORIENTED_EDGE('',*,*,#6858,.F.);
#4397=ORIENTED_EDGE('',*,*,#6859,.T.);
#4398=ORIENTED_EDGE('',*,*,#6860,.T.);
#4399=ORIENTED_EDGE('',*,*,#6861,.F.);
#4400=ORIENTED_EDGE('',*,*,#6862,.F.);
#4401=ORIENTED_EDGE('',*,*,#6857,.F.);
#4402=ORIENTED_EDGE('',*,*,#6863,.F.);
#4403=ORIENTED_EDGE('',*,*,#6864,.F.);
#4404=ORIENTED_EDGE('',*,*,#6865,.T.);
#4405=ORIENTED_EDGE('',*,*,#6866,.F.);
#4406=ORIENTED_EDGE('',*,*,#6867,.T.);
#4407=ORIENTED_EDGE('',*,*,#6868,.T.);
#4408=ORIENTED_EDGE('',*,*,#6861,.T.);
#4409=ORIENTED_EDGE('',*,*,#6869,.T.);
#4410=ORIENTED_EDGE('',*,*,#6870,.T.);
#4411=ORIENTED_EDGE('',*,*,#6871,.F.);
#4412=ORIENTED_EDGE('',*,*,#6867,.F.);
#4413=ORIENTED_EDGE('',*,*,#6872,.F.);
#4414=ORIENTED_EDGE('',*,*,#6859,.F.);
#4415=ORIENTED_EDGE('',*,*,#6873,.F.);
#4416=ORIENTED_EDGE('',*,*,#6874,.T.);
#4417=ORIENTED_EDGE('',*,*,#6875,.F.);
#4418=ORIENTED_EDGE('',*,*,#6876,.T.);
#4419=ORIENTED_EDGE('',*,*,#6877,.F.);
#4420=ORIENTED_EDGE('',*,*,#6878,.F.);
#4421=ORIENTED_EDGE('',*,*,#6879,.T.);
#4422=ORIENTED_EDGE('',*,*,#6880,.F.);
#4423=ORIENTED_EDGE('',*,*,#6881,.T.);
#4424=ORIENTED_EDGE('',*,*,#6882,.T.);
#4425=ORIENTED_EDGE('',*,*,#6883,.F.);
#4426=ORIENTED_EDGE('',*,*,#6884,.T.);
#4427=ORIENTED_EDGE('',*,*,#6885,.F.);
#4428=ORIENTED_EDGE('',*,*,#6886,.T.);
#4429=ORIENTED_EDGE('',*,*,#6887,.T.);
#4430=ORIENTED_EDGE('',*,*,#6888,.T.);
#4431=ORIENTED_EDGE('',*,*,#6889,.T.);
#4432=ORIENTED_EDGE('',*,*,#6890,.T.);
#4433=ORIENTED_EDGE('',*,*,#6891,.F.);
#4434=ORIENTED_EDGE('',*,*,#6892,.T.);
#4435=ORIENTED_EDGE('',*,*,#6893,.F.);
#4436=ORIENTED_EDGE('',*,*,#6894,.T.);
#4437=ORIENTED_EDGE('',*,*,#6895,.F.);
#4438=ORIENTED_EDGE('',*,*,#6896,.F.);
#4439=ORIENTED_EDGE('',*,*,#6897,.T.);
#4440=ORIENTED_EDGE('',*,*,#6898,.F.);
#4441=ORIENTED_EDGE('',*,*,#6899,.T.);
#4442=ORIENTED_EDGE('',*,*,#6900,.T.);
#4443=ORIENTED_EDGE('',*,*,#6901,.F.);
#4444=ORIENTED_EDGE('',*,*,#6902,.F.);
#4445=ORIENTED_EDGE('',*,*,#6897,.F.);
#4446=ORIENTED_EDGE('',*,*,#6903,.F.);
#4447=ORIENTED_EDGE('',*,*,#6904,.F.);
#4448=ORIENTED_EDGE('',*,*,#6905,.T.);
#4449=ORIENTED_EDGE('',*,*,#6906,.F.);
#4450=ORIENTED_EDGE('',*,*,#6907,.T.);
#4451=ORIENTED_EDGE('',*,*,#6908,.T.);
#4452=ORIENTED_EDGE('',*,*,#6901,.T.);
#4453=ORIENTED_EDGE('',*,*,#6909,.T.);
#4454=ORIENTED_EDGE('',*,*,#6910,.T.);
#4455=ORIENTED_EDGE('',*,*,#6911,.F.);
#4456=ORIENTED_EDGE('',*,*,#6907,.F.);
#4457=ORIENTED_EDGE('',*,*,#6912,.F.);
#4458=ORIENTED_EDGE('',*,*,#6899,.F.);
#4459=ORIENTED_EDGE('',*,*,#6913,.F.);
#4460=ORIENTED_EDGE('',*,*,#6841,.F.);
#4461=ORIENTED_EDGE('',*,*,#6831,.T.);
#4462=ORIENTED_EDGE('',*,*,#6847,.T.);
#4463=ORIENTED_EDGE('',*,*,#6914,.T.);
#4464=ORIENTED_EDGE('',*,*,#6835,.T.);
#4465=ORIENTED_EDGE('',*,*,#6914,.F.);
#4466=ORIENTED_EDGE('',*,*,#6846,.F.);
#4467=ORIENTED_EDGE('',*,*,#6915,.T.);
#4468=ORIENTED_EDGE('',*,*,#6836,.F.);
#4469=ORIENTED_EDGE('',*,*,#6915,.F.);
#4470=ORIENTED_EDGE('',*,*,#6851,.T.);
#4471=ORIENTED_EDGE('',*,*,#6916,.T.);
#4472=ORIENTED_EDGE('',*,*,#6837,.T.);
#4473=ORIENTED_EDGE('',*,*,#6916,.F.);
#4474=ORIENTED_EDGE('',*,*,#6850,.F.);
#4475=ORIENTED_EDGE('',*,*,#6917,.T.);
#4476=ORIENTED_EDGE('',*,*,#6849,.F.);
#4477=ORIENTED_EDGE('',*,*,#6844,.T.);
#4478=ORIENTED_EDGE('',*,*,#6838,.T.);
#4479=ORIENTED_EDGE('',*,*,#6917,.F.);
#4480=ORIENTED_EDGE('',*,*,#6853,.T.);
#4481=ORIENTED_EDGE('',*,*,#6918,.F.);
#4482=ORIENTED_EDGE('',*,*,#6865,.F.);
#4483=ORIENTED_EDGE('',*,*,#6919,.T.);
#4484=ORIENTED_EDGE('',*,*,#6854,.F.);
#4485=ORIENTED_EDGE('',*,*,#6919,.F.);
#4486=ORIENTED_EDGE('',*,*,#6871,.T.);
#4487=ORIENTED_EDGE('',*,*,#6920,.T.);
#4488=ORIENTED_EDGE('',*,*,#6855,.T.);
#4489=ORIENTED_EDGE('',*,*,#6920,.F.);
#4490=ORIENTED_EDGE('',*,*,#6870,.F.);
#4491=ORIENTED_EDGE('',*,*,#6921,.T.);
#4492=ORIENTED_EDGE('',*,*,#6869,.F.);
#4493=ORIENTED_EDGE('',*,*,#6863,.T.);
#4494=ORIENTED_EDGE('',*,*,#6856,.T.);
#4495=ORIENTED_EDGE('',*,*,#6921,.F.);
#4496=ORIENTED_EDGE('',*,*,#6860,.F.);
#4497=ORIENTED_EDGE('',*,*,#6872,.T.);
#4498=ORIENTED_EDGE('',*,*,#6866,.T.);
#4499=ORIENTED_EDGE('',*,*,#6918,.T.);
#4500=ORIENTED_EDGE('',*,*,#6875,.T.);
#4501=ORIENTED_EDGE('',*,*,#6922,.F.);
#4502=ORIENTED_EDGE('',*,*,#6884,.F.);
#4503=ORIENTED_EDGE('',*,*,#6923,.T.);
#4504=ORIENTED_EDGE('',*,*,#6876,.F.);
#4505=ORIENTED_EDGE('',*,*,#6923,.F.);
#4506=ORIENTED_EDGE('',*,*,#6891,.T.);
#4507=ORIENTED_EDGE('',*,*,#6924,.T.);
#4508=ORIENTED_EDGE('',*,*,#6877,.T.);
#4509=ORIENTED_EDGE('',*,*,#6924,.F.);
#4510=ORIENTED_EDGE('',*,*,#6890,.F.);
#4511=ORIENTED_EDGE('',*,*,#6925,.T.);
#4512=ORIENTED_EDGE('',*,*,#6889,.F.);
#4513=ORIENTED_EDGE('',*,*,#6926,.T.);
#4514=ORIENTED_EDGE('',*,*,#6878,.T.);
#4515=ORIENTED_EDGE('',*,*,#6925,.F.);
#4516=ORIENTED_EDGE('',*,*,#6882,.F.);
#4517=ORIENTED_EDGE('',*,*,#6927,.T.);
#4518=ORIENTED_EDGE('',*,*,#6885,.T.);
#4519=ORIENTED_EDGE('',*,*,#6922,.T.);
#4520=ORIENTED_EDGE('',*,*,#6893,.T.);
#4521=ORIENTED_EDGE('',*,*,#6928,.F.);
#4522=ORIENTED_EDGE('',*,*,#6905,.F.);
#4523=ORIENTED_EDGE('',*,*,#6929,.T.);
#4524=ORIENTED_EDGE('',*,*,#6894,.F.);
#4525=ORIENTED_EDGE('',*,*,#6929,.F.);
#4526=ORIENTED_EDGE('',*,*,#6911,.T.);
#4527=ORIENTED_EDGE('',*,*,#6930,.T.);
#4528=ORIENTED_EDGE('',*,*,#6895,.T.);
#4529=ORIENTED_EDGE('',*,*,#6930,.F.);
#4530=ORIENTED_EDGE('',*,*,#6910,.F.);
#4531=ORIENTED_EDGE('',*,*,#6931,.T.);
#4532=ORIENTED_EDGE('',*,*,#6909,.F.);
#4533=ORIENTED_EDGE('',*,*,#6903,.T.);
#4534=ORIENTED_EDGE('',*,*,#6896,.T.);
#4535=ORIENTED_EDGE('',*,*,#6931,.F.);
#4536=ORIENTED_EDGE('',*,*,#6900,.F.);
#4537=ORIENTED_EDGE('',*,*,#6912,.T.);
#4538=ORIENTED_EDGE('',*,*,#6906,.T.);
#4539=ORIENTED_EDGE('',*,*,#6928,.T.);
#4540=ORIENTED_EDGE('',*,*,#6932,.T.);
#4541=ORIENTED_EDGE('',*,*,#6933,.T.);
#4542=ORIENTED_EDGE('',*,*,#6934,.T.);
#4543=ORIENTED_EDGE('',*,*,#6935,.T.);
#4544=ORIENTED_EDGE('',*,*,#6936,.T.);
#4545=ORIENTED_EDGE('',*,*,#6937,.T.);
#4546=ORIENTED_EDGE('',*,*,#6938,.T.);
#4547=ORIENTED_EDGE('',*,*,#6939,.T.);
#4548=ORIENTED_EDGE('',*,*,#6940,.T.);
#4549=ORIENTED_EDGE('',*,*,#6941,.T.);
#4550=ORIENTED_EDGE('',*,*,#6942,.T.);
#4551=ORIENTED_EDGE('',*,*,#6943,.F.);
#4552=ORIENTED_EDGE('',*,*,#6944,.T.);
#4553=ORIENTED_EDGE('',*,*,#6945,.T.);
#4554=ORIENTED_EDGE('',*,*,#6946,.T.);
#4555=ORIENTED_EDGE('',*,*,#6947,.F.);
#4556=ORIENTED_EDGE('',*,*,#6948,.F.);
#4557=ORIENTED_EDGE('',*,*,#6949,.F.);
#4558=ORIENTED_EDGE('',*,*,#6950,.F.);
#4559=ORIENTED_EDGE('',*,*,#6951,.F.);
#4560=ORIENTED_EDGE('',*,*,#6952,.F.);
#4561=ORIENTED_EDGE('',*,*,#6953,.F.);
#4562=ORIENTED_EDGE('',*,*,#6954,.F.);
#4563=ORIENTED_EDGE('',*,*,#6955,.T.);
#4564=ORIENTED_EDGE('',*,*,#6943,.T.);
#4565=ORIENTED_EDGE('',*,*,#6956,.T.);
#4566=ORIENTED_EDGE('',*,*,#6945,.F.);
#4567=ORIENTED_EDGE('',*,*,#6956,.F.);
#4568=ORIENTED_EDGE('',*,*,#6942,.F.);
#4569=ORIENTED_EDGE('',*,*,#6957,.F.);
#4570=ORIENTED_EDGE('',*,*,#6946,.F.);
#4571=ORIENTED_EDGE('',*,*,#6955,.F.);
#4572=ORIENTED_EDGE('',*,*,#6944,.F.);
#4573=ORIENTED_EDGE('',*,*,#6958,.F.);
#4574=ORIENTED_EDGE('',*,*,#6933,.F.);
#4575=ORIENTED_EDGE('',*,*,#6959,.F.);
#4576=ORIENTED_EDGE('',*,*,#6960,.T.);
#4577=ORIENTED_EDGE('',*,*,#6961,.F.);
#4578=ORIENTED_EDGE('',*,*,#6962,.F.);
#4579=ORIENTED_EDGE('',*,*,#6963,.F.);
#4580=ORIENTED_EDGE('',*,*,#6964,.T.);
#4581=ORIENTED_EDGE('',*,*,#6965,.F.);
#4582=ORIENTED_EDGE('',*,*,#6966,.F.);
#4583=ORIENTED_EDGE('',*,*,#6967,.F.);
#4584=ORIENTED_EDGE('',*,*,#6968,.F.);
#4585=ORIENTED_EDGE('',*,*,#6969,.F.);
#4586=ORIENTED_EDGE('',*,*,#6970,.F.);
#4587=ORIENTED_EDGE('',*,*,#6971,.F.);
#4588=ORIENTED_EDGE('',*,*,#6972,.T.);
#4589=ORIENTED_EDGE('',*,*,#6973,.T.);
#4590=ORIENTED_EDGE('',*,*,#6974,.F.);
#4591=ORIENTED_EDGE('',*,*,#6964,.F.);
#4592=ORIENTED_EDGE('',*,*,#6975,.F.);
#4593=ORIENTED_EDGE('',*,*,#6976,.F.);
#4594=ORIENTED_EDGE('',*,*,#6977,.F.);
#4595=ORIENTED_EDGE('',*,*,#6978,.F.);
#4596=ORIENTED_EDGE('',*,*,#6979,.F.);
#4597=ORIENTED_EDGE('',*,*,#6972,.F.);
#4598=ORIENTED_EDGE('',*,*,#6980,.F.);
#4599=ORIENTED_EDGE('',*,*,#6981,.T.);
#4600=ORIENTED_EDGE('',*,*,#6982,.T.);
#4601=ORIENTED_EDGE('',*,*,#6983,.F.);
#4602=ORIENTED_EDGE('',*,*,#6984,.T.);
#4603=ORIENTED_EDGE('',*,*,#6985,.F.);
#4604=ORIENTED_EDGE('',*,*,#6986,.F.);
#4605=ORIENTED_EDGE('',*,*,#6987,.F.);
#4606=ORIENTED_EDGE('',*,*,#6988,.F.);
#4607=ORIENTED_EDGE('',*,*,#6989,.F.);
#4608=ORIENTED_EDGE('',*,*,#6990,.F.);
#4609=ORIENTED_EDGE('',*,*,#6991,.F.);
#4610=ORIENTED_EDGE('',*,*,#6973,.F.);
#4611=ORIENTED_EDGE('',*,*,#6992,.F.);
#4612=ORIENTED_EDGE('',*,*,#6993,.F.);
#4613=ORIENTED_EDGE('',*,*,#6994,.F.);
#4614=ORIENTED_EDGE('',*,*,#6995,.T.);
#4615=ORIENTED_EDGE('',*,*,#6981,.F.);
#4616=ORIENTED_EDGE('',*,*,#6995,.F.);
#4617=ORIENTED_EDGE('',*,*,#6996,.F.);
#4618=ORIENTED_EDGE('',*,*,#6984,.F.);
#4619=ORIENTED_EDGE('',*,*,#6997,.F.);
#4620=ORIENTED_EDGE('',*,*,#6982,.F.);
#4621=ORIENTED_EDGE('',*,*,#6998,.F.);
#4622=ORIENTED_EDGE('',*,*,#6976,.T.);
#4623=ORIENTED_EDGE('',*,*,#6999,.T.);
#4624=ORIENTED_EDGE('',*,*,#6978,.T.);
#4625=ORIENTED_EDGE('',*,*,#7000,.F.);
#4626=ORIENTED_EDGE('',*,*,#7001,.T.);
#4627=ORIENTED_EDGE('',*,*,#7002,.T.);
#4628=ORIENTED_EDGE('',*,*,#7003,.F.);
#4629=ORIENTED_EDGE('',*,*,#7004,.T.);
#4630=ORIENTED_EDGE('',*,*,#7005,.T.);
#4631=ORIENTED_EDGE('',*,*,#7006,.T.);
#4632=ORIENTED_EDGE('',*,*,#7007,.T.);
#4633=ORIENTED_EDGE('',*,*,#7008,.T.);
#4634=ORIENTED_EDGE('',*,*,#7009,.T.);
#4635=ORIENTED_EDGE('',*,*,#7006,.F.);
#4636=ORIENTED_EDGE('',*,*,#7010,.F.);
#4637=ORIENTED_EDGE('',*,*,#6941,.F.);
#4638=ORIENTED_EDGE('',*,*,#6940,.F.);
#4639=ORIENTED_EDGE('',*,*,#6939,.F.);
#4640=ORIENTED_EDGE('',*,*,#6938,.F.);
#4641=ORIENTED_EDGE('',*,*,#6937,.F.);
#4642=ORIENTED_EDGE('',*,*,#6936,.F.);
#4643=ORIENTED_EDGE('',*,*,#6935,.F.);
#4644=ORIENTED_EDGE('',*,*,#6934,.F.);
#4645=ORIENTED_EDGE('',*,*,#6958,.T.);
#4646=ORIENTED_EDGE('',*,*,#6959,.T.);
#4647=ORIENTED_EDGE('',*,*,#6954,.T.);
#4648=ORIENTED_EDGE('',*,*,#6953,.T.);
#4649=ORIENTED_EDGE('',*,*,#6952,.T.);
#4650=ORIENTED_EDGE('',*,*,#6951,.T.);
#4651=ORIENTED_EDGE('',*,*,#6950,.T.);
#4652=ORIENTED_EDGE('',*,*,#6949,.T.);
#4653=ORIENTED_EDGE('',*,*,#6948,.T.);
#4654=ORIENTED_EDGE('',*,*,#6947,.T.);
#4655=ORIENTED_EDGE('',*,*,#6957,.T.);
#4656=ORIENTED_EDGE('',*,*,#7007,.F.);
#4657=ORIENTED_EDGE('',*,*,#7010,.T.);
#4658=ORIENTED_EDGE('',*,*,#6967,.T.);
#4659=ORIENTED_EDGE('',*,*,#6966,.T.);
#4660=ORIENTED_EDGE('',*,*,#6965,.T.);
#4661=ORIENTED_EDGE('',*,*,#6974,.T.);
#4662=ORIENTED_EDGE('',*,*,#6991,.T.);
#4663=ORIENTED_EDGE('',*,*,#6990,.T.);
#4664=ORIENTED_EDGE('',*,*,#6989,.T.);
#4665=ORIENTED_EDGE('',*,*,#6988,.T.);
#4666=ORIENTED_EDGE('',*,*,#6987,.T.);
#4667=ORIENTED_EDGE('',*,*,#6986,.T.);
#4668=ORIENTED_EDGE('',*,*,#6985,.T.);
#4669=ORIENTED_EDGE('',*,*,#7011,.T.);
#4670=ORIENTED_EDGE('',*,*,#6980,.T.);
#4671=ORIENTED_EDGE('',*,*,#6971,.T.);
#4672=ORIENTED_EDGE('',*,*,#6970,.T.);
#4673=ORIENTED_EDGE('',*,*,#6969,.T.);
#4674=ORIENTED_EDGE('',*,*,#6968,.T.);
#4675=ORIENTED_EDGE('',*,*,#7012,.T.);
#4676=ORIENTED_EDGE('',*,*,#7013,.T.);
#4677=ORIENTED_EDGE('',*,*,#7014,.T.);
#4678=ORIENTED_EDGE('',*,*,#7015,.T.);
#4679=ORIENTED_EDGE('',*,*,#7016,.T.);
#4680=ORIENTED_EDGE('',*,*,#7017,.T.);
#4681=ORIENTED_EDGE('',*,*,#7018,.T.);
#4682=ORIENTED_EDGE('',*,*,#7000,.T.);
#4683=ORIENTED_EDGE('',*,*,#7017,.F.);
#4684=ORIENTED_EDGE('',*,*,#6998,.T.);
#4685=ORIENTED_EDGE('',*,*,#6975,.T.);
#4686=ORIENTED_EDGE('',*,*,#6963,.T.);
#4687=ORIENTED_EDGE('',*,*,#6962,.T.);
#4688=ORIENTED_EDGE('',*,*,#6961,.T.);
#4689=ORIENTED_EDGE('',*,*,#6979,.T.);
#4690=ORIENTED_EDGE('',*,*,#6999,.F.);
#4691=ORIENTED_EDGE('',*,*,#6983,.T.);
#4692=ORIENTED_EDGE('',*,*,#6997,.T.);
#4693=ORIENTED_EDGE('',*,*,#6993,.T.);
#4694=ORIENTED_EDGE('',*,*,#6992,.T.);
#4695=ORIENTED_EDGE('',*,*,#6977,.T.);
#4696=ORIENTED_EDGE('',*,*,#7008,.F.);
#4697=ORIENTED_EDGE('',*,*,#7011,.F.);
#4698=ORIENTED_EDGE('',*,*,#6996,.T.);
#4699=ORIENTED_EDGE('',*,*,#6994,.T.);
#4700=ORIENTED_EDGE('',*,*,#7001,.F.);
#4701=ORIENTED_EDGE('',*,*,#7012,.F.);
#4702=ORIENTED_EDGE('',*,*,#7013,.F.);
#4703=ORIENTED_EDGE('',*,*,#7019,.T.);
#4704=ORIENTED_EDGE('',*,*,#7014,.F.);
#4705=ORIENTED_EDGE('',*,*,#7002,.F.);
#4706=ORIENTED_EDGE('',*,*,#7020,.T.);
#4707=ORIENTED_EDGE('',*,*,#7003,.T.);
#4708=ORIENTED_EDGE('',*,*,#7021,.T.);
#4709=ORIENTED_EDGE('',*,*,#6960,.F.);
#4710=ORIENTED_EDGE('',*,*,#7021,.F.);
#4711=ORIENTED_EDGE('',*,*,#7016,.F.);
#4712=ORIENTED_EDGE('',*,*,#7019,.F.);
#4713=ORIENTED_EDGE('',*,*,#7015,.F.);
#4714=ORIENTED_EDGE('',*,*,#7005,.F.);
#4715=ORIENTED_EDGE('',*,*,#7018,.F.);
#4716=ORIENTED_EDGE('',*,*,#7004,.F.);
#4717=ORIENTED_EDGE('',*,*,#7020,.F.);
#4718=ORIENTED_EDGE('',*,*,#6932,.F.);
#4719=ORIENTED_EDGE('',*,*,#7022,.T.);
#4720=ORIENTED_EDGE('',*,*,#6892,.F.);
#4721=ORIENTED_EDGE('',*,*,#6904,.T.);
#4722=ORIENTED_EDGE('',*,*,#6874,.F.);
#4723=ORIENTED_EDGE('',*,*,#6883,.T.);
#4724=ORIENTED_EDGE('',*,*,#6852,.F.);
#4725=ORIENTED_EDGE('',*,*,#6864,.T.);
#4726=ORIENTED_EDGE('',*,*,#6834,.F.);
#4727=ORIENTED_EDGE('',*,*,#6845,.T.);
#4728=ORIENTED_EDGE('',*,*,#7022,.F.);
#4729=ORIENTED_EDGE('',*,*,#6829,.F.);
#4730=ORIENTED_EDGE('',*,*,#6881,.F.);
#4731=ORIENTED_EDGE('',*,*,#7023,.F.);
#4732=ORIENTED_EDGE('',*,*,#6886,.F.);
#4733=ORIENTED_EDGE('',*,*,#6927,.F.);
#4734=ORIENTED_EDGE('',*,*,#6879,.F.);
#4735=ORIENTED_EDGE('',*,*,#6926,.F.);
#4736=ORIENTED_EDGE('',*,*,#6888,.F.);
#4737=ORIENTED_EDGE('',*,*,#7024,.F.);
#4738=ORIENTED_EDGE('',*,*,#6880,.T.);
#4739=ORIENTED_EDGE('',*,*,#7024,.T.);
#4740=ORIENTED_EDGE('',*,*,#6887,.F.);
#4741=ORIENTED_EDGE('',*,*,#7023,.T.);
#4742=ORIENTED_EDGE('',*,*,#7009,.F.);
#4743=ORIENTED_EDGE('',*,*,#6828,.T.);
#4744=ORIENTED_EDGE('',*,*,#6848,.F.);
#4745=ORIENTED_EDGE('',*,*,#6833,.T.);
#4746=ORIENTED_EDGE('',*,*,#6840,.T.);
#4747=ORIENTED_EDGE('',*,*,#6843,.T.);
#4748=ORIENTED_EDGE('',*,*,#6898,.T.);
#4749=ORIENTED_EDGE('',*,*,#6902,.T.);
#4750=ORIENTED_EDGE('',*,*,#6908,.F.);
#4751=ORIENTED_EDGE('',*,*,#6913,.T.);
#4752=ORIENTED_EDGE('',*,*,#6858,.T.);
#4753=ORIENTED_EDGE('',*,*,#6862,.T.);
#4754=ORIENTED_EDGE('',*,*,#6868,.F.);
#4755=ORIENTED_EDGE('',*,*,#6873,.T.);
#4756=ORIENTED_EDGE('',*,*,#7025,.T.);
#4757=ORIENTED_EDGE('',*,*,#7026,.T.);
#4758=ORIENTED_EDGE('',*,*,#7027,.T.);
#4759=ORIENTED_EDGE('',*,*,#7028,.T.);
#4760=ORIENTED_EDGE('',*,*,#7029,.F.);
#4761=ORIENTED_EDGE('',*,*,#7030,.F.);
#4762=ORIENTED_EDGE('',*,*,#7028,.F.);
#4763=ORIENTED_EDGE('',*,*,#7031,.T.);
#4764=ORIENTED_EDGE('',*,*,#7032,.F.);
#4765=ORIENTED_EDGE('',*,*,#7033,.F.);
#4766=ORIENTED_EDGE('',*,*,#7026,.F.);
#4767=ORIENTED_EDGE('',*,*,#7034,.T.);
#4768=ORIENTED_EDGE('',*,*,#7035,.F.);
#4769=ORIENTED_EDGE('',*,*,#7034,.F.);
#4770=ORIENTED_EDGE('',*,*,#7025,.F.);
#4771=ORIENTED_EDGE('',*,*,#7030,.T.);
#4772=ORIENTED_EDGE('',*,*,#7036,.T.);
#4773=ORIENTED_EDGE('',*,*,#7037,.T.);
#4774=ORIENTED_EDGE('',*,*,#7038,.T.);
#4775=ORIENTED_EDGE('',*,*,#7039,.T.);
#4776=ORIENTED_EDGE('',*,*,#7040,.F.);
#4777=ORIENTED_EDGE('',*,*,#7041,.F.);
#4778=ORIENTED_EDGE('',*,*,#7039,.F.);
#4779=ORIENTED_EDGE('',*,*,#7042,.T.);
#4780=ORIENTED_EDGE('',*,*,#7043,.F.);
#4781=ORIENTED_EDGE('',*,*,#7044,.F.);
#4782=ORIENTED_EDGE('',*,*,#7037,.F.);
#4783=ORIENTED_EDGE('',*,*,#7045,.T.);
#4784=ORIENTED_EDGE('',*,*,#7046,.F.);
#4785=ORIENTED_EDGE('',*,*,#7045,.F.);
#4786=ORIENTED_EDGE('',*,*,#7036,.F.);
#4787=ORIENTED_EDGE('',*,*,#7041,.T.);
#4788=ORIENTED_EDGE('',*,*,#7047,.T.);
#4789=ORIENTED_EDGE('',*,*,#7048,.T.);
#4790=ORIENTED_EDGE('',*,*,#7049,.T.);
#4791=ORIENTED_EDGE('',*,*,#7050,.T.);
#4792=ORIENTED_EDGE('',*,*,#7051,.F.);
#4793=ORIENTED_EDGE('',*,*,#7052,.F.);
#4794=ORIENTED_EDGE('',*,*,#7050,.F.);
#4795=ORIENTED_EDGE('',*,*,#7053,.T.);
#4796=ORIENTED_EDGE('',*,*,#7054,.F.);
#4797=ORIENTED_EDGE('',*,*,#7055,.F.);
#4798=ORIENTED_EDGE('',*,*,#7048,.F.);
#4799=ORIENTED_EDGE('',*,*,#7056,.T.);
#4800=ORIENTED_EDGE('',*,*,#7057,.F.);
#4801=ORIENTED_EDGE('',*,*,#7056,.F.);
#4802=ORIENTED_EDGE('',*,*,#7047,.F.);
#4803=ORIENTED_EDGE('',*,*,#7052,.T.);
#4804=ORIENTED_EDGE('',*,*,#7058,.F.);
#4805=ORIENTED_EDGE('',*,*,#7059,.F.);
#4806=ORIENTED_EDGE('',*,*,#7060,.F.);
#4807=ORIENTED_EDGE('',*,*,#7061,.F.);
#4808=ORIENTED_EDGE('',*,*,#7062,.F.);
#4809=ORIENTED_EDGE('',*,*,#7054,.T.);
#4810=ORIENTED_EDGE('',*,*,#7057,.T.);
#4811=ORIENTED_EDGE('',*,*,#7051,.T.);
#4812=ORIENTED_EDGE('',*,*,#7063,.T.);
#4813=ORIENTED_EDGE('',*,*,#7043,.T.);
#4814=ORIENTED_EDGE('',*,*,#7046,.T.);
#4815=ORIENTED_EDGE('',*,*,#7040,.T.);
#4816=ORIENTED_EDGE('',*,*,#7064,.T.);
#4817=ORIENTED_EDGE('',*,*,#7032,.T.);
#4818=ORIENTED_EDGE('',*,*,#7035,.T.);
#4819=ORIENTED_EDGE('',*,*,#7029,.T.);
#4820=ORIENTED_EDGE('',*,*,#7065,.T.);
#4821=ORIENTED_EDGE('',*,*,#7066,.T.);
#4822=ORIENTED_EDGE('',*,*,#7067,.T.);
#4823=ORIENTED_EDGE('',*,*,#7068,.T.);
#4824=ORIENTED_EDGE('',*,*,#7069,.T.);
#4825=ORIENTED_EDGE('',*,*,#7070,.T.);
#4826=ORIENTED_EDGE('',*,*,#7071,.T.);
#4827=ORIENTED_EDGE('',*,*,#7072,.F.);
#4828=ORIENTED_EDGE('',*,*,#7059,.T.);
#4829=ORIENTED_EDGE('',*,*,#7068,.F.);
#4830=ORIENTED_EDGE('',*,*,#7060,.T.);
#4831=ORIENTED_EDGE('',*,*,#7069,.F.);
#4832=ORIENTED_EDGE('',*,*,#7061,.T.);
#4833=ORIENTED_EDGE('',*,*,#7070,.F.);
#4834=ORIENTED_EDGE('',*,*,#7062,.T.);
#4835=ORIENTED_EDGE('',*,*,#7071,.F.);
#4836=ORIENTED_EDGE('',*,*,#7058,.T.);
#4837=ORIENTED_EDGE('',*,*,#7067,.F.);
#4838=ORIENTED_EDGE('',*,*,#7049,.F.);
#4839=ORIENTED_EDGE('',*,*,#7055,.T.);
#4840=ORIENTED_EDGE('',*,*,#7063,.F.);
#4841=ORIENTED_EDGE('',*,*,#7053,.F.);
#4842=ORIENTED_EDGE('',*,*,#7038,.F.);
#4843=ORIENTED_EDGE('',*,*,#7044,.T.);
#4844=ORIENTED_EDGE('',*,*,#7064,.F.);
#4845=ORIENTED_EDGE('',*,*,#7042,.F.);
#4846=ORIENTED_EDGE('',*,*,#7027,.F.);
#4847=ORIENTED_EDGE('',*,*,#7033,.T.);
#4848=ORIENTED_EDGE('',*,*,#7065,.F.);
#4849=ORIENTED_EDGE('',*,*,#7031,.F.);
#4850=ORIENTED_EDGE('',*,*,#7072,.T.);
#4851=ORIENTED_EDGE('',*,*,#7066,.F.);
#4852=ORIENTED_EDGE('',*,*,#7073,.F.);
#4853=ORIENTED_EDGE('',*,*,#7074,.T.);
#4854=ORIENTED_EDGE('',*,*,#7075,.F.);
#4855=ORIENTED_EDGE('',*,*,#7076,.F.);
#4856=ORIENTED_EDGE('',*,*,#7077,.F.);
#4857=ORIENTED_EDGE('',*,*,#7078,.F.);
#4858=ORIENTED_EDGE('',*,*,#7079,.F.);
#4859=ORIENTED_EDGE('',*,*,#7080,.F.);
#4860=ORIENTED_EDGE('',*,*,#7081,.F.);
#4861=ORIENTED_EDGE('',*,*,#7082,.F.);
#4862=ORIENTED_EDGE('',*,*,#7083,.F.);
#4863=ORIENTED_EDGE('',*,*,#7084,.F.);
#4864=ORIENTED_EDGE('',*,*,#7085,.F.);
#4865=ORIENTED_EDGE('',*,*,#7086,.T.);
#4866=ORIENTED_EDGE('',*,*,#7087,.T.);
#4867=ORIENTED_EDGE('',*,*,#7088,.T.);
#4868=ORIENTED_EDGE('',*,*,#7089,.T.);
#4869=ORIENTED_EDGE('',*,*,#7090,.T.);
#4870=ORIENTED_EDGE('',*,*,#7091,.T.);
#4871=ORIENTED_EDGE('',*,*,#7092,.T.);
#4872=ORIENTED_EDGE('',*,*,#7093,.T.);
#4873=ORIENTED_EDGE('',*,*,#7094,.T.);
#4874=ORIENTED_EDGE('',*,*,#7095,.F.);
#4875=ORIENTED_EDGE('',*,*,#7096,.F.);
#4876=ORIENTED_EDGE('',*,*,#7097,.F.);
#4877=ORIENTED_EDGE('',*,*,#7096,.T.);
#4878=ORIENTED_EDGE('',*,*,#7098,.F.);
#4879=ORIENTED_EDGE('',*,*,#7074,.F.);
#4880=ORIENTED_EDGE('',*,*,#7098,.T.);
#4881=ORIENTED_EDGE('',*,*,#7095,.T.);
#4882=ORIENTED_EDGE('',*,*,#7099,.T.);
#4883=ORIENTED_EDGE('',*,*,#7075,.T.);
#4884=ORIENTED_EDGE('',*,*,#7097,.T.);
#4885=ORIENTED_EDGE('',*,*,#7073,.T.);
#4886=ORIENTED_EDGE('',*,*,#7100,.T.);
#4887=ORIENTED_EDGE('',*,*,#7085,.T.);
#4888=ORIENTED_EDGE('',*,*,#7101,.T.);
#4889=ORIENTED_EDGE('',*,*,#7102,.T.);
#4890=ORIENTED_EDGE('',*,*,#7103,.F.);
#4891=ORIENTED_EDGE('',*,*,#7104,.T.);
#4892=ORIENTED_EDGE('',*,*,#7105,.T.);
#4893=ORIENTED_EDGE('',*,*,#7103,.T.);
#4894=ORIENTED_EDGE('',*,*,#7106,.T.);
#4895=ORIENTED_EDGE('',*,*,#7107,.F.);
#4896=ORIENTED_EDGE('',*,*,#7108,.T.);
#4897=ORIENTED_EDGE('',*,*,#7109,.T.);
#4898=ORIENTED_EDGE('',*,*,#7107,.T.);
#4899=ORIENTED_EDGE('',*,*,#7110,.T.);
#4900=ORIENTED_EDGE('',*,*,#7111,.T.);
#4901=ORIENTED_EDGE('',*,*,#7112,.T.);
#4902=ORIENTED_EDGE('',*,*,#7113,.F.);
#4903=ORIENTED_EDGE('',*,*,#7114,.T.);
#4904=ORIENTED_EDGE('',*,*,#7115,.T.);
#4905=ORIENTED_EDGE('',*,*,#7113,.T.);
#4906=ORIENTED_EDGE('',*,*,#7116,.T.);
#4907=ORIENTED_EDGE('',*,*,#7117,.F.);
#4908=ORIENTED_EDGE('',*,*,#7118,.T.);
#4909=ORIENTED_EDGE('',*,*,#7119,.T.);
#4910=ORIENTED_EDGE('',*,*,#7117,.T.);
#4911=ORIENTED_EDGE('',*,*,#7120,.T.);
#4912=ORIENTED_EDGE('',*,*,#7121,.T.);
#4913=ORIENTED_EDGE('',*,*,#7122,.T.);
#4914=ORIENTED_EDGE('',*,*,#7123,.F.);
#4915=ORIENTED_EDGE('',*,*,#7124,.T.);
#4916=ORIENTED_EDGE('',*,*,#7125,.T.);
#4917=ORIENTED_EDGE('',*,*,#7123,.T.);
#4918=ORIENTED_EDGE('',*,*,#7126,.T.);
#4919=ORIENTED_EDGE('',*,*,#7127,.F.);
#4920=ORIENTED_EDGE('',*,*,#7128,.T.);
#4921=ORIENTED_EDGE('',*,*,#7129,.T.);
#4922=ORIENTED_EDGE('',*,*,#7127,.T.);
#4923=ORIENTED_EDGE('',*,*,#7130,.T.);
#4924=ORIENTED_EDGE('',*,*,#7131,.T.);
#4925=ORIENTED_EDGE('',*,*,#7132,.T.);
#4926=ORIENTED_EDGE('',*,*,#7133,.F.);
#4927=ORIENTED_EDGE('',*,*,#7134,.T.);
#4928=ORIENTED_EDGE('',*,*,#7135,.T.);
#4929=ORIENTED_EDGE('',*,*,#7133,.T.);
#4930=ORIENTED_EDGE('',*,*,#7136,.T.);
#4931=ORIENTED_EDGE('',*,*,#7137,.F.);
#4932=ORIENTED_EDGE('',*,*,#7138,.T.);
#4933=ORIENTED_EDGE('',*,*,#7139,.T.);
#4934=ORIENTED_EDGE('',*,*,#7137,.T.);
#4935=ORIENTED_EDGE('',*,*,#7140,.T.);
#4936=ORIENTED_EDGE('',*,*,#7141,.T.);
#4937=ORIENTED_EDGE('',*,*,#7142,.T.);
#4938=ORIENTED_EDGE('',*,*,#7143,.F.);
#4939=ORIENTED_EDGE('',*,*,#7144,.T.);
#4940=ORIENTED_EDGE('',*,*,#7145,.T.);
#4941=ORIENTED_EDGE('',*,*,#7143,.T.);
#4942=ORIENTED_EDGE('',*,*,#7146,.T.);
#4943=ORIENTED_EDGE('',*,*,#7147,.F.);
#4944=ORIENTED_EDGE('',*,*,#7148,.T.);
#4945=ORIENTED_EDGE('',*,*,#7149,.T.);
#4946=ORIENTED_EDGE('',*,*,#7147,.T.);
#4947=ORIENTED_EDGE('',*,*,#7150,.T.);
#4948=ORIENTED_EDGE('',*,*,#7151,.T.);
#4949=ORIENTED_EDGE('',*,*,#7152,.T.);
#4950=ORIENTED_EDGE('',*,*,#7153,.F.);
#4951=ORIENTED_EDGE('',*,*,#7154,.T.);
#4952=ORIENTED_EDGE('',*,*,#7155,.T.);
#4953=ORIENTED_EDGE('',*,*,#7153,.T.);
#4954=ORIENTED_EDGE('',*,*,#7156,.T.);
#4955=ORIENTED_EDGE('',*,*,#7157,.F.);
#4956=ORIENTED_EDGE('',*,*,#7158,.T.);
#4957=ORIENTED_EDGE('',*,*,#7159,.T.);
#4958=ORIENTED_EDGE('',*,*,#7157,.T.);
#4959=ORIENTED_EDGE('',*,*,#7160,.T.);
#4960=ORIENTED_EDGE('',*,*,#7161,.T.);
#4961=ORIENTED_EDGE('',*,*,#7162,.T.);
#4962=ORIENTED_EDGE('',*,*,#7163,.F.);
#4963=ORIENTED_EDGE('',*,*,#7164,.T.);
#4964=ORIENTED_EDGE('',*,*,#7165,.T.);
#4965=ORIENTED_EDGE('',*,*,#7163,.T.);
#4966=ORIENTED_EDGE('',*,*,#7166,.T.);
#4967=ORIENTED_EDGE('',*,*,#7167,.F.);
#4968=ORIENTED_EDGE('',*,*,#7168,.T.);
#4969=ORIENTED_EDGE('',*,*,#7169,.T.);
#4970=ORIENTED_EDGE('',*,*,#7167,.T.);
#4971=ORIENTED_EDGE('',*,*,#7170,.T.);
#4972=ORIENTED_EDGE('',*,*,#7171,.T.);
#4973=ORIENTED_EDGE('',*,*,#7172,.T.);
#4974=ORIENTED_EDGE('',*,*,#7173,.F.);
#4975=ORIENTED_EDGE('',*,*,#7174,.T.);
#4976=ORIENTED_EDGE('',*,*,#7175,.T.);
#4977=ORIENTED_EDGE('',*,*,#7173,.T.);
#4978=ORIENTED_EDGE('',*,*,#7176,.T.);
#4979=ORIENTED_EDGE('',*,*,#7177,.F.);
#4980=ORIENTED_EDGE('',*,*,#7178,.T.);
#4981=ORIENTED_EDGE('',*,*,#7179,.T.);
#4982=ORIENTED_EDGE('',*,*,#7177,.T.);
#4983=ORIENTED_EDGE('',*,*,#7180,.T.);
#4984=ORIENTED_EDGE('',*,*,#7181,.T.);
#4985=ORIENTED_EDGE('',*,*,#7182,.T.);
#4986=ORIENTED_EDGE('',*,*,#7183,.F.);
#4987=ORIENTED_EDGE('',*,*,#7184,.T.);
#4988=ORIENTED_EDGE('',*,*,#7185,.T.);
#4989=ORIENTED_EDGE('',*,*,#7183,.T.);
#4990=ORIENTED_EDGE('',*,*,#7186,.T.);
#4991=ORIENTED_EDGE('',*,*,#7187,.F.);
#4992=ORIENTED_EDGE('',*,*,#7188,.T.);
#4993=ORIENTED_EDGE('',*,*,#7189,.T.);
#4994=ORIENTED_EDGE('',*,*,#7187,.T.);
#4995=ORIENTED_EDGE('',*,*,#7190,.T.);
#4996=ORIENTED_EDGE('',*,*,#7191,.T.);
#4997=ORIENTED_EDGE('',*,*,#7192,.T.);
#4998=ORIENTED_EDGE('',*,*,#7193,.F.);
#4999=ORIENTED_EDGE('',*,*,#7194,.T.);
#5000=ORIENTED_EDGE('',*,*,#7195,.T.);
#5001=ORIENTED_EDGE('',*,*,#7193,.T.);
#5002=ORIENTED_EDGE('',*,*,#7196,.T.);
#5003=ORIENTED_EDGE('',*,*,#7197,.F.);
#5004=ORIENTED_EDGE('',*,*,#7198,.T.);
#5005=ORIENTED_EDGE('',*,*,#7199,.T.);
#5006=ORIENTED_EDGE('',*,*,#7197,.T.);
#5007=ORIENTED_EDGE('',*,*,#7200,.T.);
#5008=ORIENTED_EDGE('',*,*,#7201,.T.);
#5009=ORIENTED_EDGE('',*,*,#7202,.T.);
#5010=ORIENTED_EDGE('',*,*,#7203,.F.);
#5011=ORIENTED_EDGE('',*,*,#7204,.T.);
#5012=ORIENTED_EDGE('',*,*,#7205,.T.);
#5013=ORIENTED_EDGE('',*,*,#7203,.T.);
#5014=ORIENTED_EDGE('',*,*,#7206,.T.);
#5015=ORIENTED_EDGE('',*,*,#7207,.F.);
#5016=ORIENTED_EDGE('',*,*,#7208,.T.);
#5017=ORIENTED_EDGE('',*,*,#7209,.T.);
#5018=ORIENTED_EDGE('',*,*,#7207,.T.);
#5019=ORIENTED_EDGE('',*,*,#7210,.T.);
#5020=ORIENTED_EDGE('',*,*,#7110,.F.);
#5021=ORIENTED_EDGE('',*,*,#7106,.F.);
#5022=ORIENTED_EDGE('',*,*,#7102,.F.);
#5023=ORIENTED_EDGE('',*,*,#7211,.T.);
#5024=ORIENTED_EDGE('',*,*,#7210,.F.);
#5025=ORIENTED_EDGE('',*,*,#7206,.F.);
#5026=ORIENTED_EDGE('',*,*,#7202,.F.);
#5027=ORIENTED_EDGE('',*,*,#7212,.T.);
#5028=ORIENTED_EDGE('',*,*,#7200,.F.);
#5029=ORIENTED_EDGE('',*,*,#7196,.F.);
#5030=ORIENTED_EDGE('',*,*,#7192,.F.);
#5031=ORIENTED_EDGE('',*,*,#7213,.T.);
#5032=ORIENTED_EDGE('',*,*,#7190,.F.);
#5033=ORIENTED_EDGE('',*,*,#7186,.F.);
#5034=ORIENTED_EDGE('',*,*,#7182,.F.);
#5035=ORIENTED_EDGE('',*,*,#7214,.T.);
#5036=ORIENTED_EDGE('',*,*,#7180,.F.);
#5037=ORIENTED_EDGE('',*,*,#7176,.F.);
#5038=ORIENTED_EDGE('',*,*,#7172,.F.);
#5039=ORIENTED_EDGE('',*,*,#7215,.T.);
#5040=ORIENTED_EDGE('',*,*,#7170,.F.);
#5041=ORIENTED_EDGE('',*,*,#7166,.F.);
#5042=ORIENTED_EDGE('',*,*,#7162,.F.);
#5043=ORIENTED_EDGE('',*,*,#7216,.T.);
#5044=ORIENTED_EDGE('',*,*,#7160,.F.);
#5045=ORIENTED_EDGE('',*,*,#7156,.F.);
#5046=ORIENTED_EDGE('',*,*,#7152,.F.);
#5047=ORIENTED_EDGE('',*,*,#7217,.T.);
#5048=ORIENTED_EDGE('',*,*,#7150,.F.);
#5049=ORIENTED_EDGE('',*,*,#7146,.F.);
#5050=ORIENTED_EDGE('',*,*,#7142,.F.);
#5051=ORIENTED_EDGE('',*,*,#7218,.T.);
#5052=ORIENTED_EDGE('',*,*,#7140,.F.);
#5053=ORIENTED_EDGE('',*,*,#7136,.F.);
#5054=ORIENTED_EDGE('',*,*,#7132,.F.);
#5055=ORIENTED_EDGE('',*,*,#7219,.T.);
#5056=ORIENTED_EDGE('',*,*,#7130,.F.);
#5057=ORIENTED_EDGE('',*,*,#7126,.F.);
#5058=ORIENTED_EDGE('',*,*,#7122,.F.);
#5059=ORIENTED_EDGE('',*,*,#7220,.T.);
#5060=ORIENTED_EDGE('',*,*,#7120,.F.);
#5061=ORIENTED_EDGE('',*,*,#7116,.F.);
#5062=ORIENTED_EDGE('',*,*,#7112,.F.);
#5063=ORIENTED_EDGE('',*,*,#7221,.T.);
#5064=ORIENTED_EDGE('',*,*,#7222,.F.);
#5065=ORIENTED_EDGE('',*,*,#7105,.F.);
#5066=ORIENTED_EDGE('',*,*,#7109,.F.);
#5067=ORIENTED_EDGE('',*,*,#7223,.F.);
#5068=ORIENTED_EDGE('',*,*,#7114,.F.);
#5069=ORIENTED_EDGE('',*,*,#7115,.F.);
#5070=ORIENTED_EDGE('',*,*,#7119,.F.);
#5071=ORIENTED_EDGE('',*,*,#7224,.F.);
#5072=ORIENTED_EDGE('',*,*,#7124,.F.);
#5073=ORIENTED_EDGE('',*,*,#7125,.F.);
#5074=ORIENTED_EDGE('',*,*,#7129,.F.);
#5075=ORIENTED_EDGE('',*,*,#7225,.F.);
#5076=ORIENTED_EDGE('',*,*,#7134,.F.);
#5077=ORIENTED_EDGE('',*,*,#7135,.F.);
#5078=ORIENTED_EDGE('',*,*,#7139,.F.);
#5079=ORIENTED_EDGE('',*,*,#7226,.F.);
#5080=ORIENTED_EDGE('',*,*,#7144,.F.);
#5081=ORIENTED_EDGE('',*,*,#7145,.F.);
#5082=ORIENTED_EDGE('',*,*,#7149,.F.);
#5083=ORIENTED_EDGE('',*,*,#7227,.F.);
#5084=ORIENTED_EDGE('',*,*,#7154,.F.);
#5085=ORIENTED_EDGE('',*,*,#7155,.F.);
#5086=ORIENTED_EDGE('',*,*,#7159,.F.);
#5087=ORIENTED_EDGE('',*,*,#7228,.F.);
#5088=ORIENTED_EDGE('',*,*,#7164,.F.);
#5089=ORIENTED_EDGE('',*,*,#7165,.F.);
#5090=ORIENTED_EDGE('',*,*,#7169,.F.);
#5091=ORIENTED_EDGE('',*,*,#7229,.F.);
#5092=ORIENTED_EDGE('',*,*,#7174,.F.);
#5093=ORIENTED_EDGE('',*,*,#7175,.F.);
#5094=ORIENTED_EDGE('',*,*,#7179,.F.);
#5095=ORIENTED_EDGE('',*,*,#7230,.F.);
#5096=ORIENTED_EDGE('',*,*,#7184,.F.);
#5097=ORIENTED_EDGE('',*,*,#7185,.F.);
#5098=ORIENTED_EDGE('',*,*,#7189,.F.);
#5099=ORIENTED_EDGE('',*,*,#7231,.F.);
#5100=ORIENTED_EDGE('',*,*,#7194,.F.);
#5101=ORIENTED_EDGE('',*,*,#7195,.F.);
#5102=ORIENTED_EDGE('',*,*,#7199,.F.);
#5103=ORIENTED_EDGE('',*,*,#7232,.F.);
#5104=ORIENTED_EDGE('',*,*,#7204,.F.);
#5105=ORIENTED_EDGE('',*,*,#7205,.F.);
#5106=ORIENTED_EDGE('',*,*,#7209,.F.);
#5107=ORIENTED_EDGE('',*,*,#7233,.F.);
#5108=ORIENTED_EDGE('',*,*,#7104,.F.);
#5109=ORIENTED_EDGE('',*,*,#7234,.T.);
#5110=ORIENTED_EDGE('',*,*,#7101,.F.);
#5111=ORIENTED_EDGE('',*,*,#7233,.T.);
#5112=ORIENTED_EDGE('',*,*,#7208,.F.);
#5113=ORIENTED_EDGE('',*,*,#7211,.F.);
#5114=ORIENTED_EDGE('',*,*,#7235,.F.);
#5115=ORIENTED_EDGE('',*,*,#7236,.T.);
#5116=ORIENTED_EDGE('',*,*,#7198,.F.);
#5117=ORIENTED_EDGE('',*,*,#7212,.F.);
#5118=ORIENTED_EDGE('',*,*,#7201,.F.);
#5119=ORIENTED_EDGE('',*,*,#7232,.T.);
#5120=ORIENTED_EDGE('',*,*,#7188,.F.);
#5121=ORIENTED_EDGE('',*,*,#7213,.F.);
#5122=ORIENTED_EDGE('',*,*,#7191,.F.);
#5123=ORIENTED_EDGE('',*,*,#7231,.T.);
#5124=ORIENTED_EDGE('',*,*,#7178,.F.);
#5125=ORIENTED_EDGE('',*,*,#7214,.F.);
#5126=ORIENTED_EDGE('',*,*,#7181,.F.);
#5127=ORIENTED_EDGE('',*,*,#7230,.T.);
#5128=ORIENTED_EDGE('',*,*,#7168,.F.);
#5129=ORIENTED_EDGE('',*,*,#7215,.F.);
#5130=ORIENTED_EDGE('',*,*,#7171,.F.);
#5131=ORIENTED_EDGE('',*,*,#7229,.T.);
#5132=ORIENTED_EDGE('',*,*,#7158,.F.);
#5133=ORIENTED_EDGE('',*,*,#7216,.F.);
#5134=ORIENTED_EDGE('',*,*,#7161,.F.);
#5135=ORIENTED_EDGE('',*,*,#7228,.T.);
#5136=ORIENTED_EDGE('',*,*,#7148,.F.);
#5137=ORIENTED_EDGE('',*,*,#7217,.F.);
#5138=ORIENTED_EDGE('',*,*,#7151,.F.);
#5139=ORIENTED_EDGE('',*,*,#7227,.T.);
#5140=ORIENTED_EDGE('',*,*,#7138,.F.);
#5141=ORIENTED_EDGE('',*,*,#7218,.F.);
#5142=ORIENTED_EDGE('',*,*,#7141,.F.);
#5143=ORIENTED_EDGE('',*,*,#7226,.T.);
#5144=ORIENTED_EDGE('',*,*,#7128,.F.);
#5145=ORIENTED_EDGE('',*,*,#7219,.F.);
#5146=ORIENTED_EDGE('',*,*,#7131,.F.);
#5147=ORIENTED_EDGE('',*,*,#7225,.T.);
#5148=ORIENTED_EDGE('',*,*,#7118,.F.);
#5149=ORIENTED_EDGE('',*,*,#7220,.F.);
#5150=ORIENTED_EDGE('',*,*,#7121,.F.);
#5151=ORIENTED_EDGE('',*,*,#7224,.T.);
#5152=ORIENTED_EDGE('',*,*,#7108,.F.);
#5153=ORIENTED_EDGE('',*,*,#7221,.F.);
#5154=ORIENTED_EDGE('',*,*,#7111,.F.);
#5155=ORIENTED_EDGE('',*,*,#7223,.T.);
#5156=ORIENTED_EDGE('',*,*,#7079,.T.);
#5157=ORIENTED_EDGE('',*,*,#7078,.T.);
#5158=ORIENTED_EDGE('',*,*,#7077,.T.);
#5159=ORIENTED_EDGE('',*,*,#7076,.T.);
#5160=ORIENTED_EDGE('',*,*,#7099,.F.);
#5161=ORIENTED_EDGE('',*,*,#7094,.F.);
#5162=ORIENTED_EDGE('',*,*,#7093,.F.);
#5163=ORIENTED_EDGE('',*,*,#7092,.F.);
#5164=ORIENTED_EDGE('',*,*,#7091,.F.);
#5165=ORIENTED_EDGE('',*,*,#7090,.F.);
#5166=ORIENTED_EDGE('',*,*,#7089,.F.);
#5167=ORIENTED_EDGE('',*,*,#7088,.F.);
#5168=ORIENTED_EDGE('',*,*,#7087,.F.);
#5169=ORIENTED_EDGE('',*,*,#7086,.F.);
#5170=ORIENTED_EDGE('',*,*,#7234,.F.);
#5171=ORIENTED_EDGE('',*,*,#7100,.F.);
#5172=ORIENTED_EDGE('',*,*,#7084,.T.);
#5173=ORIENTED_EDGE('',*,*,#7083,.T.);
#5174=ORIENTED_EDGE('',*,*,#7082,.T.);
#5175=ORIENTED_EDGE('',*,*,#7081,.T.);
#5176=ORIENTED_EDGE('',*,*,#7080,.T.);
#5177=ORIENTED_EDGE('',*,*,#7235,.T.);
#5178=ORIENTED_EDGE('',*,*,#7222,.T.);
#5179=ORIENTED_EDGE('',*,*,#7236,.F.);
#5180=ORIENTED_EDGE('',*,*,#7237,.T.);
#5181=ORIENTED_EDGE('',*,*,#7238,.T.);
#5182=ORIENTED_EDGE('',*,*,#7239,.T.);
#5183=ORIENTED_EDGE('',*,*,#7240,.T.);
#5184=ORIENTED_EDGE('',*,*,#7241,.T.);
#5185=ORIENTED_EDGE('',*,*,#7242,.F.);
#5186=ORIENTED_EDGE('',*,*,#7239,.F.);
#5187=ORIENTED_EDGE('',*,*,#7243,.T.);
#5188=ORIENTED_EDGE('',*,*,#7244,.T.);
#5189=ORIENTED_EDGE('',*,*,#7245,.F.);
#5190=ORIENTED_EDGE('',*,*,#7237,.F.);
#5191=ORIENTED_EDGE('',*,*,#7246,.T.);
#5192=ORIENTED_EDGE('',*,*,#7247,.T.);
#5193=ORIENTED_EDGE('',*,*,#7248,.T.);
#5194=ORIENTED_EDGE('',*,*,#7249,.T.);
#5195=ORIENTED_EDGE('',*,*,#7250,.T.);
#5196=ORIENTED_EDGE('',*,*,#7251,.T.);
#5197=ORIENTED_EDGE('',*,*,#7252,.F.);
#5198=ORIENTED_EDGE('',*,*,#7249,.F.);
#5199=ORIENTED_EDGE('',*,*,#7253,.T.);
#5200=ORIENTED_EDGE('',*,*,#7254,.T.);
#5201=ORIENTED_EDGE('',*,*,#7255,.F.);
#5202=ORIENTED_EDGE('',*,*,#7247,.F.);
#5203=ORIENTED_EDGE('',*,*,#7256,.T.);
#5204=ORIENTED_EDGE('',*,*,#7257,.F.);
#5205=ORIENTED_EDGE('',*,*,#7258,.T.);
#5206=ORIENTED_EDGE('',*,*,#7259,.F.);
#5207=ORIENTED_EDGE('',*,*,#7260,.T.);
#5208=ORIENTED_EDGE('',*,*,#7261,.F.);
#5209=ORIENTED_EDGE('',*,*,#7262,.T.);
#5210=ORIENTED_EDGE('',*,*,#7263,.F.);
#5211=ORIENTED_EDGE('',*,*,#7264,.T.);
#5212=ORIENTED_EDGE('',*,*,#7265,.F.);
#5213=ORIENTED_EDGE('',*,*,#7266,.F.);
#5214=ORIENTED_EDGE('',*,*,#7267,.F.);
#5215=ORIENTED_EDGE('',*,*,#7268,.F.);
#5216=ORIENTED_EDGE('',*,*,#7269,.F.);
#5217=ORIENTED_EDGE('',*,*,#7270,.F.);
#5218=ORIENTED_EDGE('',*,*,#7271,.F.);
#5219=ORIENTED_EDGE('',*,*,#7272,.F.);
#5220=ORIENTED_EDGE('',*,*,#7273,.F.);
#5221=ORIENTED_EDGE('',*,*,#7274,.F.);
#5222=ORIENTED_EDGE('',*,*,#7275,.T.);
#5223=ORIENTED_EDGE('',*,*,#7276,.T.);
#5224=ORIENTED_EDGE('',*,*,#7277,.T.);
#5225=ORIENTED_EDGE('',*,*,#7278,.T.);
#5226=ORIENTED_EDGE('',*,*,#7279,.T.);
#5227=ORIENTED_EDGE('',*,*,#7280,.T.);
#5228=ORIENTED_EDGE('',*,*,#7281,.T.);
#5229=ORIENTED_EDGE('',*,*,#7282,.T.);
#5230=ORIENTED_EDGE('',*,*,#7283,.F.);
#5231=ORIENTED_EDGE('',*,*,#7284,.F.);
#5232=ORIENTED_EDGE('',*,*,#7285,.F.);
#5233=ORIENTED_EDGE('',*,*,#7284,.T.);
#5234=ORIENTED_EDGE('',*,*,#7286,.F.);
#5235=ORIENTED_EDGE('',*,*,#7264,.F.);
#5236=ORIENTED_EDGE('',*,*,#7286,.T.);
#5237=ORIENTED_EDGE('',*,*,#7283,.T.);
#5238=ORIENTED_EDGE('',*,*,#7287,.T.);
#5239=ORIENTED_EDGE('',*,*,#7265,.T.);
#5240=ORIENTED_EDGE('',*,*,#7285,.T.);
#5241=ORIENTED_EDGE('',*,*,#7263,.T.);
#5242=ORIENTED_EDGE('',*,*,#7288,.T.);
#5243=ORIENTED_EDGE('',*,*,#7274,.T.);
#5244=ORIENTED_EDGE('',*,*,#7289,.T.);
#5245=ORIENTED_EDGE('',*,*,#7290,.T.);
#5246=ORIENTED_EDGE('',*,*,#7291,.T.);
#5247=ORIENTED_EDGE('',*,*,#7292,.T.);
#5248=ORIENTED_EDGE('',*,*,#7293,.T.);
#5249=ORIENTED_EDGE('',*,*,#7294,.F.);
#5250=ORIENTED_EDGE('',*,*,#7260,.F.);
#5251=ORIENTED_EDGE('',*,*,#7295,.T.);
#5252=ORIENTED_EDGE('',*,*,#7296,.T.);
#5253=ORIENTED_EDGE('',*,*,#7297,.T.);
#5254=ORIENTED_EDGE('',*,*,#7258,.F.);
#5255=ORIENTED_EDGE('',*,*,#7298,.T.);
#5256=ORIENTED_EDGE('',*,*,#7299,.T.);
#5257=ORIENTED_EDGE('',*,*,#7300,.F.);
#5258=ORIENTED_EDGE('',*,*,#7301,.F.);
#5259=ORIENTED_EDGE('',*,*,#7302,.F.);
#5260=ORIENTED_EDGE('',*,*,#7299,.F.);
#5261=ORIENTED_EDGE('',*,*,#7303,.T.);
#5262=ORIENTED_EDGE('',*,*,#7304,.T.);
#5263=ORIENTED_EDGE('',*,*,#7305,.T.);
#5264=ORIENTED_EDGE('',*,*,#7306,.F.);
#5265=ORIENTED_EDGE('',*,*,#7261,.T.);
#5266=ORIENTED_EDGE('',*,*,#7300,.T.);
#5267=ORIENTED_EDGE('',*,*,#7305,.F.);
#5268=ORIENTED_EDGE('',*,*,#7298,.F.);
#5269=ORIENTED_EDGE('',*,*,#7257,.T.);
#5270=ORIENTED_EDGE('',*,*,#7307,.T.);
#5271=ORIENTED_EDGE('',*,*,#7303,.F.);
#5272=ORIENTED_EDGE('',*,*,#7307,.F.);
#5273=ORIENTED_EDGE('',*,*,#7262,.F.);
#5274=ORIENTED_EDGE('',*,*,#7306,.T.);
#5275=ORIENTED_EDGE('',*,*,#7304,.F.);
#5276=ORIENTED_EDGE('',*,*,#7308,.F.);
#5277=ORIENTED_EDGE('',*,*,#7244,.F.);
#5278=ORIENTED_EDGE('',*,*,#7309,.F.);
#5279=ORIENTED_EDGE('',*,*,#7241,.F.);
#5280=ORIENTED_EDGE('',*,*,#7292,.F.);
#5281=ORIENTED_EDGE('',*,*,#7310,.F.);
#5282=ORIENTED_EDGE('',*,*,#7311,.T.);
#5283=ORIENTED_EDGE('',*,*,#7296,.F.);
#5284=ORIENTED_EDGE('',*,*,#7312,.T.);
#5285=ORIENTED_EDGE('',*,*,#7254,.F.);
#5286=ORIENTED_EDGE('',*,*,#7313,.F.);
#5287=ORIENTED_EDGE('',*,*,#7251,.F.);
#5288=ORIENTED_EDGE('',*,*,#7314,.F.);
#5289=ORIENTED_EDGE('',*,*,#7267,.T.);
#5290=ORIENTED_EDGE('',*,*,#7266,.T.);
#5291=ORIENTED_EDGE('',*,*,#7287,.F.);
#5292=ORIENTED_EDGE('',*,*,#7282,.F.);
#5293=ORIENTED_EDGE('',*,*,#7281,.F.);
#5294=ORIENTED_EDGE('',*,*,#7280,.F.);
#5295=ORIENTED_EDGE('',*,*,#7279,.F.);
#5296=ORIENTED_EDGE('',*,*,#7278,.F.);
#5297=ORIENTED_EDGE('',*,*,#7277,.F.);
#5298=ORIENTED_EDGE('',*,*,#7276,.F.);
#5299=ORIENTED_EDGE('',*,*,#7275,.F.);
#5300=ORIENTED_EDGE('',*,*,#7311,.F.);
#5301=ORIENTED_EDGE('',*,*,#7288,.F.);
#5302=ORIENTED_EDGE('',*,*,#7273,.T.);
#5303=ORIENTED_EDGE('',*,*,#7272,.T.);
#5304=ORIENTED_EDGE('',*,*,#7271,.T.);
#5305=ORIENTED_EDGE('',*,*,#7270,.T.);
#5306=ORIENTED_EDGE('',*,*,#7269,.T.);
#5307=ORIENTED_EDGE('',*,*,#7268,.T.);
#5308=ORIENTED_EDGE('',*,*,#7302,.T.);
#5309=ORIENTED_EDGE('',*,*,#7310,.T.);
#5310=ORIENTED_EDGE('',*,*,#7291,.F.);
#5311=ORIENTED_EDGE('',*,*,#7315,.F.);
#5312=ORIENTED_EDGE('',*,*,#7289,.F.);
#5313=ORIENTED_EDGE('',*,*,#7301,.T.);
#5314=ORIENTED_EDGE('',*,*,#7293,.F.);
#5315=ORIENTED_EDGE('',*,*,#7294,.T.);
#5316=ORIENTED_EDGE('',*,*,#7316,.F.);
#5317=ORIENTED_EDGE('',*,*,#7290,.F.);
#5318=ORIENTED_EDGE('',*,*,#7315,.T.);
#5319=ORIENTED_EDGE('',*,*,#7316,.T.);
#5320=ORIENTED_EDGE('',*,*,#7259,.T.);
#5321=ORIENTED_EDGE('',*,*,#7297,.F.);
#5322=ORIENTED_EDGE('',*,*,#7312,.F.);
#5323=ORIENTED_EDGE('',*,*,#7295,.F.);
#5324=ORIENTED_EDGE('',*,*,#7250,.F.);
#5325=ORIENTED_EDGE('',*,*,#7252,.T.);
#5326=ORIENTED_EDGE('',*,*,#7313,.T.);
#5327=ORIENTED_EDGE('',*,*,#7256,.F.);
#5328=ORIENTED_EDGE('',*,*,#7248,.F.);
#5329=ORIENTED_EDGE('',*,*,#7255,.T.);
#5330=ORIENTED_EDGE('',*,*,#7314,.T.);
#5331=ORIENTED_EDGE('',*,*,#7253,.F.);
#5332=ORIENTED_EDGE('',*,*,#7238,.F.);
#5333=ORIENTED_EDGE('',*,*,#7245,.T.);
#5334=ORIENTED_EDGE('',*,*,#7308,.T.);
#5335=ORIENTED_EDGE('',*,*,#7243,.F.);
#5336=ORIENTED_EDGE('',*,*,#7240,.F.);
#5337=ORIENTED_EDGE('',*,*,#7242,.T.);
#5338=ORIENTED_EDGE('',*,*,#7309,.T.);
#5339=ORIENTED_EDGE('',*,*,#7246,.F.);
#5340=ORIENTED_EDGE('',*,*,#7317,.T.);
#5341=ORIENTED_EDGE('',*,*,#7318,.F.);
#5342=ORIENTED_EDGE('',*,*,#7319,.T.);
#5343=ORIENTED_EDGE('',*,*,#7320,.T.);
#5344=ORIENTED_EDGE('',*,*,#7321,.T.);
#5345=ORIENTED_EDGE('',*,*,#7322,.T.);
#5346=ORIENTED_EDGE('',*,*,#7323,.F.);
#5347=ORIENTED_EDGE('',*,*,#7324,.T.);
#5348=ORIENTED_EDGE('',*,*,#7318,.T.);
#5349=ORIENTED_EDGE('',*,*,#7325,.T.);
#5350=ORIENTED_EDGE('',*,*,#7326,.F.);
#5351=ORIENTED_EDGE('',*,*,#7327,.T.);
#5352=ORIENTED_EDGE('',*,*,#7328,.T.);
#5353=ORIENTED_EDGE('',*,*,#7323,.T.);
#5354=ORIENTED_EDGE('',*,*,#7329,.F.);
#5355=ORIENTED_EDGE('',*,*,#7326,.T.);
#5356=ORIENTED_EDGE('',*,*,#7330,.T.);
#5357=ORIENTED_EDGE('',*,*,#7321,.F.);
#5358=ORIENTED_EDGE('',*,*,#7331,.T.);
#5359=ORIENTED_EDGE('',*,*,#7332,.F.);
#5360=ORIENTED_EDGE('',*,*,#7333,.T.);
#5361=ORIENTED_EDGE('',*,*,#7334,.T.);
#5362=ORIENTED_EDGE('',*,*,#7335,.T.);
#5363=ORIENTED_EDGE('',*,*,#7336,.T.);
#5364=ORIENTED_EDGE('',*,*,#7337,.F.);
#5365=ORIENTED_EDGE('',*,*,#7338,.T.);
#5366=ORIENTED_EDGE('',*,*,#7332,.T.);
#5367=ORIENTED_EDGE('',*,*,#7339,.T.);
#5368=ORIENTED_EDGE('',*,*,#7340,.F.);
#5369=ORIENTED_EDGE('',*,*,#7341,.T.);
#5370=ORIENTED_EDGE('',*,*,#7342,.T.);
#5371=ORIENTED_EDGE('',*,*,#7337,.T.);
#5372=ORIENTED_EDGE('',*,*,#7343,.F.);
#5373=ORIENTED_EDGE('',*,*,#7340,.T.);
#5374=ORIENTED_EDGE('',*,*,#7344,.T.);
#5375=ORIENTED_EDGE('',*,*,#7335,.F.);
#5376=ORIENTED_EDGE('',*,*,#7345,.T.);
#5377=ORIENTED_EDGE('',*,*,#7346,.F.);
#5378=ORIENTED_EDGE('',*,*,#7347,.T.);
#5379=ORIENTED_EDGE('',*,*,#7348,.T.);
#5380=ORIENTED_EDGE('',*,*,#7349,.T.);
#5381=ORIENTED_EDGE('',*,*,#7350,.T.);
#5382=ORIENTED_EDGE('',*,*,#7351,.F.);
#5383=ORIENTED_EDGE('',*,*,#7352,.T.);
#5384=ORIENTED_EDGE('',*,*,#7346,.T.);
#5385=ORIENTED_EDGE('',*,*,#7353,.T.);
#5386=ORIENTED_EDGE('',*,*,#7354,.F.);
#5387=ORIENTED_EDGE('',*,*,#7355,.T.);
#5388=ORIENTED_EDGE('',*,*,#7356,.T.);
#5389=ORIENTED_EDGE('',*,*,#7351,.T.);
#5390=ORIENTED_EDGE('',*,*,#7357,.F.);
#5391=ORIENTED_EDGE('',*,*,#7354,.T.);
#5392=ORIENTED_EDGE('',*,*,#7358,.T.);
#5393=ORIENTED_EDGE('',*,*,#7349,.F.);
#5394=ORIENTED_EDGE('',*,*,#7359,.T.);
#5395=ORIENTED_EDGE('',*,*,#7360,.F.);
#5396=ORIENTED_EDGE('',*,*,#7361,.T.);
#5397=ORIENTED_EDGE('',*,*,#7362,.T.);
#5398=ORIENTED_EDGE('',*,*,#7363,.T.);
#5399=ORIENTED_EDGE('',*,*,#7364,.F.);
#5400=ORIENTED_EDGE('',*,*,#7365,.F.);
#5401=ORIENTED_EDGE('',*,*,#7366,.T.);
#5402=ORIENTED_EDGE('',*,*,#7360,.T.);
#5403=ORIENTED_EDGE('',*,*,#7367,.T.);
#5404=ORIENTED_EDGE('',*,*,#7368,.F.);
#5405=ORIENTED_EDGE('',*,*,#7369,.T.);
#5406=ORIENTED_EDGE('',*,*,#7370,.T.);
#5407=ORIENTED_EDGE('',*,*,#7365,.T.);
#5408=ORIENTED_EDGE('',*,*,#7371,.F.);
#5409=ORIENTED_EDGE('',*,*,#7368,.T.);
#5410=ORIENTED_EDGE('',*,*,#7372,.T.);
#5411=ORIENTED_EDGE('',*,*,#7363,.F.);
#5412=ORIENTED_EDGE('',*,*,#7373,.F.);
#5413=ORIENTED_EDGE('',*,*,#7371,.T.);
#5414=ORIENTED_EDGE('',*,*,#7374,.T.);
#5415=ORIENTED_EDGE('',*,*,#7343,.T.);
#5416=ORIENTED_EDGE('',*,*,#7375,.T.);
#5417=ORIENTED_EDGE('',*,*,#7357,.T.);
#5418=ORIENTED_EDGE('',*,*,#7376,.T.);
#5419=ORIENTED_EDGE('',*,*,#7329,.T.);
#5420=ORIENTED_EDGE('',*,*,#7377,.T.);
#5421=ORIENTED_EDGE('',*,*,#7378,.T.);
#5422=ORIENTED_EDGE('',*,*,#7328,.F.);
#5423=ORIENTED_EDGE('',*,*,#7379,.F.);
#5424=ORIENTED_EDGE('',*,*,#7347,.F.);
#5425=ORIENTED_EDGE('',*,*,#7352,.F.);
#5426=ORIENTED_EDGE('',*,*,#7356,.F.);
#5427=ORIENTED_EDGE('',*,*,#7380,.F.);
#5428=ORIENTED_EDGE('',*,*,#7333,.F.);
#5429=ORIENTED_EDGE('',*,*,#7338,.F.);
#5430=ORIENTED_EDGE('',*,*,#7342,.F.);
#5431=ORIENTED_EDGE('',*,*,#7381,.F.);
#5432=ORIENTED_EDGE('',*,*,#7361,.F.);
#5433=ORIENTED_EDGE('',*,*,#7366,.F.);
#5434=ORIENTED_EDGE('',*,*,#7370,.F.);
#5435=ORIENTED_EDGE('',*,*,#7382,.F.);
#5436=ORIENTED_EDGE('',*,*,#7319,.F.);
#5437=ORIENTED_EDGE('',*,*,#7324,.F.);
#5438=ORIENTED_EDGE('',*,*,#7383,.F.);
#5439=ORIENTED_EDGE('',*,*,#7364,.T.);
#5440=ORIENTED_EDGE('',*,*,#7384,.T.);
#5441=ORIENTED_EDGE('',*,*,#7336,.F.);
#5442=ORIENTED_EDGE('',*,*,#7385,.T.);
#5443=ORIENTED_EDGE('',*,*,#7350,.F.);
#5444=ORIENTED_EDGE('',*,*,#7386,.T.);
#5445=ORIENTED_EDGE('',*,*,#7322,.F.);
#5446=ORIENTED_EDGE('',*,*,#7387,.T.);
#5447=ORIENTED_EDGE('',*,*,#7372,.F.);
#5448=ORIENTED_EDGE('',*,*,#7388,.F.);
#5449=ORIENTED_EDGE('',*,*,#7330,.F.);
#5450=ORIENTED_EDGE('',*,*,#7389,.F.);
#5451=ORIENTED_EDGE('',*,*,#7358,.F.);
#5452=ORIENTED_EDGE('',*,*,#7390,.F.);
#5453=ORIENTED_EDGE('',*,*,#7344,.F.);
#5454=ORIENTED_EDGE('',*,*,#7391,.F.);
#5455=ORIENTED_EDGE('',*,*,#7392,.T.);
#5456=ORIENTED_EDGE('',*,*,#7334,.F.);
#5457=ORIENTED_EDGE('',*,*,#7380,.T.);
#5458=ORIENTED_EDGE('',*,*,#7355,.F.);
#5459=ORIENTED_EDGE('',*,*,#7375,.F.);
#5460=ORIENTED_EDGE('',*,*,#7341,.F.);
#5461=ORIENTED_EDGE('',*,*,#7374,.F.);
#5462=ORIENTED_EDGE('',*,*,#7362,.F.);
#5463=ORIENTED_EDGE('',*,*,#7381,.T.);
#5464=ORIENTED_EDGE('',*,*,#7327,.F.);
#5465=ORIENTED_EDGE('',*,*,#7376,.F.);
#5466=ORIENTED_EDGE('',*,*,#7348,.F.);
#5467=ORIENTED_EDGE('',*,*,#7379,.T.);
#5468=ORIENTED_EDGE('',*,*,#7331,.F.);
#5469=ORIENTED_EDGE('',*,*,#7390,.T.);
#5470=ORIENTED_EDGE('',*,*,#7353,.F.);
#5471=ORIENTED_EDGE('',*,*,#7385,.F.);
#5472=ORIENTED_EDGE('',*,*,#7339,.F.);
#5473=ORIENTED_EDGE('',*,*,#7384,.F.);
#5474=ORIENTED_EDGE('',*,*,#7359,.F.);
#5475=ORIENTED_EDGE('',*,*,#7391,.T.);
#5476=ORIENTED_EDGE('',*,*,#7325,.F.);
#5477=ORIENTED_EDGE('',*,*,#7386,.F.);
#5478=ORIENTED_EDGE('',*,*,#7345,.F.);
#5479=ORIENTED_EDGE('',*,*,#7389,.T.);
#5480=ORIENTED_EDGE('',*,*,#7373,.T.);
#5481=ORIENTED_EDGE('',*,*,#7392,.F.);
#5482=ORIENTED_EDGE('',*,*,#7388,.T.);
#5483=ORIENTED_EDGE('',*,*,#7367,.F.);
#5484=ORIENTED_EDGE('',*,*,#7387,.F.);
#5485=ORIENTED_EDGE('',*,*,#7317,.F.);
#5486=ORIENTED_EDGE('',*,*,#7393,.F.);
#5487=ORIENTED_EDGE('',*,*,#7383,.T.);
#5488=ORIENTED_EDGE('',*,*,#7378,.F.);
#5489=ORIENTED_EDGE('',*,*,#7393,.T.);
#5490=ORIENTED_EDGE('',*,*,#7377,.F.);
#5491=ORIENTED_EDGE('',*,*,#7320,.F.);
#5492=ORIENTED_EDGE('',*,*,#7382,.T.);
#5493=ORIENTED_EDGE('',*,*,#7369,.F.);
#5494=ORIENTED_EDGE('',*,*,#7394,.F.);
#5495=ORIENTED_EDGE('',*,*,#7395,.T.);
#5496=ORIENTED_EDGE('',*,*,#7396,.F.);
#5497=ORIENTED_EDGE('',*,*,#7397,.T.);
#5498=ORIENTED_EDGE('',*,*,#7398,.T.);
#5499=ORIENTED_EDGE('',*,*,#7399,.F.);
#5500=ORIENTED_EDGE('',*,*,#7397,.F.);
#5501=ORIENTED_EDGE('',*,*,#7400,.T.);
#5502=ORIENTED_EDGE('',*,*,#7401,.F.);
#5503=ORIENTED_EDGE('',*,*,#7402,.F.);
#5504=ORIENTED_EDGE('',*,*,#7398,.F.);
#5505=ORIENTED_EDGE('',*,*,#7403,.F.);
#5506=ORIENTED_EDGE('',*,*,#7404,.T.);
#5507=ORIENTED_EDGE('',*,*,#7405,.F.);
#5508=ORIENTED_EDGE('',*,*,#7400,.F.);
#5509=ORIENTED_EDGE('',*,*,#7406,.F.);
#5510=ORIENTED_EDGE('',*,*,#7407,.T.);
#5511=ORIENTED_EDGE('',*,*,#7408,.F.);
#5512=ORIENTED_EDGE('',*,*,#7404,.F.);
#5513=ORIENTED_EDGE('',*,*,#7409,.F.);
#5514=ORIENTED_EDGE('',*,*,#7410,.T.);
#5515=ORIENTED_EDGE('',*,*,#7411,.F.);
#5516=ORIENTED_EDGE('',*,*,#7412,.T.);
#5517=ORIENTED_EDGE('',*,*,#7413,.T.);
#5518=ORIENTED_EDGE('',*,*,#7412,.F.);
#5519=ORIENTED_EDGE('',*,*,#7414,.F.);
#5520=ORIENTED_EDGE('',*,*,#7415,.T.);
#5521=ORIENTED_EDGE('',*,*,#7416,.F.);
#5522=ORIENTED_EDGE('',*,*,#7413,.F.);
#5523=ORIENTED_EDGE('',*,*,#7417,.F.);
#5524=ORIENTED_EDGE('',*,*,#7418,.F.);
#5525=ORIENTED_EDGE('',*,*,#7419,.T.);
#5526=ORIENTED_EDGE('',*,*,#7415,.F.);
#5527=ORIENTED_EDGE('',*,*,#7420,.F.);
#5528=ORIENTED_EDGE('',*,*,#7421,.F.);
#5529=ORIENTED_EDGE('',*,*,#7422,.T.);
#5530=ORIENTED_EDGE('',*,*,#7423,.F.);
#5531=ORIENTED_EDGE('',*,*,#7419,.F.);
#5532=ORIENTED_EDGE('',*,*,#7424,.F.);
#5533=ORIENTED_EDGE('',*,*,#7425,.T.);
#5534=ORIENTED_EDGE('',*,*,#7421,.T.);
#5535=ORIENTED_EDGE('',*,*,#7426,.F.);
#5536=ORIENTED_EDGE('',*,*,#7408,.T.);
#5537=ORIENTED_EDGE('',*,*,#7427,.T.);
#5538=ORIENTED_EDGE('',*,*,#7428,.F.);
#5539=ORIENTED_EDGE('',*,*,#7429,.F.);
#5540=ORIENTED_EDGE('',*,*,#7430,.F.);
#5541=ORIENTED_EDGE('',*,*,#7431,.F.);
#5542=ORIENTED_EDGE('',*,*,#7432,.F.);
#5543=ORIENTED_EDGE('',*,*,#7433,.F.);
#5544=ORIENTED_EDGE('',*,*,#7403,.T.);
#5545=ORIENTED_EDGE('',*,*,#7396,.T.);
#5546=ORIENTED_EDGE('',*,*,#7434,.T.);
#5547=ORIENTED_EDGE('',*,*,#7435,.F.);
#5548=ORIENTED_EDGE('',*,*,#7436,.T.);
#5549=ORIENTED_EDGE('',*,*,#7406,.T.);
#5550=ORIENTED_EDGE('',*,*,#7437,.F.);
#5551=ORIENTED_EDGE('',*,*,#7438,.T.);
#5552=ORIENTED_EDGE('',*,*,#7409,.T.);
#5553=ORIENTED_EDGE('',*,*,#7416,.T.);
#5554=ORIENTED_EDGE('',*,*,#7423,.T.);
#5555=ORIENTED_EDGE('',*,*,#7439,.T.);
#5556=ORIENTED_EDGE('',*,*,#7440,.F.);
#5557=ORIENTED_EDGE('',*,*,#7411,.T.);
#5558=ORIENTED_EDGE('',*,*,#7441,.T.);
#5559=ORIENTED_EDGE('',*,*,#7442,.F.);
#5560=ORIENTED_EDGE('',*,*,#7443,.F.);
#5561=ORIENTED_EDGE('',*,*,#7444,.F.);
#5562=ORIENTED_EDGE('',*,*,#7445,.F.);
#5563=ORIENTED_EDGE('',*,*,#7446,.F.);
#5564=ORIENTED_EDGE('',*,*,#7447,.F.);
#5565=ORIENTED_EDGE('',*,*,#7448,.F.);
#5566=ORIENTED_EDGE('',*,*,#7449,.T.);
#5567=ORIENTED_EDGE('',*,*,#7394,.T.);
#5568=ORIENTED_EDGE('',*,*,#7450,.T.);
#5569=ORIENTED_EDGE('',*,*,#7451,.T.);
#5570=ORIENTED_EDGE('',*,*,#7452,.T.);
#5571=ORIENTED_EDGE('',*,*,#7453,.T.);
#5572=ORIENTED_EDGE('',*,*,#7454,.T.);
#5573=ORIENTED_EDGE('',*,*,#7455,.T.);
#5574=ORIENTED_EDGE('',*,*,#7410,.F.);
#5575=ORIENTED_EDGE('',*,*,#7438,.F.);
#5576=ORIENTED_EDGE('',*,*,#7441,.F.);
#5577=ORIENTED_EDGE('',*,*,#7422,.F.);
#5578=ORIENTED_EDGE('',*,*,#7425,.F.);
#5579=ORIENTED_EDGE('',*,*,#7439,.F.);
#5580=ORIENTED_EDGE('',*,*,#7395,.F.);
#5581=ORIENTED_EDGE('',*,*,#7449,.F.);
#5582=ORIENTED_EDGE('',*,*,#7434,.F.);
#5583=ORIENTED_EDGE('',*,*,#7407,.F.);
#5584=ORIENTED_EDGE('',*,*,#7436,.F.);
#5585=ORIENTED_EDGE('',*,*,#7427,.F.);
#5586=ORIENTED_EDGE('',*,*,#7447,.T.);
#5587=ORIENTED_EDGE('',*,*,#7446,.T.);
#5588=ORIENTED_EDGE('',*,*,#7445,.T.);
#5589=ORIENTED_EDGE('',*,*,#7444,.T.);
#5590=ORIENTED_EDGE('',*,*,#7443,.T.);
#5591=ORIENTED_EDGE('',*,*,#7442,.T.);
#5592=ORIENTED_EDGE('',*,*,#7437,.T.);
#5593=ORIENTED_EDGE('',*,*,#7424,.T.);
#5594=ORIENTED_EDGE('',*,*,#7433,.T.);
#5595=ORIENTED_EDGE('',*,*,#7432,.T.);
#5596=ORIENTED_EDGE('',*,*,#7431,.T.);
#5597=ORIENTED_EDGE('',*,*,#7430,.T.);
#5598=ORIENTED_EDGE('',*,*,#7429,.T.);
#5599=ORIENTED_EDGE('',*,*,#7428,.T.);
#5600=ORIENTED_EDGE('',*,*,#7435,.T.);
#5601=ORIENTED_EDGE('',*,*,#7448,.T.);
#5602=ORIENTED_EDGE('',*,*,#7456,.T.);
#5603=ORIENTED_EDGE('',*,*,#7457,.T.);
#5604=ORIENTED_EDGE('',*,*,#7458,.T.);
#5605=ORIENTED_EDGE('',*,*,#7450,.F.);
#5606=ORIENTED_EDGE('',*,*,#7454,.F.);
#5607=ORIENTED_EDGE('',*,*,#7459,.T.);
#5608=ORIENTED_EDGE('',*,*,#7402,.T.);
#5609=ORIENTED_EDGE('',*,*,#7401,.T.);
#5610=ORIENTED_EDGE('',*,*,#7405,.T.);
#5611=ORIENTED_EDGE('',*,*,#7426,.T.);
#5612=ORIENTED_EDGE('',*,*,#7420,.T.);
#5613=ORIENTED_EDGE('',*,*,#7418,.T.);
#5614=ORIENTED_EDGE('',*,*,#7417,.T.);
#5615=ORIENTED_EDGE('',*,*,#7414,.T.);
#5616=ORIENTED_EDGE('',*,*,#7440,.T.);
#5617=ORIENTED_EDGE('',*,*,#7399,.T.);
#5618=ORIENTED_EDGE('',*,*,#7455,.F.);
#5619=ORIENTED_EDGE('',*,*,#7457,.F.);
#5620=ORIENTED_EDGE('',*,*,#7452,.F.);
#5621=ORIENTED_EDGE('',*,*,#7456,.F.);
#5622=ORIENTED_EDGE('',*,*,#7453,.F.);
#5623=ORIENTED_EDGE('',*,*,#7458,.F.);
#5624=ORIENTED_EDGE('',*,*,#7459,.F.);
#5625=ORIENTED_EDGE('',*,*,#7451,.F.);
#5626=ORIENTED_EDGE('',*,*,#7460,.F.);
#5627=ORIENTED_EDGE('',*,*,#7461,.T.);
#5628=ORIENTED_EDGE('',*,*,#7461,.F.);
#5629=ORIENTED_EDGE('',*,*,#7460,.T.);
#5630=EDGE_CURVE('',#7462,#7463,#8773,.T.);
#5631=EDGE_CURVE('',#7463,#7464,#1826,.T.);
#5632=EDGE_CURVE('',#7464,#7465,#1827,.T.);
#5633=EDGE_CURVE('',#7465,#7466,#1828,.T.);
#5634=EDGE_CURVE('',#7466,#7467,#1829,.T.);
#5635=EDGE_CURVE('',#7467,#7468,#1830,.T.);
#5636=EDGE_CURVE('',#7468,#7469,#1831,.T.);
#5637=EDGE_CURVE('',#7469,#7470,#1832,.T.);
#5638=EDGE_CURVE('',#7470,#7471,#8774,.T.);
#5639=EDGE_CURVE('',#7462,#7471,#1833,.T.);
#5640=EDGE_CURVE('',#7472,#7462,#8775,.T.);
#5641=EDGE_CURVE('',#7471,#7473,#8776,.T.);
#5642=EDGE_CURVE('',#7472,#7473,#1834,.T.);
#5643=EDGE_CURVE('',#7474,#7470,#8777,.T.);
#5644=EDGE_CURVE('',#7473,#7474,#8778,.T.);
#5645=EDGE_CURVE('',#7475,#7476,#1062,.T.);
#5646=EDGE_CURVE('',#7476,#7472,#8779,.T.);
#5647=EDGE_CURVE('',#7477,#7474,#1835,.T.);
#5648=EDGE_CURVE('',#7478,#7477,#1836,.T.);
#5649=EDGE_CURVE('',#7479,#7478,#1837,.T.);
#5650=EDGE_CURVE('',#7480,#7479,#1838,.T.);
#5651=EDGE_CURVE('',#7481,#7480,#1839,.T.);
#5652=EDGE_CURVE('',#7482,#7481,#1840,.T.);
#5653=EDGE_CURVE('',#7475,#7482,#1841,.T.);
#5654=EDGE_CURVE('',#7463,#7483,#8780,.T.);
#5655=EDGE_CURVE('',#7483,#7476,#8781,.T.);
#5656=EDGE_CURVE('',#7484,#7484,#337,.T.);
#5657=EDGE_CURVE('',#7483,#7475,#338,.T.);
#5658=EDGE_CURVE('',#7485,#7486,#1063,.T.);
#5659=EDGE_CURVE('',#7485,#7487,#339,.T.);
#5660=EDGE_CURVE('',#7487,#7488,#1064,.T.);
#5661=EDGE_CURVE('',#7486,#7488,#340,.T.);
#5662=EDGE_CURVE('',#7488,#7486,#341,.T.);
#5663=EDGE_CURVE('',#7489,#7489,#342,.T.);
#5664=EDGE_CURVE('',#7490,#7490,#343,.T.);
#5665=EDGE_CURVE('',#7491,#7491,#344,.T.);
#5666=EDGE_CURVE('',#7492,#7493,#8782,.T.);
#5667=EDGE_CURVE('',#7494,#7493,#8783,.T.);
#5668=EDGE_CURVE('',#7495,#7494,#8784,.T.);
#5669=EDGE_CURVE('',#7495,#7492,#8785,.T.);
#5670=EDGE_CURVE('',#7496,#7497,#8786,.T.);
#5671=EDGE_CURVE('',#7498,#7497,#8787,.T.);
#5672=EDGE_CURVE('',#7499,#7498,#8788,.T.);
#5673=EDGE_CURVE('',#7499,#7496,#8789,.T.);
#5674=EDGE_CURVE('',#7497,#7492,#345,.T.);
#5675=EDGE_CURVE('',#7498,#7495,#346,.T.);
#5676=EDGE_CURVE('',#7500,#7501,#8790,.T.);
#5677=EDGE_CURVE('',#7502,#7501,#8791,.T.);
#5678=EDGE_CURVE('',#7503,#7502,#8792,.T.);
#5679=EDGE_CURVE('',#7503,#7500,#8793,.T.);
#5680=EDGE_CURVE('',#7504,#7505,#8794,.T.);
#5681=EDGE_CURVE('',#7506,#7505,#8795,.T.);
#5682=EDGE_CURVE('',#7507,#7506,#8796,.T.);
#5683=EDGE_CURVE('',#7507,#7504,#8797,.T.);
#5684=EDGE_CURVE('',#7505,#7500,#347,.T.);
#5685=EDGE_CURVE('',#7506,#7503,#348,.T.);
#5686=EDGE_CURVE('',#7508,#7509,#8798,.T.);
#5687=EDGE_CURVE('',#7510,#7509,#8799,.T.);
#5688=EDGE_CURVE('',#7511,#7510,#8800,.T.);
#5689=EDGE_CURVE('',#7511,#7508,#8801,.T.);
#5690=EDGE_CURVE('',#7512,#7513,#8802,.T.);
#5691=EDGE_CURVE('',#7514,#7513,#8803,.T.);
#5692=EDGE_CURVE('',#7515,#7514,#8804,.T.);
#5693=EDGE_CURVE('',#7515,#7512,#8805,.T.);
#5694=EDGE_CURVE('',#7513,#7508,#349,.T.);
#5695=EDGE_CURVE('',#7514,#7511,#350,.T.);
#5696=EDGE_CURVE('',#7516,#7516,#351,.T.);
#5697=EDGE_CURVE('',#7517,#7517,#352,.T.);
#5698=EDGE_CURVE('',#7518,#7518,#353,.T.);
#5699=EDGE_CURVE('',#7519,#7519,#354,.T.);
#5700=EDGE_CURVE('',#7520,#7520,#355,.T.);
#5701=EDGE_CURVE('',#7521,#7521,#356,.T.);
#5702=EDGE_CURVE('',#7522,#7522,#357,.T.);
#5703=EDGE_CURVE('',#7523,#7523,#358,.T.);
#5704=EDGE_CURVE('',#7524,#7524,#359,.T.);
#5705=EDGE_CURVE('',#7525,#7525,#360,.T.);
#5706=EDGE_CURVE('',#7526,#7526,#361,.T.);
#5707=EDGE_CURVE('',#7527,#7527,#362,.T.);
#5708=EDGE_CURVE('',#7528,#7528,#363,.T.);
#5709=EDGE_CURVE('',#7529,#7529,#364,.T.);
#5710=EDGE_CURVE('',#7530,#7530,#365,.T.);
#5711=EDGE_CURVE('',#7531,#7531,#366,.T.);
#5712=EDGE_CURVE('',#7532,#7532,#367,.T.);
#5713=EDGE_CURVE('',#7510,#7515,#368,.T.);
#5714=EDGE_CURVE('',#7502,#7507,#369,.T.);
#5715=EDGE_CURVE('',#7494,#7499,#370,.T.);
#5716=EDGE_CURVE('',#7533,#7533,#371,.T.);
#5717=EDGE_CURVE('',#7534,#7534,#372,.T.);
#5718=EDGE_CURVE('',#7535,#7535,#373,.T.);
#5719=EDGE_CURVE('',#7536,#7536,#374,.T.);
#5720=EDGE_CURVE('',#7537,#7537,#375,.T.);
#5721=EDGE_CURVE('',#7538,#7538,#376,.T.);
#5722=EDGE_CURVE('',#7539,#7539,#377,.T.);
#5723=EDGE_CURVE('',#7540,#7540,#378,.T.);
#5724=EDGE_CURVE('',#7541,#7541,#379,.T.);
#5725=EDGE_CURVE('',#7542,#7542,#380,.T.);
#5726=EDGE_CURVE('',#7509,#7512,#381,.T.);
#5727=EDGE_CURVE('',#7501,#7504,#382,.T.);
#5728=EDGE_CURVE('',#7493,#7496,#383,.T.);
#5729=EDGE_CURVE('',#7543,#7543,#384,.T.);
#5730=EDGE_CURVE('',#7544,#7544,#385,.T.);
#5731=EDGE_CURVE('',#7545,#7545,#386,.T.);
#5732=EDGE_CURVE('',#7546,#7546,#387,.T.);
#5733=EDGE_CURVE('',#7547,#7547,#388,.T.);
#5734=EDGE_CURVE('',#7548,#7548,#389,.T.);
#5735=EDGE_CURVE('',#7487,#7485,#390,.T.);
#5736=EDGE_CURVE('',#7549,#7549,#391,.T.);
#5737=EDGE_CURVE('',#7550,#7550,#392,.T.);
#5738=EDGE_CURVE('',#7551,#7551,#393,.T.);
#5739=EDGE_CURVE('',#7552,#7552,#394,.T.);
#5740=EDGE_CURVE('',#7553,#7554,#8806,.T.);
#5741=EDGE_CURVE('',#7553,#7555,#1842,.T.);
#5742=EDGE_CURVE('',#7556,#7555,#8807,.T.);
#5743=EDGE_CURVE('',#7556,#7557,#8808,.T.);
#5744=EDGE_CURVE('',#7557,#7558,#1065,.T.);
#5745=EDGE_CURVE('',#7559,#7558,#395,.T.);
#5746=EDGE_CURVE('',#7560,#7559,#1843,.T.);
#5747=EDGE_CURVE('',#7561,#7560,#1844,.T.);
#5748=EDGE_CURVE('',#7554,#7561,#1845,.T.);
#5749=EDGE_CURVE('',#7562,#7563,#8809,.T.);
#5750=EDGE_CURVE('',#7562,#7564,#1846,.T.);
#5751=EDGE_CURVE('',#7564,#7565,#1847,.T.);
#5752=EDGE_CURVE('',#7565,#7566,#1848,.T.);
#5753=EDGE_CURVE('',#7566,#7567,#1849,.T.);
#5754=EDGE_CURVE('',#7568,#7567,#8810,.T.);
#5755=EDGE_CURVE('',#7563,#7568,#1850,.T.);
#5756=EDGE_CURVE('',#7563,#7553,#8811,.T.);
#5757=EDGE_CURVE('',#7555,#7568,#8812,.T.);
#5758=EDGE_CURVE('',#7567,#7569,#8813,.T.);
#5759=EDGE_CURVE('',#7569,#7557,#396,.T.);
#5760=EDGE_CURVE('',#7554,#7562,#8814,.T.);
#5761=EDGE_CURVE('',#7570,#7570,#397,.T.);
#5762=EDGE_CURVE('',#7571,#7571,#398,.T.);
#5763=EDGE_CURVE('',#7572,#7572,#399,.T.);
#5764=EDGE_CURVE('',#7573,#7573,#400,.T.);
#5765=EDGE_CURVE('',#7574,#7574,#401,.T.);
#5766=EDGE_CURVE('',#7575,#7575,#402,.T.);
#5767=EDGE_CURVE('',#7576,#7576,#403,.T.);
#5768=EDGE_CURVE('',#7577,#7577,#404,.T.);
#5769=EDGE_CURVE('',#7578,#7578,#405,.T.);
#5770=EDGE_CURVE('',#7579,#7579,#406,.T.);
#5771=EDGE_CURVE('',#7580,#7580,#407,.T.);
#5772=EDGE_CURVE('',#7581,#7581,#408,.T.);
#5773=EDGE_CURVE('',#7582,#7582,#409,.T.);
#5774=EDGE_CURVE('',#7583,#7583,#410,.T.);
#5775=EDGE_CURVE('',#7584,#7584,#411,.T.);
#5776=EDGE_CURVE('',#7585,#7585,#412,.T.);
#5777=EDGE_CURVE('',#7586,#7586,#413,.T.);
#5778=EDGE_CURVE('',#7587,#7587,#414,.T.);
#5779=EDGE_CURVE('',#7588,#7588,#415,.T.);
#5780=EDGE_CURVE('',#7558,#7569,#416,.T.);
#5781=EDGE_CURVE('',#7589,#7589,#417,.T.);
#5782=EDGE_CURVE('',#7590,#7590,#418,.T.);
#5783=EDGE_CURVE('',#7591,#7591,#419,.T.);
#5784=EDGE_CURVE('',#7592,#7592,#420,.T.);
#5785=EDGE_CURVE('',#7593,#7593,#421,.T.);
#5786=EDGE_CURVE('',#7594,#7594,#422,.T.);
#5787=EDGE_CURVE('',#7595,#7595,#423,.T.);
#5788=EDGE_CURVE('',#7596,#7596,#424,.T.);
#5789=EDGE_CURVE('',#7597,#7597,#425,.T.);
#5790=EDGE_CURVE('',#7598,#7598,#426,.T.);
#5791=EDGE_CURVE('',#7599,#7599,#427,.T.);
#5792=EDGE_CURVE('',#7600,#7600,#428,.T.);
#5793=EDGE_CURVE('',#7601,#7601,#429,.T.);
#5794=EDGE_CURVE('',#7602,#7602,#430,.T.);
#5795=EDGE_CURVE('',#7603,#7604,#8815,.T.);
#5796=EDGE_CURVE('',#7603,#7604,#1066,.F.);
#5797=EDGE_CURVE('',#7603,#7604,#1067,.T.);
#5798=EDGE_CURVE('',#7605,#7606,#8816,.T.);
#5799=EDGE_CURVE('',#7605,#7606,#1068,.T.);
#5800=EDGE_CURVE('',#7607,#7608,#1069,.F.);
#5801=EDGE_CURVE('',#7607,#7603,#1070,.T.);
#5802=EDGE_CURVE('',#7604,#7608,#1071,.T.);
#5803=EDGE_CURVE('',#7608,#7607,#1072,.F.);
#5804=EDGE_CURVE('',#7605,#7606,#1073,.F.);
#5805=EDGE_CURVE('',#7609,#7610,#1074,.F.);
#5806=EDGE_CURVE('',#7606,#7609,#1075,.F.);
#5807=EDGE_CURVE('',#7610,#7605,#1076,.F.);
#5808=EDGE_CURVE('',#7611,#7608,#1077,.F.);
#5809=EDGE_CURVE('',#7612,#7611,#1078,.F.);
#5810=EDGE_CURVE('',#7607,#7612,#1079,.F.);
#5811=EDGE_CURVE('',#7611,#7612,#1080,.F.);
#5812=EDGE_CURVE('',#7610,#7609,#1081,.F.);
#5813=EDGE_CURVE('',#7610,#7613,#1082,.T.);
#5814=EDGE_CURVE('',#7614,#7613,#1083,.F.);
#5815=EDGE_CURVE('',#7614,#7609,#1084,.T.);
#5816=EDGE_CURVE('',#7615,#7612,#1085,.T.);
#5817=EDGE_CURVE('',#7611,#7616,#1086,.T.);
#5818=EDGE_CURVE('',#7615,#7616,#1087,.F.);
#5819=EDGE_CURVE('',#7616,#7615,#1088,.F.);
#5820=EDGE_CURVE('',#7613,#7614,#1089,.F.);
#5821=EDGE_CURVE('',#7615,#7613,#1090,.F.);
#5822=EDGE_CURVE('',#7614,#7616,#1091,.F.);
#5823=EDGE_CURVE('',#7617,#7618,#1851,.T.);
#5824=EDGE_CURVE('',#7617,#7619,#1092,.T.);
#5825=EDGE_CURVE('',#7619,#7620,#1852,.T.);
#5826=EDGE_CURVE('',#7620,#7621,#1853,.T.);
#5827=EDGE_CURVE('',#7621,#7622,#1854,.T.);
#5828=EDGE_CURVE('',#7622,#7623,#1855,.T.);
#5829=EDGE_CURVE('',#7623,#7618,#431,.T.);
#5830=EDGE_CURVE('',#7624,#7625,#1856,.T.);
#5831=EDGE_CURVE('',#7624,#7617,#1093,.T.);
#5832=EDGE_CURVE('',#7618,#7625,#8817,.T.);
#5833=EDGE_CURVE('',#7626,#7627,#1857,.T.);
#5834=EDGE_CURVE('',#7626,#7624,#1094,.T.);
#5835=EDGE_CURVE('',#7625,#7627,#432,.T.);
#5836=EDGE_CURVE('',#7628,#7629,#1858,.T.);
#5837=EDGE_CURVE('',#7628,#7626,#433,.F.);
#5838=EDGE_CURVE('',#7627,#7629,#8818,.T.);
#5839=EDGE_CURVE('',#7630,#7631,#1859,.T.);
#5840=EDGE_CURVE('',#7630,#7628,#1095,.T.);
#5841=EDGE_CURVE('',#7629,#7631,#434,.T.);
#5842=EDGE_CURVE('',#7632,#7633,#1860,.T.);
#5843=EDGE_CURVE('',#7632,#7630,#1096,.T.);
#5844=EDGE_CURVE('',#7631,#7633,#8819,.T.);
#5845=EDGE_CURVE('',#7634,#7635,#1861,.T.);
#5846=EDGE_CURVE('',#7634,#7632,#1097,.T.);
#5847=EDGE_CURVE('',#7633,#7636,#435,.T.);
#5848=EDGE_CURVE('',#7637,#7636,#1862,.T.);
#5849=EDGE_CURVE('',#7638,#7637,#1863,.T.);
#5850=EDGE_CURVE('',#7639,#7638,#1864,.T.);
#5851=EDGE_CURVE('',#7635,#7639,#1865,.T.);
#5852=EDGE_CURVE('',#7636,#7623,#8820,.T.);
#5853=EDGE_CURVE('',#7634,#7619,#436,.T.);
#5854=EDGE_CURVE('',#7640,#7640,#437,.T.);
#5855=EDGE_CURVE('',#7641,#7641,#438,.T.);
#5856=EDGE_CURVE('',#7642,#7642,#439,.T.);
#5857=EDGE_CURVE('',#7643,#7644,#440,.T.);
#5858=EDGE_CURVE('',#7645,#7644,#8821,.T.);
#5859=EDGE_CURVE('',#7645,#7646,#1098,.F.);
#5860=EDGE_CURVE('',#7643,#7646,#8822,.T.);
#5861=EDGE_CURVE('',#7647,#7648,#441,.T.);
#5862=EDGE_CURVE('',#7646,#7648,#442,.T.);
#5863=EDGE_CURVE('',#7647,#7645,#443,.T.);
#5864=EDGE_CURVE('',#7649,#7650,#444,.T.);
#5865=EDGE_CURVE('',#7650,#7644,#445,.T.);
#5866=EDGE_CURVE('',#7643,#7649,#446,.T.);
#5867=EDGE_CURVE('',#7651,#7652,#447,.T.);
#5868=EDGE_CURVE('',#7652,#7648,#448,.T.);
#5869=EDGE_CURVE('',#7647,#7651,#449,.T.);
#5870=EDGE_CURVE('',#7653,#7654,#450,.T.);
#5871=EDGE_CURVE('',#7649,#7654,#8823,.T.);
#5872=EDGE_CURVE('',#7653,#7643,#8824,.T.);
#5873=EDGE_CURVE('',#7655,#7656,#451,.T.);
#5874=EDGE_CURVE('',#7652,#7656,#8825,.T.);
#5875=EDGE_CURVE('',#7655,#7651,#8826,.T.);
#5876=EDGE_CURVE('',#7657,#7658,#452,.T.);
#5877=EDGE_CURVE('',#7648,#7658,#8827,.T.);
#5878=EDGE_CURVE('',#7657,#7652,#8828,.T.);
#5879=EDGE_CURVE('',#7659,#7660,#453,.T.);
#5880=EDGE_CURVE('',#7660,#7654,#454,.T.);
#5881=EDGE_CURVE('',#7653,#7659,#455,.T.);
#5882=EDGE_CURVE('',#7661,#7662,#456,.T.);
#5883=EDGE_CURVE('',#7662,#7663,#457,.T.);
#5884=EDGE_CURVE('',#7664,#7663,#458,.T.);
#5885=EDGE_CURVE('',#7664,#7661,#459,.T.);
#5886=EDGE_CURVE('',#7665,#7666,#460,.T.);
#5887=EDGE_CURVE('',#7666,#7656,#461,.T.);
#5888=EDGE_CURVE('',#7655,#7665,#462,.T.);
#5889=EDGE_CURVE('',#7667,#7668,#463,.T.);
#5890=EDGE_CURVE('',#7668,#7658,#464,.T.);
#5891=EDGE_CURVE('',#7657,#7667,#465,.T.);
#5892=EDGE_CURVE('',#7669,#7670,#1099,.T.);
#5893=EDGE_CURVE('',#7659,#7670,#8829,.T.);
#5894=EDGE_CURVE('',#7669,#7653,#8830,.T.);
#5895=EDGE_CURVE('',#7671,#7672,#466,.T.);
#5896=EDGE_CURVE('',#7661,#7672,#8831,.T.);
#5897=EDGE_CURVE('',#7671,#7664,#8832,.T.);
#5898=EDGE_CURVE('',#7673,#7674,#467,.T.);
#5899=EDGE_CURVE('',#7662,#7674,#8833,.T.);
#5900=EDGE_CURVE('',#7673,#7661,#8834,.T.);
#5901=EDGE_CURVE('',#7675,#7676,#468,.T.);
#5902=EDGE_CURVE('',#7666,#7676,#469,.T.);
#5903=EDGE_CURVE('',#7675,#7665,#470,.T.);
#5904=EDGE_CURVE('',#7677,#7678,#471,.T.);
#5905=EDGE_CURVE('',#7656,#7678,#8835,.T.);
#5906=EDGE_CURVE('',#7677,#7666,#8836,.T.);
#5907=EDGE_CURVE('',#7678,#7679,#472,.T.);
#5908=EDGE_CURVE('',#7667,#7679,#8837,.T.);
#5909=EDGE_CURVE('',#7678,#7657,#8838,.T.);
#5910=EDGE_CURVE('',#7670,#7668,#473,.T.);
#5911=EDGE_CURVE('',#7658,#7669,#474,.T.);
#5912=EDGE_CURVE('',#7680,#7681,#475,.T.);
#5913=EDGE_CURVE('',#7681,#7672,#476,.T.);
#5914=EDGE_CURVE('',#7680,#7671,#477,.T.);
#5915=EDGE_CURVE('',#7682,#7683,#478,.T.);
#5916=EDGE_CURVE('',#7683,#7674,#479,.T.);
#5917=EDGE_CURVE('',#7673,#7682,#480,.T.);
#5918=EDGE_CURVE('',#7684,#7685,#481,.T.);
#5919=EDGE_CURVE('',#7685,#7676,#482,.T.);
#5920=EDGE_CURVE('',#7675,#7684,#483,.T.);
#5921=EDGE_CURVE('',#7677,#7686,#484,.T.);
#5922=EDGE_CURVE('',#7686,#7679,#485,.T.);
#5923=EDGE_CURVE('',#7687,#7688,#486,.T.);
#5924=EDGE_CURVE('',#7672,#7688,#8839,.T.);
#5925=EDGE_CURVE('',#7687,#7681,#8840,.T.);
#5926=EDGE_CURVE('',#7688,#7689,#487,.T.);
#5927=EDGE_CURVE('',#7682,#7689,#8841,.T.);
#5928=EDGE_CURVE('',#7688,#7673,#8842,.T.);
#5929=EDGE_CURVE('',#7690,#7691,#488,.T.);
#5930=EDGE_CURVE('',#7683,#7691,#489,.T.);
#5931=EDGE_CURVE('',#7690,#7682,#490,.T.);
#5932=EDGE_CURVE('',#7692,#7693,#491,.T.);
#5933=EDGE_CURVE('',#7685,#7693,#8843,.T.);
#5934=EDGE_CURVE('',#7692,#7684,#8844,.T.);
#5935=EDGE_CURVE('',#7694,#7695,#492,.T.);
#5936=EDGE_CURVE('',#7676,#7695,#8845,.T.);
#5937=EDGE_CURVE('',#7694,#7685,#8846,.T.);
#5938=EDGE_CURVE('',#7695,#7696,#493,.T.);
#5939=EDGE_CURVE('',#7686,#7696,#494,.T.);
#5940=EDGE_CURVE('',#7695,#7677,#495,.T.);
#5941=EDGE_CURVE('',#7687,#7697,#496,.T.);
#5942=EDGE_CURVE('',#7697,#7689,#497,.T.);
#5943=EDGE_CURVE('',#7698,#7699,#498,.T.);
#5944=EDGE_CURVE('',#7699,#7691,#499,.T.);
#5945=EDGE_CURVE('',#7690,#7698,#500,.T.);
#5946=EDGE_CURVE('',#7700,#7701,#501,.T.);
#5947=EDGE_CURVE('',#7701,#7693,#502,.T.);
#5948=EDGE_CURVE('',#7692,#7700,#503,.T.);
#5949=EDGE_CURVE('',#7694,#7702,#504,.T.);
#5950=EDGE_CURVE('',#7702,#7696,#505,.T.);
#5951=EDGE_CURVE('',#7703,#7704,#506,.T.);
#5952=EDGE_CURVE('',#7689,#7704,#507,.T.);
#5953=EDGE_CURVE('',#7703,#7697,#508,.T.);
#5954=EDGE_CURVE('',#7704,#7705,#509,.T.);
#5955=EDGE_CURVE('',#7698,#7705,#8847,.T.);
#5956=EDGE_CURVE('',#7704,#7690,#8848,.T.);
#5957=EDGE_CURVE('',#7706,#7707,#510,.T.);
#5958=EDGE_CURVE('',#7699,#7707,#8849,.T.);
#5959=EDGE_CURVE('',#7706,#7698,#8850,.T.);
#5960=EDGE_CURVE('',#7708,#7709,#511,.T.);
#5961=EDGE_CURVE('',#7701,#7709,#512,.T.);
#5962=EDGE_CURVE('',#7708,#7700,#513,.T.);
#5963=EDGE_CURVE('',#7710,#7711,#514,.T.);
#5964=EDGE_CURVE('',#7693,#7711,#8851,.T.);
#5965=EDGE_CURVE('',#7710,#7701,#8852,.T.);
#5966=EDGE_CURVE('',#7711,#7712,#515,.T.);
#5967=EDGE_CURVE('',#7702,#7712,#8853,.T.);
#5968=EDGE_CURVE('',#7711,#7694,#8854,.T.);
#5969=EDGE_CURVE('',#7703,#7713,#516,.T.);
#5970=EDGE_CURVE('',#7713,#7705,#517,.T.);
#5971=EDGE_CURVE('',#7714,#7715,#518,.T.);
#5972=EDGE_CURVE('',#7715,#7707,#519,.T.);
#5973=EDGE_CURVE('',#7706,#7714,#520,.T.);
#5974=EDGE_CURVE('',#7716,#7717,#521,.T.);
#5975=EDGE_CURVE('',#7717,#7709,#522,.T.);
#5976=EDGE_CURVE('',#7708,#7716,#523,.T.);
#5977=EDGE_CURVE('',#7710,#7718,#524,.T.);
#5978=EDGE_CURVE('',#7718,#7712,#525,.T.);
#5979=EDGE_CURVE('',#7719,#7720,#526,.T.);
#5980=EDGE_CURVE('',#7705,#7720,#8855,.T.);
#5981=EDGE_CURVE('',#7719,#7713,#8856,.T.);
#5982=EDGE_CURVE('',#7720,#7721,#527,.T.);
#5983=EDGE_CURVE('',#7714,#7721,#8857,.T.);
#5984=EDGE_CURVE('',#7720,#7706,#8858,.T.);
#5985=EDGE_CURVE('',#7722,#7723,#528,.T.);
#5986=EDGE_CURVE('',#7715,#7723,#529,.T.);
#5987=EDGE_CURVE('',#7722,#7714,#530,.T.);
#5988=EDGE_CURVE('',#7724,#7725,#531,.T.);
#5989=EDGE_CURVE('',#7717,#7725,#8859,.T.);
#5990=EDGE_CURVE('',#7724,#7716,#8860,.T.);
#5991=EDGE_CURVE('',#7726,#7727,#532,.T.);
#5992=EDGE_CURVE('',#7709,#7727,#8861,.T.);
#5993=EDGE_CURVE('',#7726,#7717,#8862,.T.);
#5994=EDGE_CURVE('',#7727,#7728,#533,.T.);
#5995=EDGE_CURVE('',#7718,#7728,#534,.T.);
#5996=EDGE_CURVE('',#7727,#7710,#535,.T.);
#5997=EDGE_CURVE('',#7719,#7729,#536,.T.);
#5998=EDGE_CURVE('',#7729,#7721,#537,.T.);
#5999=EDGE_CURVE('',#7722,#7725,#538,.T.);
#6000=EDGE_CURVE('',#7724,#7723,#539,.T.);
#6001=EDGE_CURVE('',#7726,#7730,#540,.T.);
#6002=EDGE_CURVE('',#7730,#7728,#541,.T.);
#6003=EDGE_CURVE('',#7731,#7732,#542,.T.);
#6004=EDGE_CURVE('',#7721,#7732,#543,.T.);
#6005=EDGE_CURVE('',#7731,#7729,#544,.T.);
#6006=EDGE_CURVE('',#7732,#7733,#545,.T.);
#6007=EDGE_CURVE('',#7725,#7733,#8863,.T.);
#6008=EDGE_CURVE('',#7732,#7722,#8864,.T.);
#6009=EDGE_CURVE('',#7733,#7734,#546,.T.);
#6010=EDGE_CURVE('',#7730,#7734,#8865,.T.);
#6011=EDGE_CURVE('',#7733,#7726,#8866,.T.);
#6012=EDGE_CURVE('',#7731,#7734,#547,.T.);
#6013=EDGE_CURVE('',#7735,#7735,#548,.T.);
#6014=EDGE_CURVE('',#7736,#7736,#549,.T.);
#6015=EDGE_CURVE('',#7737,#7737,#550,.T.);
#6016=EDGE_CURVE('',#7738,#7738,#551,.T.);
#6017=EDGE_CURVE('',#7739,#7739,#552,.T.);
#6018=EDGE_CURVE('',#7740,#7740,#553,.T.);
#6019=EDGE_CURVE('',#7741,#7742,#8867,.T.);
#6020=EDGE_CURVE('',#7742,#7743,#1866,.T.);
#6021=EDGE_CURVE('',#7743,#7744,#1867,.T.);
#6022=EDGE_CURVE('',#7744,#7745,#1868,.T.);
#6023=EDGE_CURVE('',#7745,#7746,#1869,.T.);
#6024=EDGE_CURVE('',#7746,#7747,#8868,.T.);
#6025=EDGE_CURVE('',#7741,#7747,#1870,.T.);
#6026=EDGE_CURVE('',#7748,#7749,#8869,.T.);
#6027=EDGE_CURVE('',#7749,#7750,#1871,.T.);
#6028=EDGE_CURVE('',#7750,#7751,#8870,.T.);
#6029=EDGE_CURVE('',#7752,#7751,#1872,.T.);
#6030=EDGE_CURVE('',#7753,#7752,#1873,.T.);
#6031=EDGE_CURVE('',#7754,#7753,#1874,.T.);
#6032=EDGE_CURVE('',#7748,#7754,#1875,.T.);
#6033=EDGE_CURVE('',#7749,#7741,#8871,.T.);
#6034=EDGE_CURVE('',#7747,#7750,#8872,.T.);
#6035=EDGE_CURVE('',#7751,#7746,#8873,.T.);
#6036=EDGE_CURVE('',#7742,#7748,#8874,.T.);
#6037=EDGE_CURVE('',#7755,#7755,#554,.T.);
#6038=EDGE_CURVE('',#7756,#7756,#555,.T.);
#6039=EDGE_CURVE('',#7757,#7757,#556,.T.);
#6040=EDGE_CURVE('',#7758,#7758,#557,.T.);
#6041=EDGE_CURVE('',#7759,#7759,#558,.T.);
#6042=EDGE_CURVE('',#7650,#7663,#559,.T.);
#6043=EDGE_CURVE('',#7760,#7760,#560,.T.);
#6044=EDGE_CURVE('',#7664,#7649,#561,.T.);
#6045=EDGE_CURVE('',#7654,#7671,#562,.T.);
#6046=EDGE_CURVE('',#7646,#7669,#8875,.T.);
#6047=EDGE_CURVE('',#7680,#7660,#563,.T.);
#6048=EDGE_CURVE('',#7761,#7761,#564,.T.);
#6049=EDGE_CURVE('',#7762,#7762,#565,.T.);
#6050=EDGE_CURVE('',#7763,#7763,#566,.T.);
#6051=EDGE_CURVE('',#7748,#7748,#567,.T.);
#6052=EDGE_CURVE('',#7764,#7764,#568,.T.);
#6053=EDGE_CURVE('',#7765,#7766,#569,.T.);
#6054=EDGE_CURVE('',#7766,#7767,#8876,.T.);
#6055=EDGE_CURVE('',#7768,#7767,#8877,.T.);
#6056=EDGE_CURVE('',#7765,#7768,#8878,.T.);
#6057=EDGE_CURVE('',#7767,#7769,#8879,.T.);
#6058=EDGE_CURVE('',#7769,#7766,#570,.T.);
#6059=EDGE_CURVE('',#7770,#7768,#8880,.T.);
#6060=EDGE_CURVE('',#7765,#7770,#571,.T.);
#6061=EDGE_CURVE('',#7771,#7772,#572,.T.);
#6062=EDGE_CURVE('',#7772,#7773,#8881,.T.);
#6063=EDGE_CURVE('',#7774,#7773,#8882,.T.);
#6064=EDGE_CURVE('',#7771,#7774,#8883,.T.);
#6065=EDGE_CURVE('',#7775,#7774,#8884,.T.);
#6066=EDGE_CURVE('',#7771,#7775,#573,.T.);
#6067=EDGE_CURVE('',#7773,#7776,#8885,.T.);
#6068=EDGE_CURVE('',#7776,#7772,#574,.T.);
#6069=EDGE_CURVE('',#7777,#7767,#8886,.T.);
#6070=EDGE_CURVE('',#7777,#7778,#575,.T.);
#6071=EDGE_CURVE('',#7778,#7774,#8887,.T.);
#6072=EDGE_CURVE('',#7767,#7774,#8888,.T.);
#6073=EDGE_CURVE('',#7779,#7780,#576,.T.);
#6074=EDGE_CURVE('',#7780,#7768,#8889,.T.);
#6075=EDGE_CURVE('',#7773,#7768,#8890,.T.);
#6076=EDGE_CURVE('',#7779,#7773,#8891,.T.);
#6077=EDGE_CURVE('',#7781,#7781,#577,.T.);
#6078=EDGE_CURVE('',#7782,#7782,#578,.T.);
#6079=EDGE_CURVE('',#7783,#7783,#579,.T.);
#6080=EDGE_CURVE('',#7775,#7778,#580,.T.);
#6081=EDGE_CURVE('',#7779,#7776,#581,.T.);
#6082=EDGE_CURVE('',#7777,#7769,#582,.T.);
#6083=EDGE_CURVE('',#7770,#7780,#583,.T.);
#6084=EDGE_CURVE('',#7784,#7784,#584,.T.);
#6085=EDGE_CURVE('',#7785,#7785,#585,.T.);
#6086=EDGE_CURVE('',#7786,#7786,#586,.T.);
#6087=EDGE_CURVE('',#7787,#7787,#587,.T.);
#6088=EDGE_CURVE('',#7788,#7788,#588,.T.);
#6089=EDGE_CURVE('',#7789,#7789,#589,.T.);
#6090=EDGE_CURVE('',#7791,#7791,#590,.T.);
#6091=EDGE_CURVE('',#7793,#7793,#591,.T.);
#6092=EDGE_CURVE('',#7794,#7794,#592,.T.);
#6093=EDGE_CURVE('',#7795,#7795,#593,.T.);
#6094=EDGE_CURVE('',#7796,#7796,#594,.T.);
#6095=EDGE_CURVE('',#7797,#7797,#595,.T.);
#6096=EDGE_CURVE('',#7798,#7798,#596,.T.);
#6097=EDGE_CURVE('',#7799,#7799,#597,.T.);
#6098=EDGE_CURVE('',#7800,#7800,#598,.T.);
#6099=EDGE_CURVE('',#7801,#7801,#599,.T.);
#6100=EDGE_CURVE('',#7802,#7802,#600,.T.);
#6101=EDGE_CURVE('',#7803,#7803,#601,.T.);
#6102=EDGE_CURVE('',#7804,#7805,#602,.T.);
#6103=EDGE_CURVE('',#7805,#7806,#1876,.T.);
#6104=EDGE_CURVE('',#7806,#7807,#603,.T.);
#6105=EDGE_CURVE('',#7808,#7807,#1877,.T.);
#6106=EDGE_CURVE('',#7809,#7808,#1878,.T.);
#6107=EDGE_CURVE('',#7810,#7809,#1879,.T.);
#6108=EDGE_CURVE('',#7811,#7810,#1880,.T.);
#6109=EDGE_CURVE('',#7804,#7811,#1881,.T.);
#6110=EDGE_CURVE('',#7812,#7813,#1882,.T.);
#6111=EDGE_CURVE('',#7813,#7814,#1100,.T.);
#6112=EDGE_CURVE('',#7814,#7806,#8892,.T.);
#6113=EDGE_CURVE('',#7805,#7812,#8893,.T.);
#6114=EDGE_CURVE('',#7815,#7816,#1883,.T.);
#6115=EDGE_CURVE('',#7816,#7813,#1101,.T.);
#6116=EDGE_CURVE('',#7812,#7815,#604,.T.);
#6117=EDGE_CURVE('',#7817,#7818,#1884,.T.);
#6118=EDGE_CURVE('',#7818,#7816,#605,.F.);
#6119=EDGE_CURVE('',#7815,#7817,#8894,.T.);
#6120=EDGE_CURVE('',#7819,#7820,#606,.T.);
#6121=EDGE_CURVE('',#7821,#7819,#8895,.T.);
#6122=EDGE_CURVE('',#7817,#7821,#607,.T.);
#6123=EDGE_CURVE('',#7820,#7804,#8896,.T.);
#6124=EDGE_CURVE('',#7822,#7823,#8897,.T.);
#6125=EDGE_CURVE('',#7823,#7824,#608,.T.);
#6126=EDGE_CURVE('',#7825,#7824,#1885,.T.);
#6127=EDGE_CURVE('',#7825,#7822,#609,.T.);
#6128=EDGE_CURVE('',#7821,#7826,#1886,.T.);
#6129=EDGE_CURVE('',#7826,#7818,#1102,.T.);
#6130=EDGE_CURVE('',#7819,#7827,#1887,.T.);
#6131=EDGE_CURVE('',#7827,#7826,#1103,.T.);
#6132=EDGE_CURVE('',#7824,#7827,#1104,.T.);
#6133=EDGE_CURVE('',#7820,#7828,#1888,.T.);
#6134=EDGE_CURVE('',#7828,#7829,#1889,.T.);
#6135=EDGE_CURVE('',#7829,#7830,#1890,.T.);
#6136=EDGE_CURVE('',#7830,#7825,#1891,.T.);
#6137=EDGE_CURVE('',#7814,#7823,#8898,.T.);
#6138=EDGE_CURVE('',#7807,#7822,#8899,.T.);
#6139=EDGE_CURVE('',#7831,#7832,#8900,.T.);
#6140=EDGE_CURVE('',#7831,#7833,#8901,.T.);
#6141=EDGE_CURVE('',#7834,#7833,#1105,.T.);
#6142=EDGE_CURVE('',#7835,#7834,#8902,.T.);
#6143=EDGE_CURVE('',#7832,#7835,#610,.T.);
#6144=EDGE_CURVE('',#7836,#7835,#1892,.T.);
#6145=EDGE_CURVE('',#7836,#7837,#1106,.T.);
#6146=EDGE_CURVE('',#7837,#7832,#1893,.T.);
#6147=EDGE_CURVE('',#7838,#7834,#611,.T.);
#6148=EDGE_CURVE('',#7838,#7836,#1107,.T.);
#6149=EDGE_CURVE('',#7833,#7838,#1108,.T.);
#6150=EDGE_CURVE('',#7837,#7831,#612,.T.);
#6151=EDGE_CURVE('',#7804,#7804,#613,.T.);
#6152=EDGE_CURVE('',#7839,#7839,#614,.T.);
#6153=EDGE_CURVE('',#7840,#7840,#615,.T.);
#6154=EDGE_CURVE('',#7825,#7822,#616,.T.);
#6155=EDGE_CURVE('',#7841,#7841,#617,.T.);
#6156=EDGE_CURVE('',#7842,#7842,#618,.T.);
#6157=EDGE_CURVE('',#7843,#7843,#619,.T.);
#6158=EDGE_CURVE('',#7844,#7844,#620,.T.);
#6159=EDGE_CURVE('',#7845,#7845,#621,.T.);
#6160=EDGE_CURVE('',#7846,#7846,#622,.T.);
#6161=EDGE_CURVE('',#7847,#7847,#623,.T.);
#6162=EDGE_CURVE('',#7848,#7848,#624,.T.);
#6163=EDGE_CURVE('',#7849,#7849,#625,.T.);
#6164=EDGE_CURVE('',#7850,#7850,#626,.T.);
#6165=EDGE_CURVE('',#7851,#7851,#627,.T.);
#6166=EDGE_CURVE('',#7852,#7852,#628,.T.);
#6167=EDGE_CURVE('',#7853,#7853,#629,.T.);
#6168=EDGE_CURVE('',#7854,#7854,#630,.T.);
#6169=EDGE_CURVE('',#7855,#7855,#631,.T.);
#6170=EDGE_CURVE('',#7856,#7856,#632,.T.);
#6171=EDGE_CURVE('',#7857,#7857,#633,.T.);
#6172=EDGE_CURVE('',#7858,#7858,#634,.T.);
#6173=EDGE_CURVE('',#7859,#7859,#635,.T.);
#6174=EDGE_CURVE('',#7860,#7860,#636,.T.);
#6175=EDGE_CURVE('',#7861,#7861,#637,.T.);
#6176=EDGE_CURVE('',#7862,#7862,#638,.T.);
#6177=EDGE_CURVE('',#7863,#7863,#639,.T.);
#6178=EDGE_CURVE('',#7864,#7864,#640,.T.);
#6179=EDGE_CURVE('',#7865,#7865,#641,.T.);
#6180=EDGE_CURVE('',#7866,#7866,#642,.T.);
#6181=EDGE_CURVE('',#7867,#7867,#643,.T.);
#6182=EDGE_CURVE('',#7868,#7868,#644,.T.);
#6183=EDGE_CURVE('',#7869,#7870,#1109,.T.);
#6184=EDGE_CURVE('',#7871,#7869,#1894,.T.);
#6185=EDGE_CURVE('',#7872,#7871,#1895,.T.);
#6186=EDGE_CURVE('',#7873,#7872,#1896,.T.);
#6187=EDGE_CURVE('',#7874,#7873,#1897,.T.);
#6188=EDGE_CURVE('',#7875,#7874,#1898,.T.);
#6189=EDGE_CURVE('',#7876,#7875,#1899,.T.);
#6190=EDGE_CURVE('',#7877,#7876,#1900,.T.);
#6191=EDGE_CURVE('',#7878,#7877,#8903,.T.);
#6192=EDGE_CURVE('',#7878,#7879,#1901,.T.);
#6193=EDGE_CURVE('',#7870,#7879,#8904,.T.);
#6194=EDGE_CURVE('',#7880,#7881,#8905,.T.);
#6195=EDGE_CURVE('',#7880,#7882,#1902,.T.);
#6196=EDGE_CURVE('',#7882,#7883,#1903,.T.);
#6197=EDGE_CURVE('',#7883,#7884,#1904,.T.);
#6198=EDGE_CURVE('',#7884,#7885,#1905,.T.);
#6199=EDGE_CURVE('',#7885,#7886,#1906,.T.);
#6200=EDGE_CURVE('',#7886,#7887,#1907,.T.);
#6201=EDGE_CURVE('',#7887,#7888,#1908,.T.);
#6202=EDGE_CURVE('',#7888,#7889,#1909,.T.);
#6203=EDGE_CURVE('',#7890,#7889,#8906,.T.);
#6204=EDGE_CURVE('',#7881,#7890,#1910,.T.);
#6205=EDGE_CURVE('',#7881,#7878,#8907,.T.);
#6206=EDGE_CURVE('',#7879,#7890,#8908,.T.);
#6207=EDGE_CURVE('',#7870,#7891,#8909,.T.);
#6208=EDGE_CURVE('',#7889,#7891,#8910,.T.);
#6209=EDGE_CURVE('',#7877,#7880,#8911,.T.);
#6210=EDGE_CURVE('',#7880,#7880,#645,.T.);
#6211=EDGE_CURVE('',#7892,#7892,#646,.T.);
#6212=EDGE_CURVE('',#7893,#7894,#8912,.T.);
#6213=EDGE_CURVE('',#7895,#7893,#647,.T.);
#6214=EDGE_CURVE('',#7896,#7895,#8913,.T.);
#6215=EDGE_CURVE('',#7897,#7896,#8914,.T.);
#6216=EDGE_CURVE('',#7898,#7897,#648,.T.);
#6217=EDGE_CURVE('',#7899,#7898,#8915,.T.);
#6218=EDGE_CURVE('',#7900,#7899,#8916,.T.);
#6219=EDGE_CURVE('',#7901,#7900,#649,.T.);
#6220=EDGE_CURVE('',#7902,#7901,#8917,.T.);
#6221=EDGE_CURVE('',#7903,#7902,#8918,.T.);
#6222=EDGE_CURVE('',#7904,#7903,#650,.T.);
#6223=EDGE_CURVE('',#7905,#7904,#8919,.T.);
#6224=EDGE_CURVE('',#7906,#7905,#8920,.T.);
#6225=EDGE_CURVE('',#7907,#7906,#651,.T.);
#6226=EDGE_CURVE('',#7908,#7907,#8921,.T.);
#6227=EDGE_CURVE('',#7909,#7908,#8922,.T.);
#6228=EDGE_CURVE('',#7910,#7909,#652,.T.);
#6229=EDGE_CURVE('',#7911,#7910,#8923,.T.);
#6230=EDGE_CURVE('',#7912,#7911,#8924,.T.);
#6231=EDGE_CURVE('',#7913,#7912,#653,.T.);
#6232=EDGE_CURVE('',#7914,#7913,#8925,.T.);
#6233=EDGE_CURVE('',#7915,#7914,#8926,.T.);
#6234=EDGE_CURVE('',#7916,#7915,#654,.T.);
#6235=EDGE_CURVE('',#7917,#7916,#8927,.T.);
#6236=EDGE_CURVE('',#7918,#7917,#8928,.T.);
#6237=EDGE_CURVE('',#7919,#7918,#655,.T.);
#6238=EDGE_CURVE('',#7920,#7919,#8929,.T.);
#6239=EDGE_CURVE('',#7921,#7920,#8930,.T.);
#6240=EDGE_CURVE('',#7922,#7921,#656,.T.);
#6241=EDGE_CURVE('',#7923,#7922,#8931,.T.);
#6242=EDGE_CURVE('',#7924,#7923,#8932,.T.);
#6243=EDGE_CURVE('',#7925,#7924,#657,.T.);
#6244=EDGE_CURVE('',#7926,#7925,#8933,.T.);
#6245=EDGE_CURVE('',#7927,#7926,#8934,.T.);
#6246=EDGE_CURVE('',#7928,#7927,#658,.T.);
#6247=EDGE_CURVE('',#7929,#7928,#8935,.T.);
#6248=EDGE_CURVE('',#7930,#7929,#8936,.T.);
#6249=EDGE_CURVE('',#7931,#7930,#659,.T.);
#6250=EDGE_CURVE('',#7932,#7931,#8937,.T.);
#6251=EDGE_CURVE('',#7933,#7932,#8938,.T.);
#6252=EDGE_CURVE('',#7934,#7933,#660,.T.);
#6253=EDGE_CURVE('',#7935,#7934,#8939,.T.);
#6254=EDGE_CURVE('',#7936,#7935,#8940,.T.);
#6255=EDGE_CURVE('',#7937,#7936,#661,.T.);
#6256=EDGE_CURVE('',#7938,#7937,#8941,.T.);
#6257=EDGE_CURVE('',#7939,#7938,#8942,.T.);
#6258=EDGE_CURVE('',#7940,#7939,#662,.T.);
#6259=EDGE_CURVE('',#7941,#7940,#8943,.T.);
#6260=EDGE_CURVE('',#7942,#7941,#8944,.T.);
#6261=EDGE_CURVE('',#7943,#7942,#663,.T.);
#6262=EDGE_CURVE('',#7944,#7943,#8945,.T.);
#6263=EDGE_CURVE('',#7945,#7944,#8946,.T.);
#6264=EDGE_CURVE('',#7946,#7945,#664,.T.);
#6265=EDGE_CURVE('',#7947,#7946,#8947,.T.);
#6266=EDGE_CURVE('',#7948,#7947,#8948,.T.);
#6267=EDGE_CURVE('',#7949,#7948,#665,.T.);
#6268=EDGE_CURVE('',#7950,#7949,#8949,.T.);
#6269=EDGE_CURVE('',#7951,#7950,#8950,.T.);
#6270=EDGE_CURVE('',#7952,#7951,#666,.T.);
#6271=EDGE_CURVE('',#7953,#7952,#8951,.T.);
#6272=EDGE_CURVE('',#7954,#7953,#8952,.T.);
#6273=EDGE_CURVE('',#7955,#7954,#667,.T.);
#6274=EDGE_CURVE('',#7956,#7955,#8953,.T.);
#6275=EDGE_CURVE('',#7957,#7956,#8954,.T.);
#6276=EDGE_CURVE('',#7958,#7957,#668,.T.);
#6277=EDGE_CURVE('',#7959,#7958,#8955,.T.);
#6278=EDGE_CURVE('',#7960,#7959,#8956,.T.);
#6279=EDGE_CURVE('',#7961,#7960,#669,.T.);
#6280=EDGE_CURVE('',#7962,#7961,#8957,.T.);
#6281=EDGE_CURVE('',#7963,#7962,#8958,.T.);
#6282=EDGE_CURVE('',#7964,#7963,#670,.T.);
#6283=EDGE_CURVE('',#7965,#7964,#8959,.T.);
#6284=EDGE_CURVE('',#7966,#7965,#8960,.T.);
#6285=EDGE_CURVE('',#7967,#7966,#671,.T.);
#6286=EDGE_CURVE('',#7968,#7967,#8961,.T.);
#6287=EDGE_CURVE('',#7969,#7968,#8962,.T.);
#6288=EDGE_CURVE('',#7970,#7969,#672,.T.);
#6289=EDGE_CURVE('',#7971,#7970,#8963,.T.);
#6290=EDGE_CURVE('',#7972,#7971,#8964,.T.);
#6291=EDGE_CURVE('',#7973,#7972,#673,.T.);
#6292=EDGE_CURVE('',#7974,#7973,#8965,.T.);
#6293=EDGE_CURVE('',#7975,#7974,#8966,.T.);
#6294=EDGE_CURVE('',#7976,#7975,#674,.T.);
#6295=EDGE_CURVE('',#7977,#7976,#8967,.T.);
#6296=EDGE_CURVE('',#7978,#7977,#8968,.T.);
#6297=EDGE_CURVE('',#7979,#7978,#675,.T.);
#6298=EDGE_CURVE('',#7980,#7979,#8969,.T.);
#6299=EDGE_CURVE('',#7981,#7980,#8970,.T.);
#6300=EDGE_CURVE('',#7982,#7981,#676,.T.);
#6301=EDGE_CURVE('',#7983,#7982,#8971,.T.);
#6302=EDGE_CURVE('',#7984,#7983,#8972,.T.);
#6303=EDGE_CURVE('',#7985,#7984,#677,.T.);
#6304=EDGE_CURVE('',#7986,#7985,#8973,.T.);
#6305=EDGE_CURVE('',#7987,#7986,#8974,.T.);
#6306=EDGE_CURVE('',#7988,#7987,#678,.T.);
#6307=EDGE_CURVE('',#7989,#7988,#8975,.T.);
#6308=EDGE_CURVE('',#7990,#7989,#8976,.T.);
#6309=EDGE_CURVE('',#7991,#7990,#679,.T.);
#6310=EDGE_CURVE('',#7992,#7991,#8977,.T.);
#6311=EDGE_CURVE('',#7993,#7992,#8978,.T.);
#6312=EDGE_CURVE('',#7994,#7993,#680,.T.);
#6313=EDGE_CURVE('',#7995,#7994,#8979,.T.);
#6314=EDGE_CURVE('',#7996,#7995,#8980,.T.);
#6315=EDGE_CURVE('',#7997,#7996,#681,.T.);
#6316=EDGE_CURVE('',#7998,#7997,#8981,.T.);
#6317=EDGE_CURVE('',#7999,#7998,#8982,.T.);
#6318=EDGE_CURVE('',#8000,#7999,#682,.T.);
#6319=EDGE_CURVE('',#8001,#8000,#8983,.T.);
#6320=EDGE_CURVE('',#8002,#8001,#8984,.T.);
#6321=EDGE_CURVE('',#8003,#8002,#683,.T.);
#6322=EDGE_CURVE('',#8004,#8003,#8985,.T.);
#6323=EDGE_CURVE('',#8005,#8004,#8986,.T.);
#6324=EDGE_CURVE('',#8006,#8005,#684,.T.);
#6325=EDGE_CURVE('',#8007,#8006,#8987,.T.);
#6326=EDGE_CURVE('',#8008,#8007,#8988,.T.);
#6327=EDGE_CURVE('',#8009,#8008,#685,.T.);
#6328=EDGE_CURVE('',#8010,#8009,#8989,.T.);
#6329=EDGE_CURVE('',#8011,#8010,#8990,.T.);
#6330=EDGE_CURVE('',#8012,#8011,#686,.T.);
#6331=EDGE_CURVE('',#8013,#8012,#8991,.T.);
#6332=EDGE_CURVE('',#8014,#8013,#8992,.T.);
#6333=EDGE_CURVE('',#8015,#8014,#687,.T.);
#6334=EDGE_CURVE('',#8016,#8015,#8993,.T.);
#6335=EDGE_CURVE('',#8017,#8016,#8994,.T.);
#6336=EDGE_CURVE('',#8018,#8017,#688,.T.);
#6337=EDGE_CURVE('',#8019,#8018,#8995,.T.);
#6338=EDGE_CURVE('',#8020,#8019,#8996,.T.);
#6339=EDGE_CURVE('',#8021,#8020,#689,.T.);
#6340=EDGE_CURVE('',#8022,#8021,#8997,.T.);
#6341=EDGE_CURVE('',#8023,#8022,#8998,.T.);
#6342=EDGE_CURVE('',#8024,#8023,#8999,.T.);
#6343=EDGE_CURVE('',#8025,#8024,#9000,.T.);
#6344=EDGE_CURVE('',#8026,#8025,#690,.T.);
#6345=EDGE_CURVE('',#8027,#8026,#9001,.T.);
#6346=EDGE_CURVE('',#8028,#8027,#9002,.T.);
#6347=EDGE_CURVE('',#8029,#8028,#691,.T.);
#6348=EDGE_CURVE('',#8030,#8029,#9003,.T.);
#6349=EDGE_CURVE('',#8031,#8030,#9004,.T.);
#6350=EDGE_CURVE('',#8032,#8031,#692,.T.);
#6351=EDGE_CURVE('',#8033,#8032,#9005,.T.);
#6352=EDGE_CURVE('',#8034,#8033,#9006,.T.);
#6353=EDGE_CURVE('',#8035,#8034,#693,.T.);
#6354=EDGE_CURVE('',#7894,#8035,#9007,.T.);
#6355=EDGE_CURVE('',#8036,#8036,#694,.T.);
#6356=EDGE_CURVE('',#8037,#8038,#9008,.T.);
#6357=EDGE_CURVE('',#8038,#8039,#9009,.T.);
#6358=EDGE_CURVE('',#8039,#8040,#695,.T.);
#6359=EDGE_CURVE('',#8040,#8041,#9010,.T.);
#6360=EDGE_CURVE('',#8041,#8042,#9011,.T.);
#6361=EDGE_CURVE('',#8042,#8043,#696,.T.);
#6362=EDGE_CURVE('',#8043,#8044,#9012,.T.);
#6363=EDGE_CURVE('',#8044,#8045,#9013,.T.);
#6364=EDGE_CURVE('',#8045,#8046,#697,.T.);
#6365=EDGE_CURVE('',#8046,#8047,#9014,.T.);
#6366=EDGE_CURVE('',#8047,#8048,#9015,.T.);
#6367=EDGE_CURVE('',#8048,#8049,#698,.T.);
#6368=EDGE_CURVE('',#8049,#8050,#9016,.T.);
#6369=EDGE_CURVE('',#8050,#8051,#9017,.T.);
#6370=EDGE_CURVE('',#8051,#8052,#9018,.T.);
#6371=EDGE_CURVE('',#8052,#8053,#9019,.T.);
#6372=EDGE_CURVE('',#8053,#8054,#699,.T.);
#6373=EDGE_CURVE('',#8054,#8055,#9020,.T.);
#6374=EDGE_CURVE('',#8055,#8056,#9021,.T.);
#6375=EDGE_CURVE('',#8056,#8057,#700,.T.);
#6376=EDGE_CURVE('',#8057,#8058,#9022,.T.);
#6377=EDGE_CURVE('',#8058,#8059,#9023,.T.);
#6378=EDGE_CURVE('',#8059,#8060,#701,.T.);
#6379=EDGE_CURVE('',#8060,#8061,#9024,.T.);
#6380=EDGE_CURVE('',#8061,#8062,#9025,.T.);
#6381=EDGE_CURVE('',#8062,#8063,#702,.T.);
#6382=EDGE_CURVE('',#8063,#8064,#9026,.T.);
#6383=EDGE_CURVE('',#8064,#8065,#9027,.T.);
#6384=EDGE_CURVE('',#8065,#8066,#703,.T.);
#6385=EDGE_CURVE('',#8066,#8067,#9028,.T.);
#6386=EDGE_CURVE('',#8067,#8068,#9029,.T.);
#6387=EDGE_CURVE('',#8068,#8069,#704,.T.);
#6388=EDGE_CURVE('',#8069,#8070,#9030,.T.);
#6389=EDGE_CURVE('',#8070,#8071,#9031,.T.);
#6390=EDGE_CURVE('',#8071,#8072,#705,.T.);
#6391=EDGE_CURVE('',#8072,#8073,#9032,.T.);
#6392=EDGE_CURVE('',#8073,#8074,#9033,.T.);
#6393=EDGE_CURVE('',#8074,#8075,#706,.T.);
#6394=EDGE_CURVE('',#8075,#8076,#9034,.T.);
#6395=EDGE_CURVE('',#8076,#8077,#9035,.T.);
#6396=EDGE_CURVE('',#8077,#8078,#707,.T.);
#6397=EDGE_CURVE('',#8078,#8079,#9036,.T.);
#6398=EDGE_CURVE('',#8079,#8080,#9037,.T.);
#6399=EDGE_CURVE('',#8080,#8081,#708,.T.);
#6400=EDGE_CURVE('',#8081,#8082,#9038,.T.);
#6401=EDGE_CURVE('',#8082,#8083,#9039,.T.);
#6402=EDGE_CURVE('',#8083,#8084,#709,.T.);
#6403=EDGE_CURVE('',#8084,#8085,#9040,.T.);
#6404=EDGE_CURVE('',#8085,#8086,#9041,.T.);
#6405=EDGE_CURVE('',#8086,#8087,#710,.T.);
#6406=EDGE_CURVE('',#8087,#8088,#9042,.T.);
#6407=EDGE_CURVE('',#8088,#8089,#9043,.T.);
#6408=EDGE_CURVE('',#8089,#8090,#711,.T.);
#6409=EDGE_CURVE('',#8090,#8091,#9044,.T.);
#6410=EDGE_CURVE('',#8091,#8092,#9045,.T.);
#6411=EDGE_CURVE('',#8092,#8093,#712,.T.);
#6412=EDGE_CURVE('',#8093,#8094,#9046,.T.);
#6413=EDGE_CURVE('',#8094,#8095,#9047,.T.);
#6414=EDGE_CURVE('',#8095,#8096,#713,.T.);
#6415=EDGE_CURVE('',#8096,#8097,#9048,.T.);
#6416=EDGE_CURVE('',#8097,#8098,#9049,.T.);
#6417=EDGE_CURVE('',#8098,#8099,#714,.T.);
#6418=EDGE_CURVE('',#8099,#8100,#9050,.T.);
#6419=EDGE_CURVE('',#8100,#8101,#9051,.T.);
#6420=EDGE_CURVE('',#8101,#8102,#715,.T.);
#6421=EDGE_CURVE('',#8102,#8103,#9052,.T.);
#6422=EDGE_CURVE('',#8103,#8104,#9053,.T.);
#6423=EDGE_CURVE('',#8104,#8105,#716,.T.);
#6424=EDGE_CURVE('',#8105,#8106,#9054,.T.);
#6425=EDGE_CURVE('',#8106,#8107,#9055,.T.);
#6426=EDGE_CURVE('',#8107,#8108,#717,.T.);
#6427=EDGE_CURVE('',#8108,#8109,#9056,.T.);
#6428=EDGE_CURVE('',#8109,#8110,#9057,.T.);
#6429=EDGE_CURVE('',#8110,#8111,#718,.T.);
#6430=EDGE_CURVE('',#8111,#8112,#9058,.T.);
#6431=EDGE_CURVE('',#8112,#8113,#9059,.T.);
#6432=EDGE_CURVE('',#8113,#8114,#719,.T.);
#6433=EDGE_CURVE('',#8114,#8115,#9060,.T.);
#6434=EDGE_CURVE('',#8115,#8116,#9061,.T.);
#6435=EDGE_CURVE('',#8116,#8117,#720,.T.);
#6436=EDGE_CURVE('',#8117,#8118,#9062,.T.);
#6437=EDGE_CURVE('',#8118,#8119,#9063,.T.);
#6438=EDGE_CURVE('',#8119,#8120,#721,.T.);
#6439=EDGE_CURVE('',#8120,#8121,#9064,.T.);
#6440=EDGE_CURVE('',#8121,#8122,#9065,.T.);
#6441=EDGE_CURVE('',#8122,#8123,#722,.T.);
#6442=EDGE_CURVE('',#8123,#8124,#9066,.T.);
#6443=EDGE_CURVE('',#8124,#8125,#9067,.T.);
#6444=EDGE_CURVE('',#8125,#8126,#723,.T.);
#6445=EDGE_CURVE('',#8126,#8127,#9068,.T.);
#6446=EDGE_CURVE('',#8127,#8128,#9069,.T.);
#6447=EDGE_CURVE('',#8128,#8129,#724,.T.);
#6448=EDGE_CURVE('',#8129,#8130,#9070,.T.);
#6449=EDGE_CURVE('',#8130,#8131,#9071,.T.);
#6450=EDGE_CURVE('',#8131,#8132,#725,.T.);
#6451=EDGE_CURVE('',#8132,#8133,#9072,.T.);
#6452=EDGE_CURVE('',#8133,#8134,#9073,.T.);
#6453=EDGE_CURVE('',#8134,#8135,#726,.T.);
#6454=EDGE_CURVE('',#8135,#8136,#9074,.T.);
#6455=EDGE_CURVE('',#8136,#8137,#9075,.T.);
#6456=EDGE_CURVE('',#8137,#8138,#727,.T.);
#6457=EDGE_CURVE('',#8138,#8139,#9076,.T.);
#6458=EDGE_CURVE('',#8139,#8140,#9077,.T.);
#6459=EDGE_CURVE('',#8140,#8141,#728,.T.);
#6460=EDGE_CURVE('',#8141,#8142,#9078,.T.);
#6461=EDGE_CURVE('',#8142,#8143,#9079,.T.);
#6462=EDGE_CURVE('',#8143,#8144,#729,.T.);
#6463=EDGE_CURVE('',#8144,#8145,#9080,.T.);
#6464=EDGE_CURVE('',#8145,#8146,#9081,.T.);
#6465=EDGE_CURVE('',#8146,#8147,#730,.T.);
#6466=EDGE_CURVE('',#8147,#8148,#9082,.T.);
#6467=EDGE_CURVE('',#8148,#8149,#9083,.T.);
#6468=EDGE_CURVE('',#8149,#8150,#731,.T.);
#6469=EDGE_CURVE('',#8150,#8151,#9084,.T.);
#6470=EDGE_CURVE('',#8151,#8152,#9085,.T.);
#6471=EDGE_CURVE('',#8152,#8153,#732,.T.);
#6472=EDGE_CURVE('',#8153,#8154,#9086,.T.);
#6473=EDGE_CURVE('',#8154,#8155,#9087,.T.);
#6474=EDGE_CURVE('',#8155,#8156,#733,.T.);
#6475=EDGE_CURVE('',#8156,#8157,#9088,.T.);
#6476=EDGE_CURVE('',#8157,#8158,#9089,.T.);
#6477=EDGE_CURVE('',#8158,#8159,#734,.T.);
#6478=EDGE_CURVE('',#8159,#8160,#9090,.T.);
#6479=EDGE_CURVE('',#8160,#8161,#9091,.T.);
#6480=EDGE_CURVE('',#8161,#8162,#735,.T.);
#6481=EDGE_CURVE('',#8162,#8163,#9092,.T.);
#6482=EDGE_CURVE('',#8163,#8164,#9093,.T.);
#6483=EDGE_CURVE('',#8164,#8165,#736,.T.);
#6484=EDGE_CURVE('',#8165,#8166,#9094,.T.);
#6485=EDGE_CURVE('',#8166,#8167,#9095,.T.);
#6486=EDGE_CURVE('',#8167,#8168,#737,.T.);
#6487=EDGE_CURVE('',#8168,#8169,#9096,.T.);
#6488=EDGE_CURVE('',#8169,#8170,#9097,.T.);
#6489=EDGE_CURVE('',#8170,#8171,#738,.T.);
#6490=EDGE_CURVE('',#8171,#8172,#9098,.T.);
#6491=EDGE_CURVE('',#8172,#8173,#9099,.T.);
#6492=EDGE_CURVE('',#8173,#8174,#739,.T.);
#6493=EDGE_CURVE('',#8174,#8175,#9100,.T.);
#6494=EDGE_CURVE('',#8175,#8176,#9101,.T.);
#6495=EDGE_CURVE('',#8176,#8177,#740,.T.);
#6496=EDGE_CURVE('',#8177,#8178,#9102,.T.);
#6497=EDGE_CURVE('',#8178,#8179,#9103,.T.);
#6498=EDGE_CURVE('',#8179,#8037,#741,.T.);
#6499=EDGE_CURVE('',#8180,#8180,#742,.T.);
#6500=EDGE_CURVE('',#8037,#7893,#9104,.T.);
#6501=EDGE_CURVE('',#8179,#7895,#9105,.T.);
#6502=EDGE_CURVE('',#8178,#7896,#9106,.T.);
#6503=EDGE_CURVE('',#8177,#7897,#9107,.T.);
#6504=EDGE_CURVE('',#8176,#7898,#9108,.T.);
#6505=EDGE_CURVE('',#8175,#7899,#9109,.T.);
#6506=EDGE_CURVE('',#8174,#7900,#9110,.T.);
#6507=EDGE_CURVE('',#8173,#7901,#9111,.T.);
#6508=EDGE_CURVE('',#8172,#7902,#9112,.T.);
#6509=EDGE_CURVE('',#8171,#7903,#9113,.T.);
#6510=EDGE_CURVE('',#8170,#7904,#9114,.T.);
#6511=EDGE_CURVE('',#8169,#7905,#9115,.T.);
#6512=EDGE_CURVE('',#8168,#7906,#9116,.T.);
#6513=EDGE_CURVE('',#8167,#7907,#9117,.T.);
#6514=EDGE_CURVE('',#8166,#7908,#9118,.T.);
#6515=EDGE_CURVE('',#8165,#7909,#9119,.T.);
#6516=EDGE_CURVE('',#8164,#7910,#9120,.T.);
#6517=EDGE_CURVE('',#8163,#7911,#9121,.T.);
#6518=EDGE_CURVE('',#8162,#7912,#9122,.T.);
#6519=EDGE_CURVE('',#8161,#7913,#9123,.T.);
#6520=EDGE_CURVE('',#8160,#7914,#9124,.T.);
#6521=EDGE_CURVE('',#8159,#7915,#9125,.T.);
#6522=EDGE_CURVE('',#8158,#7916,#9126,.T.);
#6523=EDGE_CURVE('',#8157,#7917,#9127,.T.);
#6524=EDGE_CURVE('',#8156,#7918,#9128,.T.);
#6525=EDGE_CURVE('',#8155,#7919,#9129,.T.);
#6526=EDGE_CURVE('',#8154,#7920,#9130,.T.);
#6527=EDGE_CURVE('',#8153,#7921,#9131,.T.);
#6528=EDGE_CURVE('',#8152,#7922,#9132,.T.);
#6529=EDGE_CURVE('',#8151,#7923,#9133,.T.);
#6530=EDGE_CURVE('',#8150,#7924,#9134,.T.);
#6531=EDGE_CURVE('',#8149,#7925,#9135,.T.);
#6532=EDGE_CURVE('',#8148,#7926,#9136,.T.);
#6533=EDGE_CURVE('',#8147,#7927,#9137,.T.);
#6534=EDGE_CURVE('',#8146,#7928,#9138,.T.);
#6535=EDGE_CURVE('',#8145,#7929,#9139,.T.);
#6536=EDGE_CURVE('',#8144,#7930,#9140,.T.);
#6537=EDGE_CURVE('',#8143,#7931,#9141,.T.);
#6538=EDGE_CURVE('',#8142,#7932,#9142,.T.);
#6539=EDGE_CURVE('',#8141,#7933,#9143,.T.);
#6540=EDGE_CURVE('',#8140,#7934,#9144,.T.);
#6541=EDGE_CURVE('',#8139,#7935,#9145,.T.);
#6542=EDGE_CURVE('',#8138,#7936,#9146,.T.);
#6543=EDGE_CURVE('',#8137,#7937,#9147,.T.);
#6544=EDGE_CURVE('',#8136,#7938,#9148,.T.);
#6545=EDGE_CURVE('',#8135,#7939,#9149,.T.);
#6546=EDGE_CURVE('',#8134,#7940,#9150,.T.);
#6547=EDGE_CURVE('',#8133,#7941,#9151,.T.);
#6548=EDGE_CURVE('',#8132,#7942,#9152,.T.);
#6549=EDGE_CURVE('',#8131,#7943,#9153,.T.);
#6550=EDGE_CURVE('',#8130,#7944,#9154,.T.);
#6551=EDGE_CURVE('',#8129,#7945,#9155,.T.);
#6552=EDGE_CURVE('',#8128,#7946,#9156,.T.);
#6553=EDGE_CURVE('',#8127,#7947,#9157,.T.);
#6554=EDGE_CURVE('',#8126,#7948,#9158,.T.);
#6555=EDGE_CURVE('',#8125,#7949,#9159,.T.);
#6556=EDGE_CURVE('',#8124,#7950,#9160,.T.);
#6557=EDGE_CURVE('',#8123,#7951,#9161,.T.);
#6558=EDGE_CURVE('',#8122,#7952,#9162,.T.);
#6559=EDGE_CURVE('',#8121,#7953,#9163,.T.);
#6560=EDGE_CURVE('',#8120,#7954,#9164,.T.);
#6561=EDGE_CURVE('',#8119,#7955,#9165,.T.);
#6562=EDGE_CURVE('',#8118,#7956,#9166,.T.);
#6563=EDGE_CURVE('',#8117,#7957,#9167,.T.);
#6564=EDGE_CURVE('',#8116,#7958,#9168,.T.);
#6565=EDGE_CURVE('',#8115,#7959,#9169,.T.);
#6566=EDGE_CURVE('',#8114,#7960,#9170,.T.);
#6567=EDGE_CURVE('',#8113,#7961,#9171,.T.);
#6568=EDGE_CURVE('',#8112,#7962,#9172,.T.);
#6569=EDGE_CURVE('',#8111,#7963,#9173,.T.);
#6570=EDGE_CURVE('',#8110,#7964,#9174,.T.);
#6571=EDGE_CURVE('',#8109,#7965,#9175,.T.);
#6572=EDGE_CURVE('',#8108,#7966,#9176,.T.);
#6573=EDGE_CURVE('',#8107,#7967,#9177,.T.);
#6574=EDGE_CURVE('',#8106,#7968,#9178,.T.);
#6575=EDGE_CURVE('',#8105,#7969,#9179,.T.);
#6576=EDGE_CURVE('',#8104,#7970,#9180,.T.);
#6577=EDGE_CURVE('',#8103,#7971,#9181,.T.);
#6578=EDGE_CURVE('',#8102,#7972,#9182,.T.);
#6579=EDGE_CURVE('',#8101,#7973,#9183,.T.);
#6580=EDGE_CURVE('',#8100,#7974,#9184,.T.);
#6581=EDGE_CURVE('',#8099,#7975,#9185,.T.);
#6582=EDGE_CURVE('',#8098,#7976,#9186,.T.);
#6583=EDGE_CURVE('',#8097,#7977,#9187,.T.);
#6584=EDGE_CURVE('',#8096,#7978,#9188,.T.);
#6585=EDGE_CURVE('',#8095,#7979,#9189,.T.);
#6586=EDGE_CURVE('',#8094,#7980,#9190,.T.);
#6587=EDGE_CURVE('',#8093,#7981,#9191,.T.);
#6588=EDGE_CURVE('',#8092,#7982,#9192,.T.);
#6589=EDGE_CURVE('',#8091,#7983,#9193,.T.);
#6590=EDGE_CURVE('',#8090,#7984,#9194,.T.);
#6591=EDGE_CURVE('',#8089,#7985,#9195,.T.);
#6592=EDGE_CURVE('',#8088,#7986,#9196,.T.);
#6593=EDGE_CURVE('',#8087,#7987,#9197,.T.);
#6594=EDGE_CURVE('',#8086,#7988,#9198,.T.);
#6595=EDGE_CURVE('',#8085,#7989,#9199,.T.);
#6596=EDGE_CURVE('',#8084,#7990,#9200,.T.);
#6597=EDGE_CURVE('',#8083,#7991,#9201,.T.);
#6598=EDGE_CURVE('',#8082,#7992,#9202,.T.);
#6599=EDGE_CURVE('',#8081,#7993,#9203,.T.);
#6600=EDGE_CURVE('',#8080,#7994,#9204,.T.);
#6601=EDGE_CURVE('',#8079,#7995,#9205,.T.);
#6602=EDGE_CURVE('',#8078,#7996,#9206,.T.);
#6603=EDGE_CURVE('',#8077,#7997,#9207,.T.);
#6604=EDGE_CURVE('',#8076,#7998,#9208,.T.);
#6605=EDGE_CURVE('',#8075,#7999,#9209,.T.);
#6606=EDGE_CURVE('',#8074,#8000,#9210,.T.);
#6607=EDGE_CURVE('',#8073,#8001,#9211,.T.);
#6608=EDGE_CURVE('',#8072,#8002,#9212,.T.);
#6609=EDGE_CURVE('',#8071,#8003,#9213,.T.);
#6610=EDGE_CURVE('',#8070,#8004,#9214,.T.);
#6611=EDGE_CURVE('',#8069,#8005,#9215,.T.);
#6612=EDGE_CURVE('',#8068,#8006,#9216,.T.);
#6613=EDGE_CURVE('',#8067,#8007,#9217,.T.);
#6614=EDGE_CURVE('',#8066,#8008,#9218,.T.);
#6615=EDGE_CURVE('',#8065,#8009,#9219,.T.);
#6616=EDGE_CURVE('',#8064,#8010,#9220,.T.);
#6617=EDGE_CURVE('',#8063,#8011,#9221,.T.);
#6618=EDGE_CURVE('',#8062,#8012,#9222,.T.);
#6619=EDGE_CURVE('',#8061,#8013,#9223,.T.);
#6620=EDGE_CURVE('',#8060,#8014,#9224,.T.);
#6621=EDGE_CURVE('',#8059,#8015,#9225,.T.);
#6622=EDGE_CURVE('',#8058,#8016,#9226,.T.);
#6623=EDGE_CURVE('',#8057,#8017,#9227,.T.);
#6624=EDGE_CURVE('',#8056,#8018,#9228,.T.);
#6625=EDGE_CURVE('',#8055,#8019,#9229,.T.);
#6626=EDGE_CURVE('',#8054,#8020,#9230,.T.);
#6627=EDGE_CURVE('',#8053,#8021,#9231,.T.);
#6628=EDGE_CURVE('',#8052,#8022,#9232,.T.);
#6629=EDGE_CURVE('',#8051,#8023,#9233,.T.);
#6630=EDGE_CURVE('',#8050,#8024,#9234,.T.);
#6631=EDGE_CURVE('',#8049,#8025,#9235,.T.);
#6632=EDGE_CURVE('',#8048,#8026,#9236,.T.);
#6633=EDGE_CURVE('',#8047,#8027,#9237,.T.);
#6634=EDGE_CURVE('',#8046,#8028,#9238,.T.);
#6635=EDGE_CURVE('',#8045,#8029,#9239,.T.);
#6636=EDGE_CURVE('',#8044,#8030,#9240,.T.);
#6637=EDGE_CURVE('',#8043,#8031,#9241,.T.);
#6638=EDGE_CURVE('',#8042,#8032,#9242,.T.);
#6639=EDGE_CURVE('',#8041,#8033,#9243,.T.);
#6640=EDGE_CURVE('',#8040,#8034,#9244,.T.);
#6641=EDGE_CURVE('',#8039,#8035,#9245,.T.);
#6642=EDGE_CURVE('',#8038,#7894,#9246,.T.);
#6643=EDGE_CURVE('',#7869,#7891,#743,.T.);
#6644=EDGE_CURVE('',#8181,#8181,#744,.T.);
#6645=EDGE_CURVE('',#8182,#8182,#745,.T.);
#6646=EDGE_CURVE('',#8183,#8183,#746,.T.);
#6647=EDGE_CURVE('',#8184,#8184,#747,.T.);
#6648=EDGE_CURVE('',#8185,#8185,#748,.T.);
#6649=EDGE_CURVE('',#8186,#8186,#749,.T.);
#6650=EDGE_CURVE('',#8187,#8187,#750,.T.);
#6651=EDGE_CURVE('',#8188,#8188,#751,.T.);
#6652=EDGE_CURVE('',#8189,#8189,#752,.T.);
#6653=EDGE_CURVE('',#8190,#8190,#753,.T.);
#6654=EDGE_CURVE('',#8191,#8191,#754,.T.);
#6655=EDGE_CURVE('',#8192,#8193,#755,.T.);
#6656=EDGE_CURVE('',#8194,#8192,#756,.T.);
#6657=EDGE_CURVE('',#8195,#8194,#757,.T.);
#6658=EDGE_CURVE('',#8193,#8195,#758,.T.);
#6659=EDGE_CURVE('',#8196,#8197,#759,.T.);
#6660=EDGE_CURVE('',#8195,#8196,#9247,.T.);
#6661=EDGE_CURVE('',#8194,#8197,#9248,.T.);
#6662=EDGE_CURVE('',#8198,#8199,#760,.T.);
#6663=EDGE_CURVE('',#8192,#8198,#9249,.T.);
#6664=EDGE_CURVE('',#8193,#8199,#9250,.T.);
#6665=EDGE_CURVE('',#8200,#8201,#761,.T.);
#6666=EDGE_CURVE('',#8202,#8200,#762,.T.);
#6667=EDGE_CURVE('',#8203,#8202,#763,.T.);
#6668=EDGE_CURVE('',#8201,#8203,#764,.T.);
#6669=EDGE_CURVE('',#8204,#8205,#765,.T.);
#6670=EDGE_CURVE('',#8201,#8204,#9251,.T.);
#6671=EDGE_CURVE('',#8203,#8205,#9252,.T.);
#6672=EDGE_CURVE('',#8206,#8207,#766,.T.);
#6673=EDGE_CURVE('',#8202,#8206,#9253,.T.);
#6674=EDGE_CURVE('',#8200,#8207,#9254,.T.);
#6675=EDGE_CURVE('',#8208,#8208,#767,.T.);
#6676=EDGE_CURVE('',#8209,#8209,#768,.T.);
#6677=EDGE_CURVE('',#8197,#8198,#769,.T.);
#6678=EDGE_CURVE('',#8199,#8196,#770,.T.);
#6679=EDGE_CURVE('',#8210,#8210,#771,.T.);
#6680=EDGE_CURVE('',#8211,#8211,#772,.T.);
#6681=EDGE_CURVE('',#8207,#8204,#773,.T.);
#6682=EDGE_CURVE('',#8205,#8206,#774,.T.);
#6683=EDGE_CURVE('',#8213,#8214,#9255,.T.);
#6684=EDGE_CURVE('',#8214,#8215,#9256,.T.);
#6685=EDGE_CURVE('',#8216,#8215,#9257,.T.);
#6686=EDGE_CURVE('',#8213,#8216,#9258,.T.);
#6687=EDGE_CURVE('',#8215,#8217,#775,.T.);
#6688=EDGE_CURVE('',#8218,#8217,#9259,.T.);
#6689=EDGE_CURVE('',#8216,#8218,#776,.T.);
#6690=EDGE_CURVE('',#8217,#8219,#9260,.T.);
#6691=EDGE_CURVE('',#8220,#8219,#9261,.T.);
#6692=EDGE_CURVE('',#8218,#8220,#9262,.T.);
#6693=EDGE_CURVE('',#8221,#8222,#9263,.T.);
#6694=EDGE_CURVE('',#8222,#8223,#9264,.T.);
#6695=EDGE_CURVE('',#8224,#8223,#9265,.T.);
#6696=EDGE_CURVE('',#8221,#8224,#9266,.T.);
#6697=EDGE_CURVE('',#8225,#8226,#9267,.T.);
#6698=EDGE_CURVE('',#8226,#8227,#9268,.T.);
#6699=EDGE_CURVE('',#8228,#8227,#9269,.T.);
#6700=EDGE_CURVE('',#8225,#8228,#9270,.T.);
#6701=EDGE_CURVE('',#8227,#8222,#777,.T.);
#6702=EDGE_CURVE('',#8228,#8221,#778,.T.);
#6703=EDGE_CURVE('',#8229,#8230,#9271,.T.);
#6704=EDGE_CURVE('',#8230,#8231,#9272,.T.);
#6705=EDGE_CURVE('',#8232,#8231,#9273,.T.);
#6706=EDGE_CURVE('',#8229,#8232,#9274,.T.);
#6707=EDGE_CURVE('',#8233,#8234,#9275,.T.);
#6708=EDGE_CURVE('',#8234,#8235,#9276,.T.);
#6709=EDGE_CURVE('',#8236,#8235,#9277,.T.);
#6710=EDGE_CURVE('',#8233,#8236,#9278,.T.);
#6711=EDGE_CURVE('',#8235,#8230,#779,.T.);
#6712=EDGE_CURVE('',#8236,#8229,#780,.T.);
#6713=EDGE_CURVE('',#8237,#8237,#781,.T.);
#6714=EDGE_CURVE('',#8238,#8238,#782,.T.);
#6715=EDGE_CURVE('',#8239,#8239,#783,.T.);
#6716=EDGE_CURVE('',#8240,#8240,#784,.T.);
#6717=EDGE_CURVE('',#8241,#8241,#785,.T.);
#6718=EDGE_CURVE('',#8242,#8242,#786,.T.);
#6719=EDGE_CURVE('',#8243,#8243,#787,.T.);
#6720=EDGE_CURVE('',#8244,#8244,#788,.T.);
#6721=EDGE_CURVE('',#8245,#8245,#789,.T.);
#6722=EDGE_CURVE('',#8231,#8234,#790,.T.);
#6723=EDGE_CURVE('',#8223,#8226,#791,.T.);
#6724=EDGE_CURVE('',#8219,#8214,#792,.T.);
#6725=EDGE_CURVE('',#8246,#8246,#793,.T.);
#6726=EDGE_CURVE('',#8247,#8247,#794,.T.);
#6727=EDGE_CURVE('',#8248,#8248,#795,.T.);
#6728=EDGE_CURVE('',#8249,#8249,#796,.T.);
#6729=EDGE_CURVE('',#8250,#8250,#797,.T.);
#6730=EDGE_CURVE('',#8232,#8233,#798,.T.);
#6731=EDGE_CURVE('',#8224,#8225,#799,.T.);
#6732=EDGE_CURVE('',#8220,#8213,#800,.T.);
#6733=EDGE_CURVE('',#8251,#8251,#801,.T.);
#6734=EDGE_CURVE('',#8252,#8252,#802,.T.);
#6735=EDGE_CURVE('',#8253,#8253,#803,.T.);
#6736=EDGE_CURVE('',#8254,#8254,#804,.T.);
#6737=EDGE_CURVE('',#8255,#8255,#805,.T.);
#6738=EDGE_CURVE('',#8256,#8256,#806,.T.);
#6739=EDGE_CURVE('',#8258,#8259,#807,.T.);
#6740=EDGE_CURVE('',#8259,#8260,#9279,.T.);
#6741=EDGE_CURVE('',#8260,#8261,#808,.T.);
#6742=EDGE_CURVE('',#8261,#8258,#9280,.T.);
#6743=EDGE_CURVE('',#8261,#8262,#9281,.T.);
#6744=EDGE_CURVE('',#8263,#8262,#9282,.T.);
#6745=EDGE_CURVE('',#8258,#8263,#9283,.T.);
#6746=EDGE_CURVE('',#8259,#8264,#9284,.T.);
#6747=EDGE_CURVE('',#8265,#8264,#9285,.T.);
#6748=EDGE_CURVE('',#8260,#8265,#9286,.T.);
#6749=EDGE_CURVE('',#8264,#8263,#809,.T.);
#6750=EDGE_CURVE('',#8266,#8267,#810,.T.);
#6751=EDGE_CURVE('',#8267,#8268,#9287,.T.);
#6752=EDGE_CURVE('',#8268,#8269,#811,.T.);
#6753=EDGE_CURVE('',#8269,#8266,#9288,.T.);
#6754=EDGE_CURVE('',#8269,#8270,#9289,.T.);
#6755=EDGE_CURVE('',#8271,#8270,#9290,.T.);
#6756=EDGE_CURVE('',#8266,#8271,#9291,.T.);
#6757=EDGE_CURVE('',#8267,#8272,#9292,.T.);
#6758=EDGE_CURVE('',#8273,#8272,#9293,.T.);
#6759=EDGE_CURVE('',#8268,#8273,#9294,.T.);
#6760=EDGE_CURVE('',#8272,#8271,#812,.T.);
#6761=EDGE_CURVE('',#8274,#8275,#813,.T.);
#6762=EDGE_CURVE('',#8275,#8276,#9295,.T.);
#6763=EDGE_CURVE('',#8276,#8277,#814,.T.);
#6764=EDGE_CURVE('',#8277,#8274,#9296,.T.);
#6765=EDGE_CURVE('',#8277,#8278,#9297,.T.);
#6766=EDGE_CURVE('',#8279,#8278,#9298,.T.);
#6767=EDGE_CURVE('',#8274,#8279,#9299,.T.);
#6768=EDGE_CURVE('',#8275,#8280,#9300,.T.);
#6769=EDGE_CURVE('',#8281,#8280,#9301,.T.);
#6770=EDGE_CURVE('',#8276,#8281,#9302,.T.);
#6771=EDGE_CURVE('',#8280,#8279,#815,.T.);
#6772=EDGE_CURVE('',#8282,#8282,#816,.T.);
#6773=EDGE_CURVE('',#8283,#8283,#817,.T.);
#6774=EDGE_CURVE('',#8278,#8281,#818,.T.);
#6775=EDGE_CURVE('',#8270,#8273,#819,.T.);
#6776=EDGE_CURVE('',#8262,#8265,#820,.T.);
#6777=EDGE_CURVE('',#8284,#8284,#821,.T.);
#6778=EDGE_CURVE('',#8285,#8285,#822,.T.);
#6779=EDGE_CURVE('',#8286,#8287,#9303,.T.);
#6780=EDGE_CURVE('',#8287,#8288,#9304,.T.);
#6781=EDGE_CURVE('',#8288,#8289,#9305,.T.);
#6782=EDGE_CURVE('',#8286,#8289,#9306,.T.);
#6783=EDGE_CURVE('',#8290,#8291,#9307,.T.);
#6784=EDGE_CURVE('',#8291,#8292,#9308,.T.);
#6785=EDGE_CURVE('',#8292,#8293,#9309,.T.);
#6786=EDGE_CURVE('',#8290,#8293,#9310,.T.);
#6787=EDGE_CURVE('',#8294,#8295,#9311,.T.);
#6788=EDGE_CURVE('',#8295,#8296,#9312,.T.);
#6789=EDGE_CURVE('',#8296,#8297,#9313,.T.);
#6790=EDGE_CURVE('',#8294,#8297,#9314,.T.);
#6791=EDGE_CURVE('',#8298,#8299,#9315,.T.);
#6792=EDGE_CURVE('',#8299,#8300,#9316,.T.);
#6793=EDGE_CURVE('',#8300,#8301,#9317,.T.);
#6794=EDGE_CURVE('',#8298,#8301,#9318,.T.);
#6795=EDGE_CURVE('',#8302,#8303,#823,.T.);
#6796=EDGE_CURVE('',#8304,#8302,#824,.T.);
#6797=EDGE_CURVE('',#8305,#8304,#825,.T.);
#6798=EDGE_CURVE('',#8303,#8305,#826,.T.);
#6799=EDGE_CURVE('',#8306,#8307,#827,.T.);
#6800=EDGE_CURVE('',#8305,#8306,#9319,.T.);
#6801=EDGE_CURVE('',#8304,#8307,#9320,.T.);
#6802=EDGE_CURVE('',#8308,#8309,#828,.T.);
#6803=EDGE_CURVE('',#8302,#8308,#9321,.T.);
#6804=EDGE_CURVE('',#8303,#8309,#9322,.T.);
#6805=EDGE_CURVE('',#8310,#8311,#829,.T.);
#6806=EDGE_CURVE('',#8312,#8310,#830,.T.);
#6807=EDGE_CURVE('',#8313,#8312,#831,.T.);
#6808=EDGE_CURVE('',#8311,#8313,#832,.T.);
#6809=EDGE_CURVE('',#8314,#8315,#833,.T.);
#6810=EDGE_CURVE('',#8311,#8314,#9323,.T.);
#6811=EDGE_CURVE('',#8313,#8315,#9324,.T.);
#6812=EDGE_CURVE('',#8316,#8317,#834,.T.);
#6813=EDGE_CURVE('',#8312,#8316,#9325,.T.);
#6814=EDGE_CURVE('',#8310,#8317,#9326,.T.);
#6815=EDGE_CURVE('',#8287,#8290,#835,.T.);
#6816=EDGE_CURVE('',#8286,#8299,#836,.T.);
#6817=EDGE_CURVE('',#8295,#8298,#837,.T.);
#6818=EDGE_CURVE('',#8294,#8291,#838,.T.);
#6819=EDGE_CURVE('',#8318,#8318,#839,.T.);
#6820=EDGE_CURVE('',#8289,#8300,#840,.T.);
#6821=EDGE_CURVE('',#8288,#8301,#841,.T.);
#6822=EDGE_CURVE('',#8317,#8314,#842,.T.);
#6823=EDGE_CURVE('',#8315,#8316,#843,.T.);
#6824=EDGE_CURVE('',#8297,#8292,#844,.T.);
#6825=EDGE_CURVE('',#8296,#8293,#845,.T.);
#6826=EDGE_CURVE('',#8307,#8308,#846,.T.);
#6827=EDGE_CURVE('',#8309,#8306,#847,.T.);
#6828=EDGE_CURVE('',#8319,#8319,#848,.T.);
#6829=EDGE_CURVE('',#8320,#8320,#849,.T.);
#6830=EDGE_CURVE('',#8321,#8322,#850,.T.);
#6831=EDGE_CURVE('',#8323,#8321,#9327,.T.);
#6832=EDGE_CURVE('',#8324,#8323,#851,.T.);
#6833=EDGE_CURVE('',#8322,#8324,#9328,.T.);
#6834=EDGE_CURVE('',#8325,#8325,#852,.T.);
#6835=EDGE_CURVE('',#8326,#8327,#853,.T.);
#6836=EDGE_CURVE('',#8326,#8328,#9329,.T.);
#6837=EDGE_CURVE('',#8329,#8328,#854,.T.);
#6838=EDGE_CURVE('',#8330,#8329,#9330,.T.);
#6839=EDGE_CURVE('',#8330,#8331,#855,.T.);
#6840=EDGE_CURVE('',#8324,#8331,#856,.T.);
#6841=EDGE_CURVE('',#8323,#8327,#9331,.T.);
#6842=EDGE_CURVE('',#8332,#8333,#857,.T.);
#6843=EDGE_CURVE('',#8331,#8332,#9332,.T.);
#6844=EDGE_CURVE('',#8333,#8330,#9333,.T.);
#6845=EDGE_CURVE('',#8334,#8334,#858,.T.);
#6846=EDGE_CURVE('',#8335,#8336,#859,.T.);
#6847=EDGE_CURVE('',#8321,#8336,#9334,.T.);
#6848=EDGE_CURVE('',#8322,#8332,#860,.T.);
#6849=EDGE_CURVE('',#8333,#8337,#9335,.T.);
#6850=EDGE_CURVE('',#8337,#8338,#861,.T.);
#6851=EDGE_CURVE('',#8335,#8338,#9336,.T.);
#6852=EDGE_CURVE('',#8339,#8339,#862,.T.);
#6853=EDGE_CURVE('',#8340,#8341,#863,.T.);
#6854=EDGE_CURVE('',#8340,#8342,#9337,.T.);
#6855=EDGE_CURVE('',#8343,#8342,#864,.T.);
#6856=EDGE_CURVE('',#8344,#8343,#9338,.T.);
#6857=EDGE_CURVE('',#8344,#8345,#865,.T.);
#6858=EDGE_CURVE('',#8346,#8345,#866,.T.);
#6859=EDGE_CURVE('',#8346,#8347,#867,.T.);
#6860=EDGE_CURVE('',#8347,#8341,#9339,.T.);
#6861=EDGE_CURVE('',#8348,#8349,#868,.T.);
#6862=EDGE_CURVE('',#8345,#8348,#9340,.T.);
#6863=EDGE_CURVE('',#8349,#8344,#9341,.T.);
#6864=EDGE_CURVE('',#8350,#8350,#869,.T.);
#6865=EDGE_CURVE('',#8351,#8352,#870,.T.);
#6866=EDGE_CURVE('',#8353,#8352,#9342,.T.);
#6867=EDGE_CURVE('',#8353,#8354,#871,.T.);
#6868=EDGE_CURVE('',#8354,#8348,#872,.T.);
#6869=EDGE_CURVE('',#8349,#8355,#9343,.T.);
#6870=EDGE_CURVE('',#8355,#8356,#873,.T.);
#6871=EDGE_CURVE('',#8351,#8356,#9344,.T.);
#6872=EDGE_CURVE('',#8347,#8353,#9345,.T.);
#6873=EDGE_CURVE('',#8354,#8346,#9346,.T.);
#6874=EDGE_CURVE('',#8357,#8357,#874,.T.);
#6875=EDGE_CURVE('',#8358,#8359,#875,.T.);
#6876=EDGE_CURVE('',#8358,#8360,#9347,.T.);
#6877=EDGE_CURVE('',#8361,#8360,#876,.T.);
#6878=EDGE_CURVE('',#8362,#8361,#9348,.T.);
#6879=EDGE_CURVE('',#8362,#8363,#877,.T.);
#6880=EDGE_CURVE('',#8364,#8363,#878,.T.);
#6881=EDGE_CURVE('',#8364,#8365,#879,.T.);
#6882=EDGE_CURVE('',#8365,#8359,#9349,.T.);
#6883=EDGE_CURVE('',#8366,#8366,#880,.T.);
#6884=EDGE_CURVE('',#8367,#8368,#881,.T.);
#6885=EDGE_CURVE('',#8369,#8368,#9350,.T.);
#6886=EDGE_CURVE('',#8369,#8370,#882,.T.);
#6887=EDGE_CURVE('',#8370,#8371,#883,.T.);
#6888=EDGE_CURVE('',#8371,#8372,#884,.T.);
#6889=EDGE_CURVE('',#8372,#8373,#9351,.T.);
#6890=EDGE_CURVE('',#8373,#8374,#885,.T.);
#6891=EDGE_CURVE('',#8367,#8374,#9352,.T.);
#6892=EDGE_CURVE('',#8375,#8375,#886,.T.);
#6893=EDGE_CURVE('',#8376,#8377,#887,.T.);
#6894=EDGE_CURVE('',#8376,#8378,#9353,.T.);
#6895=EDGE_CURVE('',#8379,#8378,#888,.T.);
#6896=EDGE_CURVE('',#8380,#8379,#9354,.T.);
#6897=EDGE_CURVE('',#8380,#8381,#889,.T.);
#6898=EDGE_CURVE('',#8382,#8381,#890,.T.);
#6899=EDGE_CURVE('',#8382,#8383,#891,.T.);
#6900=EDGE_CURVE('',#8383,#8377,#9355,.T.);
#6901=EDGE_CURVE('',#8384,#8385,#892,.T.);
#6902=EDGE_CURVE('',#8381,#8384,#9356,.T.);
#6903=EDGE_CURVE('',#8385,#8380,#9357,.T.);
#6904=EDGE_CURVE('',#8386,#8386,#893,.T.);
#6905=EDGE_CURVE('',#8387,#8388,#894,.T.);
#6906=EDGE_CURVE('',#8389,#8388,#9358,.T.);
#6907=EDGE_CURVE('',#8389,#8390,#895,.T.);
#6908=EDGE_CURVE('',#8390,#8384,#896,.T.);
#6909=EDGE_CURVE('',#8385,#8391,#9359,.T.);
#6910=EDGE_CURVE('',#8391,#8392,#897,.T.);
#6911=EDGE_CURVE('',#8387,#8392,#9360,.T.);
#6912=EDGE_CURVE('',#8383,#8389,#9361,.T.);
#6913=EDGE_CURVE('',#8390,#8382,#9362,.T.);
#6914=EDGE_CURVE('',#8336,#8327,#9363,.T.);
#6915=EDGE_CURVE('',#8335,#8326,#9364,.T.);
#6916=EDGE_CURVE('',#8338,#8328,#9365,.T.);
#6917=EDGE_CURVE('',#8337,#8329,#9366,.T.);
#6918=EDGE_CURVE('',#8352,#8341,#9367,.T.);
#6919=EDGE_CURVE('',#8351,#8340,#9368,.T.);
#6920=EDGE_CURVE('',#8356,#8342,#9369,.T.);
#6921=EDGE_CURVE('',#8355,#8343,#9370,.T.);
#6922=EDGE_CURVE('',#8368,#8359,#9371,.T.);
#6923=EDGE_CURVE('',#8367,#8358,#9372,.T.);
#6924=EDGE_CURVE('',#8374,#8360,#9373,.T.);
#6925=EDGE_CURVE('',#8373,#8361,#9374,.T.);
#6926=EDGE_CURVE('',#8372,#8362,#9375,.T.);
#6927=EDGE_CURVE('',#8365,#8369,#9376,.T.);
#6928=EDGE_CURVE('',#8388,#8377,#9377,.T.);
#6929=EDGE_CURVE('',#8387,#8376,#9378,.T.);
#6930=EDGE_CURVE('',#8392,#8378,#9379,.T.);
#6931=EDGE_CURVE('',#8391,#8379,#9380,.T.);
#6932=EDGE_CURVE('',#8393,#8393,#898,.T.);
#6933=EDGE_CURVE('',#8394,#8395,#9381,.T.);
#6934=EDGE_CURVE('',#8395,#8396,#1911,.T.);
#6935=EDGE_CURVE('',#8396,#8397,#1912,.T.);
#6936=EDGE_CURVE('',#8397,#8398,#1913,.T.);
#6937=EDGE_CURVE('',#8398,#8399,#1914,.T.);
#6938=EDGE_CURVE('',#8399,#8400,#1915,.T.);
#6939=EDGE_CURVE('',#8400,#8401,#1916,.T.);
#6940=EDGE_CURVE('',#8401,#8402,#1917,.T.);
#6941=EDGE_CURVE('',#8402,#8403,#1918,.T.);
#6942=EDGE_CURVE('',#8403,#8404,#9382,.T.);
#6943=EDGE_CURVE('',#8394,#8404,#1919,.T.);
#6944=EDGE_CURVE('',#8405,#8406,#9383,.T.);
#6945=EDGE_CURVE('',#8406,#8407,#1920,.T.);
#6946=EDGE_CURVE('',#8407,#8408,#9384,.T.);
#6947=EDGE_CURVE('',#8409,#8408,#1921,.T.);
#6948=EDGE_CURVE('',#8410,#8409,#1922,.T.);
#6949=EDGE_CURVE('',#8411,#8410,#1923,.T.);
#6950=EDGE_CURVE('',#8412,#8411,#1924,.T.);
#6951=EDGE_CURVE('',#8413,#8412,#1925,.T.);
#6952=EDGE_CURVE('',#8414,#8413,#1926,.T.);
#6953=EDGE_CURVE('',#8415,#8414,#1927,.T.);
#6954=EDGE_CURVE('',#8405,#8415,#1928,.T.);
#6955=EDGE_CURVE('',#8406,#8394,#9385,.T.);
#6956=EDGE_CURVE('',#8404,#8407,#9386,.T.);
#6957=EDGE_CURVE('',#8408,#8403,#9387,.T.);
#6958=EDGE_CURVE('',#8395,#8405,#9388,.T.);
#6959=EDGE_CURVE('',#8405,#8405,#899,.T.);
#6960=EDGE_CURVE('',#8416,#8416,#900,.T.);
#6961=EDGE_CURVE('',#8417,#8418,#1110,.F.);
#6962=EDGE_CURVE('',#8419,#8417,#1111,.F.);
#6963=EDGE_CURVE('',#8420,#8419,#1112,.F.);
#6964=EDGE_CURVE('',#8420,#8421,#1113,.F.);
#6965=EDGE_CURVE('',#8422,#8421,#1114,.T.);
#6966=EDGE_CURVE('',#8423,#8422,#1115,.T.);
#6967=EDGE_CURVE('',#8424,#8423,#1116,.T.);
#6968=EDGE_CURVE('',#8425,#8424,#1117,.T.);
#6969=EDGE_CURVE('',#8426,#8425,#1118,.T.);
#6970=EDGE_CURVE('',#8427,#8426,#1119,.T.);
#6971=EDGE_CURVE('',#8428,#8427,#1120,.T.);
#6972=EDGE_CURVE('',#8428,#8418,#1121,.F.);
#6973=EDGE_CURVE('',#8429,#8430,#1122,.T.);
#6974=EDGE_CURVE('',#8421,#8430,#1123,.F.);
#6975=EDGE_CURVE('',#8431,#8420,#1124,.F.);
#6976=EDGE_CURVE('',#8432,#8431,#1125,.T.);
#6977=EDGE_CURVE('',#8429,#8432,#901,.T.);
#6978=EDGE_CURVE('',#8433,#8434,#1126,.T.);
#6979=EDGE_CURVE('',#8418,#8433,#1127,.F.);
#6980=EDGE_CURVE('',#8435,#8428,#1128,.F.);
#6981=EDGE_CURVE('',#8435,#8436,#1129,.T.);
#6982=EDGE_CURVE('',#8436,#8437,#1130,.T.);
#6983=EDGE_CURVE('',#8434,#8437,#1131,.F.);
#6984=EDGE_CURVE('',#8438,#8439,#902,.T.);
#6985=EDGE_CURVE('',#8440,#8439,#1132,.T.);
#6986=EDGE_CURVE('',#8441,#8440,#1133,.T.);
#6987=EDGE_CURVE('',#8442,#8441,#1134,.T.);
#6988=EDGE_CURVE('',#8443,#8442,#1135,.T.);
#6989=EDGE_CURVE('',#8444,#8443,#1136,.T.);
#6990=EDGE_CURVE('',#8445,#8444,#1137,.T.);
#6991=EDGE_CURVE('',#8430,#8445,#1138,.T.);
#6992=EDGE_CURVE('',#8446,#8429,#1139,.F.);
#6993=EDGE_CURVE('',#8438,#8446,#1140,.F.);
#6994=EDGE_CURVE('',#8447,#8435,#1141,.T.);
#6995=EDGE_CURVE('',#8447,#8436,#1142,.T.);
#6996=EDGE_CURVE('',#8439,#8447,#1143,.T.);
#6997=EDGE_CURVE('',#8437,#8438,#1144,.F.);
#6998=EDGE_CURVE('',#8432,#8431,#903,.T.);
#6999=EDGE_CURVE('',#8434,#8433,#904,.T.);
#7000=EDGE_CURVE('',#8448,#8448,#905,.T.);
#7001=EDGE_CURVE('',#8449,#8449,#906,.T.);
#7002=EDGE_CURVE('',#8450,#8450,#907,.T.);
#7003=EDGE_CURVE('',#8451,#8452,#908,.T.);
#7004=EDGE_CURVE('',#8451,#8452,#909,.T.);
#7005=EDGE_CURVE('',#8453,#8453,#910,.T.);
#7006=EDGE_CURVE('',#8454,#8455,#911,.T.);
#7007=EDGE_CURVE('',#8455,#8454,#912,.T.);
#7008=EDGE_CURVE('',#8456,#8456,#913,.T.);
#7009=EDGE_CURVE('',#8457,#8457,#914,.T.);
#7010=EDGE_CURVE('',#8455,#8454,#1145,.T.);
#7011=EDGE_CURVE('',#8439,#8435,#915,.T.);
#7012=EDGE_CURVE('',#8458,#8458,#916,.T.);
#7013=EDGE_CURVE('',#8459,#8459,#917,.T.);
#7014=EDGE_CURVE('',#8460,#8460,#918,.T.);
#7015=EDGE_CURVE('',#8461,#8461,#919,.T.);
#7016=EDGE_CURVE('',#8462,#8462,#920,.T.);
#7017=EDGE_CURVE('',#8463,#8463,#921,.T.);
#7018=EDGE_CURVE('',#8464,#8464,#922,.T.);
#7019=EDGE_CURVE('',#8465,#8465,#923,.T.);
#7020=EDGE_CURVE('',#8452,#8451,#1146,.T.);
#7021=EDGE_CURVE('',#8466,#8466,#924,.T.);
#7022=EDGE_CURVE('',#8467,#8467,#925,.T.);
#7023=EDGE_CURVE('',#8370,#8364,#9389,.T.);
#7024=EDGE_CURVE('',#8363,#8371,#9390,.T.);
#7025=EDGE_CURVE('',#8468,#8469,#926,.T.);
#7026=EDGE_CURVE('',#8469,#8470,#9391,.T.);
#7027=EDGE_CURVE('',#8470,#8471,#927,.T.);
#7028=EDGE_CURVE('',#8471,#8468,#9392,.T.);
#7029=EDGE_CURVE('',#8472,#8473,#9393,.T.);
#7030=EDGE_CURVE('',#8468,#8472,#9394,.T.);
#7031=EDGE_CURVE('',#8471,#8473,#9395,.T.);
#7032=EDGE_CURVE('',#8474,#8475,#9396,.T.);
#7033=EDGE_CURVE('',#8470,#8474,#9397,.T.);
#7034=EDGE_CURVE('',#8469,#8475,#9398,.T.);
#7035=EDGE_CURVE('',#8475,#8472,#928,.T.);
#7036=EDGE_CURVE('',#8476,#8477,#929,.T.);
#7037=EDGE_CURVE('',#8477,#8478,#9399,.T.);
#7038=EDGE_CURVE('',#8478,#8479,#930,.T.);
#7039=EDGE_CURVE('',#8479,#8476,#9400,.T.);
#7040=EDGE_CURVE('',#8480,#8481,#9401,.T.);
#7041=EDGE_CURVE('',#8476,#8480,#9402,.T.);
#7042=EDGE_CURVE('',#8479,#8481,#9403,.T.);
#7043=EDGE_CURVE('',#8482,#8483,#9404,.T.);
#7044=EDGE_CURVE('',#8478,#8482,#9405,.T.);
#7045=EDGE_CURVE('',#8477,#8483,#9406,.T.);
#7046=EDGE_CURVE('',#8483,#8480,#931,.T.);
#7047=EDGE_CURVE('',#8484,#8485,#932,.T.);
#7048=EDGE_CURVE('',#8485,#8486,#9407,.T.);
#7049=EDGE_CURVE('',#8486,#8487,#933,.T.);
#7050=EDGE_CURVE('',#8487,#8484,#9408,.T.);
#7051=EDGE_CURVE('',#8488,#8489,#9409,.T.);
#7052=EDGE_CURVE('',#8484,#8488,#9410,.T.);
#7053=EDGE_CURVE('',#8487,#8489,#9411,.T.);
#7054=EDGE_CURVE('',#8490,#8491,#9412,.T.);
#7055=EDGE_CURVE('',#8486,#8490,#9413,.T.);
#7056=EDGE_CURVE('',#8485,#8491,#9414,.T.);
#7057=EDGE_CURVE('',#8491,#8488,#934,.T.);
#7058=EDGE_CURVE('',#8492,#8492,#935,.T.);
#7059=EDGE_CURVE('',#8493,#8493,#936,.T.);
#7060=EDGE_CURVE('',#8494,#8494,#937,.T.);
#7061=EDGE_CURVE('',#8495,#8495,#938,.T.);
#7062=EDGE_CURVE('',#8496,#8496,#939,.T.);
#7063=EDGE_CURVE('',#8489,#8490,#940,.T.);
#7064=EDGE_CURVE('',#8481,#8482,#941,.T.);
#7065=EDGE_CURVE('',#8473,#8474,#942,.T.);
#7066=EDGE_CURVE('',#8497,#8497,#943,.T.);
#7067=EDGE_CURVE('',#8498,#8498,#944,.T.);
#7068=EDGE_CURVE('',#8499,#8499,#945,.T.);
#7069=EDGE_CURVE('',#8500,#8500,#946,.T.);
#7070=EDGE_CURVE('',#8501,#8501,#947,.T.);
#7071=EDGE_CURVE('',#8502,#8502,#948,.T.);
#7072=EDGE_CURVE('',#8503,#8503,#949,.T.);
#7073=EDGE_CURVE('',#8504,#8505,#9415,.T.);
#7074=EDGE_CURVE('',#8504,#8506,#1929,.T.);
#7075=EDGE_CURVE('',#8507,#8506,#9416,.T.);
#7076=EDGE_CURVE('',#8508,#8507,#1930,.T.);
#7077=EDGE_CURVE('',#8509,#8508,#1931,.T.);
#7078=EDGE_CURVE('',#8510,#8509,#1932,.T.);
#7079=EDGE_CURVE('',#8511,#8510,#1933,.T.);
#7080=EDGE_CURVE('',#8512,#8511,#1934,.T.);
#7081=EDGE_CURVE('',#8513,#8512,#1935,.T.);
#7082=EDGE_CURVE('',#8514,#8513,#1936,.T.);
#7083=EDGE_CURVE('',#8515,#8514,#1937,.T.);
#7084=EDGE_CURVE('',#8505,#8515,#1938,.T.);
#7085=EDGE_CURVE('',#8516,#8517,#9417,.T.);
#7086=EDGE_CURVE('',#8516,#8518,#1939,.T.);
#7087=EDGE_CURVE('',#8518,#8519,#1940,.T.);
#7088=EDGE_CURVE('',#8519,#8520,#1941,.T.);
#7089=EDGE_CURVE('',#8520,#8521,#1942,.T.);
#7090=EDGE_CURVE('',#8521,#8522,#1943,.T.);
#7091=EDGE_CURVE('',#8522,#8523,#1944,.T.);
#7092=EDGE_CURVE('',#8523,#8524,#1945,.T.);
#7093=EDGE_CURVE('',#8524,#8525,#1946,.T.);
#7094=EDGE_CURVE('',#8525,#8526,#1147,.T.);
#7095=EDGE_CURVE('',#8527,#8526,#9418,.T.);
#7096=EDGE_CURVE('',#8517,#8527,#1947,.T.);
#7097=EDGE_CURVE('',#8517,#8504,#9419,.T.);
#7098=EDGE_CURVE('',#8506,#8527,#9420,.T.);
#7099=EDGE_CURVE('',#8526,#8507,#9421,.T.);
#7100=EDGE_CURVE('',#8505,#8516,#9422,.T.);
#7101=EDGE_CURVE('',#8528,#8529,#9423,.T.);
#7102=EDGE_CURVE('',#8529,#8530,#9424,.T.);
#7103=EDGE_CURVE('',#8531,#8530,#9425,.T.);
#7104=EDGE_CURVE('',#8531,#8528,#9426,.T.);
#7105=EDGE_CURVE('',#8532,#8531,#9427,.T.);
#7106=EDGE_CURVE('',#8530,#8533,#9428,.T.);
#7107=EDGE_CURVE('',#8532,#8533,#9429,.T.);
#7108=EDGE_CURVE('',#8534,#8535,#9430,.T.);
#7109=EDGE_CURVE('',#8535,#8532,#9431,.T.);
#7110=EDGE_CURVE('',#8533,#8534,#9432,.T.);
#7111=EDGE_CURVE('',#8536,#8537,#9433,.T.);
#7112=EDGE_CURVE('',#8537,#8538,#9434,.T.);
#7113=EDGE_CURVE('',#8539,#8538,#9435,.T.);
#7114=EDGE_CURVE('',#8539,#8536,#9436,.T.);
#7115=EDGE_CURVE('',#8540,#8539,#9437,.T.);
#7116=EDGE_CURVE('',#8538,#8541,#9438,.T.);
#7117=EDGE_CURVE('',#8540,#8541,#9439,.T.);
#7118=EDGE_CURVE('',#8542,#8543,#9440,.T.);
#7119=EDGE_CURVE('',#8543,#8540,#9441,.T.);
#7120=EDGE_CURVE('',#8541,#8542,#9442,.T.);
#7121=EDGE_CURVE('',#8544,#8545,#9443,.T.);
#7122=EDGE_CURVE('',#8545,#8546,#9444,.T.);
#7123=EDGE_CURVE('',#8547,#8546,#9445,.T.);
#7124=EDGE_CURVE('',#8547,#8544,#9446,.T.);
#7125=EDGE_CURVE('',#8548,#8547,#9447,.T.);
#7126=EDGE_CURVE('',#8546,#8549,#9448,.T.);
#7127=EDGE_CURVE('',#8548,#8549,#9449,.T.);
#7128=EDGE_CURVE('',#8550,#8551,#9450,.T.);
#7129=EDGE_CURVE('',#8551,#8548,#9451,.T.);
#7130=EDGE_CURVE('',#8549,#8550,#9452,.T.);
#7131=EDGE_CURVE('',#8552,#8553,#9453,.T.);
#7132=EDGE_CURVE('',#8553,#8554,#9454,.T.);
#7133=EDGE_CURVE('',#8555,#8554,#9455,.T.);
#7134=EDGE_CURVE('',#8555,#8552,#9456,.T.);
#7135=EDGE_CURVE('',#8556,#8555,#9457,.T.);
#7136=EDGE_CURVE('',#8554,#8557,#9458,.T.);
#7137=EDGE_CURVE('',#8556,#8557,#9459,.T.);
#7138=EDGE_CURVE('',#8558,#8559,#9460,.T.);
#7139=EDGE_CURVE('',#8559,#8556,#9461,.T.);
#7140=EDGE_CURVE('',#8557,#8558,#9462,.T.);
#7141=EDGE_CURVE('',#8560,#8561,#9463,.T.);
#7142=EDGE_CURVE('',#8561,#8562,#9464,.T.);
#7143=EDGE_CURVE('',#8563,#8562,#9465,.T.);
#7144=EDGE_CURVE('',#8563,#8560,#9466,.T.);
#7145=EDGE_CURVE('',#8564,#8563,#9467,.T.);
#7146=EDGE_CURVE('',#8562,#8565,#9468,.T.);
#7147=EDGE_CURVE('',#8564,#8565,#9469,.T.);
#7148=EDGE_CURVE('',#8566,#8567,#9470,.T.);
#7149=EDGE_CURVE('',#8567,#8564,#9471,.T.);
#7150=EDGE_CURVE('',#8565,#8566,#9472,.T.);
#7151=EDGE_CURVE('',#8568,#8569,#9473,.T.);
#7152=EDGE_CURVE('',#8569,#8570,#9474,.T.);
#7153=EDGE_CURVE('',#8571,#8570,#9475,.T.);
#7154=EDGE_CURVE('',#8571,#8568,#9476,.T.);
#7155=EDGE_CURVE('',#8572,#8571,#9477,.T.);
#7156=EDGE_CURVE('',#8570,#8573,#9478,.T.);
#7157=EDGE_CURVE('',#8572,#8573,#9479,.T.);
#7158=EDGE_CURVE('',#8574,#8575,#9480,.T.);
#7159=EDGE_CURVE('',#8575,#8572,#9481,.T.);
#7160=EDGE_CURVE('',#8573,#8574,#9482,.T.);
#7161=EDGE_CURVE('',#8576,#8577,#9483,.T.);
#7162=EDGE_CURVE('',#8577,#8578,#9484,.T.);
#7163=EDGE_CURVE('',#8579,#8578,#9485,.T.);
#7164=EDGE_CURVE('',#8579,#8576,#9486,.T.);
#7165=EDGE_CURVE('',#8580,#8579,#9487,.T.);
#7166=EDGE_CURVE('',#8578,#8581,#9488,.T.);
#7167=EDGE_CURVE('',#8580,#8581,#9489,.T.);
#7168=EDGE_CURVE('',#8582,#8583,#9490,.T.);
#7169=EDGE_CURVE('',#8583,#8580,#9491,.T.);
#7170=EDGE_CURVE('',#8581,#8582,#9492,.T.);
#7171=EDGE_CURVE('',#8584,#8585,#9493,.T.);
#7172=EDGE_CURVE('',#8585,#8586,#9494,.T.);
#7173=EDGE_CURVE('',#8587,#8586,#9495,.T.);
#7174=EDGE_CURVE('',#8587,#8584,#9496,.T.);
#7175=EDGE_CURVE('',#8588,#8587,#9497,.T.);
#7176=EDGE_CURVE('',#8586,#8589,#9498,.T.);
#7177=EDGE_CURVE('',#8588,#8589,#9499,.T.);
#7178=EDGE_CURVE('',#8590,#8591,#9500,.T.);
#7179=EDGE_CURVE('',#8591,#8588,#9501,.T.);
#7180=EDGE_CURVE('',#8589,#8590,#9502,.T.);
#7181=EDGE_CURVE('',#8592,#8593,#9503,.T.);
#7182=EDGE_CURVE('',#8593,#8594,#9504,.T.);
#7183=EDGE_CURVE('',#8595,#8594,#9505,.T.);
#7184=EDGE_CURVE('',#8595,#8592,#9506,.T.);
#7185=EDGE_CURVE('',#8596,#8595,#9507,.T.);
#7186=EDGE_CURVE('',#8594,#8597,#9508,.T.);
#7187=EDGE_CURVE('',#8596,#8597,#9509,.T.);
#7188=EDGE_CURVE('',#8598,#8599,#9510,.T.);
#7189=EDGE_CURVE('',#8599,#8596,#9511,.T.);
#7190=EDGE_CURVE('',#8597,#8598,#9512,.T.);
#7191=EDGE_CURVE('',#8600,#8601,#9513,.T.);
#7192=EDGE_CURVE('',#8601,#8602,#9514,.T.);
#7193=EDGE_CURVE('',#8603,#8602,#9515,.T.);
#7194=EDGE_CURVE('',#8603,#8600,#9516,.T.);
#7195=EDGE_CURVE('',#8604,#8603,#9517,.T.);
#7196=EDGE_CURVE('',#8602,#8605,#9518,.T.);
#7197=EDGE_CURVE('',#8604,#8605,#9519,.T.);
#7198=EDGE_CURVE('',#8606,#8607,#9520,.T.);
#7199=EDGE_CURVE('',#8607,#8604,#9521,.T.);
#7200=EDGE_CURVE('',#8605,#8606,#9522,.T.);
#7201=EDGE_CURVE('',#8608,#8609,#9523,.T.);
#7202=EDGE_CURVE('',#8609,#8610,#9524,.T.);
#7203=EDGE_CURVE('',#8611,#8610,#9525,.T.);
#7204=EDGE_CURVE('',#8611,#8608,#9526,.T.);
#7205=EDGE_CURVE('',#8612,#8611,#9527,.T.);
#7206=EDGE_CURVE('',#8610,#8613,#9528,.T.);
#7207=EDGE_CURVE('',#8612,#8613,#9529,.T.);
#7208=EDGE_CURVE('',#8614,#8615,#9530,.T.);
#7209=EDGE_CURVE('',#8615,#8612,#9531,.T.);
#7210=EDGE_CURVE('',#8613,#8614,#9532,.T.);
#7211=EDGE_CURVE('',#8529,#8614,#950,.T.);
#7212=EDGE_CURVE('',#8609,#8606,#951,.T.);
#7213=EDGE_CURVE('',#8601,#8598,#952,.T.);
#7214=EDGE_CURVE('',#8593,#8590,#953,.T.);
#7215=EDGE_CURVE('',#8585,#8582,#954,.T.);
#7216=EDGE_CURVE('',#8577,#8574,#955,.T.);
#7217=EDGE_CURVE('',#8569,#8566,#956,.T.);
#7218=EDGE_CURVE('',#8561,#8558,#957,.T.);
#7219=EDGE_CURVE('',#8553,#8550,#958,.T.);
#7220=EDGE_CURVE('',#8545,#8542,#959,.T.);
#7221=EDGE_CURVE('',#8537,#8534,#960,.T.);
#7222=EDGE_CURVE('',#8616,#8616,#961,.T.);
#7223=EDGE_CURVE('',#8536,#8535,#962,.T.);
#7224=EDGE_CURVE('',#8544,#8543,#963,.T.);
#7225=EDGE_CURVE('',#8552,#8551,#964,.T.);
#7226=EDGE_CURVE('',#8560,#8559,#965,.T.);
#7227=EDGE_CURVE('',#8568,#8567,#966,.T.);
#7228=EDGE_CURVE('',#8576,#8575,#967,.T.);
#7229=EDGE_CURVE('',#8584,#8583,#968,.T.);
#7230=EDGE_CURVE('',#8592,#8591,#969,.T.);
#7231=EDGE_CURVE('',#8600,#8599,#970,.T.);
#7232=EDGE_CURVE('',#8608,#8607,#971,.T.);
#7233=EDGE_CURVE('',#8528,#8615,#972,.T.);
#7234=EDGE_CURVE('',#8516,#8516,#973,.T.);
#7235=EDGE_CURVE('',#8617,#8617,#974,.T.);
#7236=EDGE_CURVE('',#8618,#8618,#975,.T.);
#7237=EDGE_CURVE('',#8619,#8620,#976,.T.);
#7238=EDGE_CURVE('',#8620,#8621,#977,.T.);
#7239=EDGE_CURVE('',#8621,#8622,#978,.T.);
#7240=EDGE_CURVE('',#8622,#8619,#979,.T.);
#7241=EDGE_CURVE('',#8623,#8624,#980,.T.);
#7242=EDGE_CURVE('',#8622,#8624,#9533,.T.);
#7243=EDGE_CURVE('',#8621,#8623,#9534,.T.);
#7244=EDGE_CURVE('',#8625,#8626,#981,.T.);
#7245=EDGE_CURVE('',#8620,#8626,#9535,.T.);
#7246=EDGE_CURVE('',#8619,#8625,#9536,.T.);
#7247=EDGE_CURVE('',#8627,#8628,#982,.T.);
#7248=EDGE_CURVE('',#8628,#8629,#983,.T.);
#7249=EDGE_CURVE('',#8629,#8630,#984,.T.);
#7250=EDGE_CURVE('',#8630,#8627,#985,.T.);
#7251=EDGE_CURVE('',#8631,#8632,#986,.T.);
#7252=EDGE_CURVE('',#8630,#8632,#9537,.T.);
#7253=EDGE_CURVE('',#8629,#8631,#9538,.T.);
#7254=EDGE_CURVE('',#8633,#8634,#987,.T.);
#7255=EDGE_CURVE('',#8628,#8634,#9539,.T.);
#7256=EDGE_CURVE('',#8627,#8633,#9540,.T.);
#7257=EDGE_CURVE('',#8635,#8636,#9541,.T.);
#7258=EDGE_CURVE('',#8635,#8637,#988,.T.);
#7259=EDGE_CURVE('',#8638,#8637,#989,.T.);
#7260=EDGE_CURVE('',#8638,#8639,#990,.T.);
#7261=EDGE_CURVE('',#8640,#8639,#9542,.T.);
#7262=EDGE_CURVE('',#8640,#8636,#991,.T.);
#7263=EDGE_CURVE('',#8641,#8642,#9543,.T.);
#7264=EDGE_CURVE('',#8641,#8643,#1948,.T.);
#7265=EDGE_CURVE('',#8644,#8643,#9544,.T.);
#7266=EDGE_CURVE('',#8645,#8644,#1949,.T.);
#7267=EDGE_CURVE('',#8646,#8645,#1950,.T.);
#7268=EDGE_CURVE('',#8647,#8646,#1951,.T.);
#7269=EDGE_CURVE('',#8648,#8647,#1952,.T.);
#7270=EDGE_CURVE('',#8649,#8648,#1953,.T.);
#7271=EDGE_CURVE('',#8650,#8649,#1954,.T.);
#7272=EDGE_CURVE('',#8651,#8650,#1955,.T.);
#7273=EDGE_CURVE('',#8642,#8651,#1956,.T.);
#7274=EDGE_CURVE('',#8652,#8653,#9545,.T.);
#7275=EDGE_CURVE('',#8652,#8654,#1957,.T.);
#7276=EDGE_CURVE('',#8654,#8655,#1958,.T.);
#7277=EDGE_CURVE('',#8655,#8656,#1959,.T.);
#7278=EDGE_CURVE('',#8656,#8657,#1960,.T.);
#7279=EDGE_CURVE('',#8657,#8658,#1961,.T.);
#7280=EDGE_CURVE('',#8658,#8659,#1962,.T.);
#7281=EDGE_CURVE('',#8659,#8660,#1963,.T.);
#7282=EDGE_CURVE('',#8660,#8661,#1964,.T.);
#7283=EDGE_CURVE('',#8662,#8661,#9546,.T.);
#7284=EDGE_CURVE('',#8653,#8662,#1965,.T.);
#7285=EDGE_CURVE('',#8653,#8641,#9547,.T.);
#7286=EDGE_CURVE('',#8643,#8662,#9548,.T.);
#7287=EDGE_CURVE('',#8661,#8644,#9549,.T.);
#7288=EDGE_CURVE('',#8642,#8652,#9550,.T.);
#7289=EDGE_CURVE('',#8663,#8664,#9551,.T.);
#7290=EDGE_CURVE('',#8664,#8665,#992,.T.);
#7291=EDGE_CURVE('',#8665,#8666,#9552,.T.);
#7292=EDGE_CURVE('',#8666,#8663,#993,.T.);
#7293=EDGE_CURVE('',#8667,#8667,#994,.T.);
#7294=EDGE_CURVE('',#8668,#8668,#995,.T.);
#7295=EDGE_CURVE('',#8638,#8669,#9553,.T.);
#7296=EDGE_CURVE('',#8669,#8670,#996,.T.);
#7297=EDGE_CURVE('',#8670,#8637,#9554,.T.);
#7298=EDGE_CURVE('',#8635,#8671,#9555,.T.);
#7299=EDGE_CURVE('',#8671,#8672,#997,.T.);
#7300=EDGE_CURVE('',#8639,#8672,#9556,.T.);
#7301=EDGE_CURVE('',#8673,#8673,#998,.T.);
#7302=EDGE_CURVE('',#8674,#8674,#999,.T.);
#7303=EDGE_CURVE('',#8671,#8675,#9557,.T.);
#7304=EDGE_CURVE('',#8675,#8676,#1000,.T.);
#7305=EDGE_CURVE('',#8676,#8672,#9558,.T.);
#7306=EDGE_CURVE('',#8640,#8676,#9559,.T.);
#7307=EDGE_CURVE('',#8636,#8675,#9560,.T.);
#7308=EDGE_CURVE('',#8626,#8623,#1001,.T.);
#7309=EDGE_CURVE('',#8624,#8625,#1002,.T.);
#7310=EDGE_CURVE('',#8663,#8666,#1003,.T.);
#7311=EDGE_CURVE('',#8652,#8652,#1004,.T.);
#7312=EDGE_CURVE('',#8669,#8670,#1005,.T.);
#7313=EDGE_CURVE('',#8632,#8633,#1006,.T.);
#7314=EDGE_CURVE('',#8634,#8631,#1007,.T.);
#7315=EDGE_CURVE('',#8664,#8665,#1148,.T.);
#7316=EDGE_CURVE('',#8677,#8677,#1008,.T.);
#7317=EDGE_CURVE('',#8678,#8679,#9561,.T.);
#7318=EDGE_CURVE('',#8680,#8679,#9562,.T.);
#7319=EDGE_CURVE('',#8680,#8681,#9563,.T.);
#7320=EDGE_CURVE('',#8681,#8682,#9564,.T.);
#7321=EDGE_CURVE('',#8682,#8678,#9565,.T.);
#7322=EDGE_CURVE('',#8679,#8683,#1009,.T.);
#7323=EDGE_CURVE('',#8684,#8683,#9566,.T.);
#7324=EDGE_CURVE('',#8684,#8680,#1010,.T.);
#7325=EDGE_CURVE('',#8683,#8685,#9567,.T.);
#7326=EDGE_CURVE('',#8686,#8685,#9568,.T.);
#7327=EDGE_CURVE('',#8686,#8687,#9569,.T.);
#7328=EDGE_CURVE('',#8687,#8684,#9570,.T.);
#7329=EDGE_CURVE('',#8686,#8682,#1011,.T.);
#7330=EDGE_CURVE('',#8685,#8678,#1012,.T.);
#7331=EDGE_CURVE('',#8688,#8689,#9571,.T.);
#7332=EDGE_CURVE('',#8690,#8689,#9572,.T.);
#7333=EDGE_CURVE('',#8690,#8691,#9573,.T.);
#7334=EDGE_CURVE('',#8691,#8692,#9574,.T.);
#7335=EDGE_CURVE('',#8692,#8688,#9575,.T.);
#7336=EDGE_CURVE('',#8689,#8693,#1013,.T.);
#7337=EDGE_CURVE('',#8694,#8693,#9576,.T.);
#7338=EDGE_CURVE('',#8694,#8690,#1014,.T.);
#7339=EDGE_CURVE('',#8693,#8695,#9577,.T.);
#7340=EDGE_CURVE('',#8696,#8695,#9578,.T.);
#7341=EDGE_CURVE('',#8696,#8697,#9579,.T.);
#7342=EDGE_CURVE('',#8697,#8694,#9580,.T.);
#7343=EDGE_CURVE('',#8696,#8692,#1015,.T.);
#7344=EDGE_CURVE('',#8695,#8688,#1016,.T.);
#7345=EDGE_CURVE('',#8698,#8699,#9581,.T.);
#7346=EDGE_CURVE('',#8700,#8699,#9582,.T.);
#7347=EDGE_CURVE('',#8700,#8701,#9583,.T.);
#7348=EDGE_CURVE('',#8701,#8702,#9584,.T.);
#7349=EDGE_CURVE('',#8702,#8698,#9585,.T.);
#7350=EDGE_CURVE('',#8699,#8703,#1017,.T.);
#7351=EDGE_CURVE('',#8704,#8703,#9586,.T.);
#7352=EDGE_CURVE('',#8704,#8700,#1018,.T.);
#7353=EDGE_CURVE('',#8703,#8705,#9587,.T.);
#7354=EDGE_CURVE('',#8706,#8705,#9588,.T.);
#7355=EDGE_CURVE('',#8706,#8707,#9589,.T.);
#7356=EDGE_CURVE('',#8707,#8704,#9590,.T.);
#7357=EDGE_CURVE('',#8706,#8702,#1019,.T.);
#7358=EDGE_CURVE('',#8705,#8698,#1020,.T.);
#7359=EDGE_CURVE('',#8708,#8709,#9591,.T.);
#7360=EDGE_CURVE('',#8710,#8709,#9592,.T.);
#7361=EDGE_CURVE('',#8710,#8711,#9593,.T.);
#7362=EDGE_CURVE('',#8711,#8712,#9594,.T.);
#7363=EDGE_CURVE('',#8712,#8708,#9595,.T.);
#7364=EDGE_CURVE('',#8713,#8709,#1021,.T.);
#7365=EDGE_CURVE('',#8714,#8713,#9596,.T.);
#7366=EDGE_CURVE('',#8714,#8710,#1022,.T.);
#7367=EDGE_CURVE('',#8713,#8715,#9597,.T.);
#7368=EDGE_CURVE('',#8716,#8715,#9598,.T.);
#7369=EDGE_CURVE('',#8716,#8717,#9599,.T.);
#7370=EDGE_CURVE('',#8717,#8714,#9600,.T.);
#7371=EDGE_CURVE('',#8716,#8712,#1023,.T.);
#7372=EDGE_CURVE('',#8715,#8708,#1024,.T.);
#7373=EDGE_CURVE('',#8718,#8718,#1025,.T.);
#7374=EDGE_CURVE('',#8712,#8696,#1026,.T.);
#7375=EDGE_CURVE('',#8692,#8706,#1027,.T.);
#7376=EDGE_CURVE('',#8702,#8686,#1028,.T.);
#7377=EDGE_CURVE('',#8682,#8716,#1029,.T.);
#7378=EDGE_CURVE('',#8719,#8719,#1030,.T.);
#7379=EDGE_CURVE('',#8701,#8687,#1031,.T.);
#7380=EDGE_CURVE('',#8691,#8707,#1032,.T.);
#7381=EDGE_CURVE('',#8711,#8697,#1033,.T.);
#7382=EDGE_CURVE('',#8681,#8717,#1034,.T.);
#7383=EDGE_CURVE('',#8720,#8720,#1035,.T.);
#7384=EDGE_CURVE('',#8709,#8693,#1036,.T.);
#7385=EDGE_CURVE('',#8689,#8703,#1037,.T.);
#7386=EDGE_CURVE('',#8699,#8683,#1038,.T.);
#7387=EDGE_CURVE('',#8679,#8713,#1039,.T.);
#7388=EDGE_CURVE('',#8678,#8715,#1040,.T.);
#7389=EDGE_CURVE('',#8698,#8685,#1041,.T.);
#7390=EDGE_CURVE('',#8688,#8705,#1042,.T.);
#7391=EDGE_CURVE('',#8708,#8695,#1043,.T.);
#7392=EDGE_CURVE('',#8721,#8721,#1044,.T.);
#7393=EDGE_CURVE('',#8722,#8722,#1045,.T.);
#7394=EDGE_CURVE('',#8723,#8724,#1149,.F.);
#7395=EDGE_CURVE('',#8723,#8725,#1046,.T.);
#7396=EDGE_CURVE('',#8726,#8725,#1150,.T.);
#7397=EDGE_CURVE('',#8726,#8724,#1151,.F.);
#7398=EDGE_CURVE('',#8726,#8727,#1152,.T.);
#7399=EDGE_CURVE('',#8724,#8727,#1153,.F.);
#7400=EDGE_CURVE('',#8728,#8729,#1154,.F.);
#7401=EDGE_CURVE('',#8730,#8729,#1155,.F.);
#7402=EDGE_CURVE('',#8727,#8730,#1156,.F.);
#7403=EDGE_CURVE('',#8728,#8726,#1157,.T.);
#7404=EDGE_CURVE('',#8728,#8731,#1158,.T.);
#7405=EDGE_CURVE('',#8729,#8731,#1159,.F.);
#7406=EDGE_CURVE('',#8732,#8728,#1160,.T.);
#7407=EDGE_CURVE('',#8732,#8733,#1047,.T.);
#7408=EDGE_CURVE('',#8731,#8733,#1161,.F.);
#7409=EDGE_CURVE('',#8734,#8735,#1162,.T.);
#7410=EDGE_CURVE('',#8734,#8736,#1048,.T.);
#7411=EDGE_CURVE('',#8737,#8736,#1163,.F.);
#7412=EDGE_CURVE('',#8737,#8735,#1164,.F.);
#7413=EDGE_CURVE('',#8738,#8735,#1165,.T.);
#7414=EDGE_CURVE('',#8738,#8737,#1166,.F.);
#7415=EDGE_CURVE('',#8739,#8740,#1167,.F.);
#7416=EDGE_CURVE('',#8735,#8740,#1168,.T.);
#7417=EDGE_CURVE('',#8741,#8738,#1169,.F.);
#7418=EDGE_CURVE('',#8739,#8741,#1170,.F.);
#7419=EDGE_CURVE('',#8742,#8740,#1171,.T.);
#7420=EDGE_CURVE('',#8742,#8739,#1172,.F.);
#7421=EDGE_CURVE('',#8743,#8742,#1173,.F.);
#7422=EDGE_CURVE('',#8743,#8744,#1049,.T.);
#7423=EDGE_CURVE('',#8740,#8744,#1174,.T.);
#7424=EDGE_CURVE('',#8745,#8746,#1175,.T.);
#7425=EDGE_CURVE('',#8745,#8743,#1176,.T.);
#7426=EDGE_CURVE('',#8731,#8742,#1177,.F.);
#7427=EDGE_CURVE('',#8733,#8747,#1178,.T.);
#7428=EDGE_CURVE('',#8748,#8747,#1179,.T.);
#7429=EDGE_CURVE('',#8749,#8748,#1180,.T.);
#7430=EDGE_CURVE('',#8750,#8749,#1181,.T.);
#7431=EDGE_CURVE('',#8751,#8750,#1182,.T.);
#7432=EDGE_CURVE('',#8752,#8751,#1183,.T.);
#7433=EDGE_CURVE('',#8746,#8752,#1184,.T.);
#7434=EDGE_CURVE('',#8725,#8753,#1185,.T.);
#7435=EDGE_CURVE('',#8747,#8753,#1186,.F.);
#7436=EDGE_CURVE('',#8747,#8732,#1187,.T.);
#7437=EDGE_CURVE('',#8754,#8745,#1188,.F.);
#7438=EDGE_CURVE('',#8754,#8734,#1189,.T.);
#7439=EDGE_CURVE('',#8744,#8745,#1190,.T.);
#7440=EDGE_CURVE('',#8737,#8724,#1191,.F.);
#7441=EDGE_CURVE('',#8736,#8754,#1192,.T.);
#7442=EDGE_CURVE('',#8755,#8754,#1193,.T.);
#7443=EDGE_CURVE('',#8756,#8755,#1194,.T.);
#7444=EDGE_CURVE('',#8757,#8756,#1195,.T.);
#7445=EDGE_CURVE('',#8758,#8757,#1196,.T.);
#7446=EDGE_CURVE('',#8759,#8758,#1197,.T.);
#7447=EDGE_CURVE('',#8760,#8759,#1198,.T.);
#7448=EDGE_CURVE('',#8753,#8760,#1199,.T.);
#7449=EDGE_CURVE('',#8753,#8723,#1200,.T.);
#7450=EDGE_CURVE('',#8761,#8761,#1050,.T.);
#7451=EDGE_CURVE('',#8762,#8762,#1051,.T.);
#7452=EDGE_CURVE('',#8763,#8763,#1052,.T.);
#7453=EDGE_CURVE('',#8764,#8764,#1053,.T.);
#7454=EDGE_CURVE('',#8765,#8765,#1054,.T.);
#7455=EDGE_CURVE('',#8766,#8766,#1055,.T.);
#7456=EDGE_CURVE('',#8767,#8767,#1056,.T.);
#7457=EDGE_CURVE('',#8768,#8768,#1057,.T.);
#7458=EDGE_CURVE('',#8769,#8769,#1058,.T.);
#7459=EDGE_CURVE('',#8770,#8770,#1059,.T.);
#7460=EDGE_CURVE('',#8771,#8771,#1060,.T.);
#7461=EDGE_CURVE('',#8772,#8772,#1061,.T.);
#7462=VERTEX_POINT('',#19225);
#7463=VERTEX_POINT('',#19226);
#7464=VERTEX_POINT('',#19236);
#7465=VERTEX_POINT('',#19246);
#7466=VERTEX_POINT('',#19256);
#7467=VERTEX_POINT('',#19266);
#7468=VERTEX_POINT('',#19276);
#7469=VERTEX_POINT('',#19286);
#7470=VERTEX_POINT('',#19296);
#7471=VERTEX_POINT('',#19298);
#7472=VERTEX_POINT('',#19358);
#7473=VERTEX_POINT('',#19360);
#7474=VERTEX_POINT('',#19420);
#7475=VERTEX_POINT('',#19540);
#7476=VERTEX_POINT('',#19541);
#7477=VERTEX_POINT('',#19552);
#7478=VERTEX_POINT('',#19562);
#7479=VERTEX_POINT('',#19572);
#7480=VERTEX_POINT('',#19582);
#7481=VERTEX_POINT('',#19592);
#7482=VERTEX_POINT('',#19602);
#7483=VERTEX_POINT('',#19612);
#7484=VERTEX_POINT('',#19616);
#7485=VERTEX_POINT('',#19637);
#7486=VERTEX_POINT('',#19638);
#7487=VERTEX_POINT('',#19640);
#7488=VERTEX_POINT('',#19644);
#7489=VERTEX_POINT('',#19649);
#7490=VERTEX_POINT('',#19652);
#7491=VERTEX_POINT('',#19654);
#7492=VERTEX_POINT('',#19657);
#7493=VERTEX_POINT('',#19658);
#7494=VERTEX_POINT('',#19660);
#7495=VERTEX_POINT('',#19662);
#7496=VERTEX_POINT('',#19666);
#7497=VERTEX_POINT('',#19667);
#7498=VERTEX_POINT('',#19669);
#7499=VERTEX_POINT('',#19671);
#7500=VERTEX_POINT('',#19678);
#7501=VERTEX_POINT('',#19679);
#7502=VERTEX_POINT('',#19681);
#7503=VERTEX_POINT('',#19683);
#7504=VERTEX_POINT('',#19687);
#7505=VERTEX_POINT('',#19688);
#7506=VERTEX_POINT('',#19690);
#7507=VERTEX_POINT('',#19692);
#7508=VERTEX_POINT('',#19699);
#7509=VERTEX_POINT('',#19700);
#7510=VERTEX_POINT('',#19702);
#7511=VERTEX_POINT('',#19704);
#7512=VERTEX_POINT('',#19708);
#7513=VERTEX_POINT('',#19709);
#7514=VERTEX_POINT('',#19711);
#7515=VERTEX_POINT('',#19713);
#7516=VERTEX_POINT('',#19720);
#7517=VERTEX_POINT('',#19722);
#7518=VERTEX_POINT('',#19725);
#7519=VERTEX_POINT('',#19727);
#7520=VERTEX_POINT('',#19730);
#7521=VERTEX_POINT('',#19732);
#7522=VERTEX_POINT('',#19735);
#7523=VERTEX_POINT('',#19737);
#7524=VERTEX_POINT('',#19740);
#7525=VERTEX_POINT('',#19742);
#7526=VERTEX_POINT('',#19744);
#7527=VERTEX_POINT('',#19746);
#7528=VERTEX_POINT('',#19748);
#7529=VERTEX_POINT('',#19750);
#7530=VERTEX_POINT('',#19752);
#7531=VERTEX_POINT('',#19754);
#7532=VERTEX_POINT('',#19756);
#7533=VERTEX_POINT('',#19761);
#7534=VERTEX_POINT('',#19764);
#7535=VERTEX_POINT('',#19766);
#7536=VERTEX_POINT('',#19768);
#7537=VERTEX_POINT('',#19770);
#7538=VERTEX_POINT('',#19772);
#7539=VERTEX_POINT('',#19774);
#7540=VERTEX_POINT('',#19776);
#7541=VERTEX_POINT('',#19778);
#7542=VERTEX_POINT('',#19780);
#7543=VERTEX_POINT('',#19785);
#7544=VERTEX_POINT('',#19788);
#7545=VERTEX_POINT('',#19790);
#7546=VERTEX_POINT('',#19793);
#7547=VERTEX_POINT('',#19795);
#7548=VERTEX_POINT('',#19798);
#7549=VERTEX_POINT('',#19841);
#7550=VERTEX_POINT('',#19843);
#7551=VERTEX_POINT('',#19846);
#7552=VERTEX_POINT('',#19848);
#7553=VERTEX_POINT('',#19955);
#7554=VERTEX_POINT('',#19956);
#7555=VERTEX_POINT('',#19992);
#7556=VERTEX_POINT('',#19994);
#7557=VERTEX_POINT('',#19996);
#7558=VERTEX_POINT('',#20002);
#7559=VERTEX_POINT('',#20004);
#7560=VERTEX_POINT('',#20016);
#7561=VERTEX_POINT('',#20028);
#7562=VERTEX_POINT('',#20265);
#7563=VERTEX_POINT('',#20266);
#7564=VERTEX_POINT('',#20278);
#7565=VERTEX_POINT('',#20290);
#7566=VERTEX_POINT('',#20302);
#7567=VERTEX_POINT('',#20308);
#7568=VERTEX_POINT('',#20310);
#7569=VERTEX_POINT('',#20351);
#7570=VERTEX_POINT('',#20357);
#7571=VERTEX_POINT('',#20359);
#7572=VERTEX_POINT('',#20362);
#7573=VERTEX_POINT('',#20364);
#7574=VERTEX_POINT('',#20367);
#7575=VERTEX_POINT('',#20369);
#7576=VERTEX_POINT('',#20372);
#7577=VERTEX_POINT('',#20374);
#7578=VERTEX_POINT('',#20377);
#7579=VERTEX_POINT('',#20379);
#7580=VERTEX_POINT('',#20382);
#7581=VERTEX_POINT('',#20384);
#7582=VERTEX_POINT('',#20387);
#7583=VERTEX_POINT('',#20389);
#7584=VERTEX_POINT('',#20392);
#7585=VERTEX_POINT('',#20394);
#7586=VERTEX_POINT('',#20397);
#7587=VERTEX_POINT('',#20399);
#7588=VERTEX_POINT('',#20402);
#7589=VERTEX_POINT('',#20406);
#7590=VERTEX_POINT('',#20409);
#7591=VERTEX_POINT('',#20412);
#7592=VERTEX_POINT('',#20415);
#7593=VERTEX_POINT('',#20418);
#7594=VERTEX_POINT('',#20420);
#7595=VERTEX_POINT('',#20425);
#7596=VERTEX_POINT('',#20427);
#7597=VERTEX_POINT('',#20431);
#7598=VERTEX_POINT('',#20434);
#7599=VERTEX_POINT('',#20436);
#7600=VERTEX_POINT('',#20439);
#7601=VERTEX_POINT('',#20453);
#7602=VERTEX_POINT('',#20455);
#7603=VERTEX_POINT('',#20461);
#7604=VERTEX_POINT('',#20462);
#7605=VERTEX_POINT('',#20573);
#7606=VERTEX_POINT('',#20574);
#7607=VERTEX_POINT('',#21065);
#7608=VERTEX_POINT('',#21066);
#7609=VERTEX_POINT('',#22227);
#7610=VERTEX_POINT('',#22228);
#7611=VERTEX_POINT('',#22738);
#7612=VERTEX_POINT('',#22746);
#7613=VERTEX_POINT('',#24347);
#7614=VERTEX_POINT('',#24355);
#7615=VERTEX_POINT('',#24862);
#7616=VERTEX_POINT('',#24882);
#7617=VERTEX_POINT('',#27274);
#7618=VERTEX_POINT('',#27275);
#7619=VERTEX_POINT('',#27284);
#7620=VERTEX_POINT('',#27290);
#7621=VERTEX_POINT('',#27304);
#7622=VERTEX_POINT('',#27318);
#7623=VERTEX_POINT('',#27332);
#7624=VERTEX_POINT('',#27469);
#7625=VERTEX_POINT('',#27470);
#7626=VERTEX_POINT('',#27711);
#7627=VERTEX_POINT('',#27712);
#7628=VERTEX_POINT('',#27772);
#7629=VERTEX_POINT('',#27773);
#7630=VERTEX_POINT('',#28041);
#7631=VERTEX_POINT('',#28042);
#7632=VERTEX_POINT('',#28225);
#7633=VERTEX_POINT('',#28226);
#7634=VERTEX_POINT('',#28491);
#7635=VERTEX_POINT('',#28492);
#7636=VERTEX_POINT('',#28499);
#7637=VERTEX_POINT('',#28513);
#7638=VERTEX_POINT('',#28527);
#7639=VERTEX_POINT('',#28541);
#7640=VERTEX_POINT('',#28561);
#7641=VERTEX_POINT('',#28566);
#7642=VERTEX_POINT('',#28569);
#7643=VERTEX_POINT('',#30743);
#7644=VERTEX_POINT('',#30744);
#7645=VERTEX_POINT('',#30746);
#7646=VERTEX_POINT('',#30752);
#7647=VERTEX_POINT('',#30756);
#7648=VERTEX_POINT('',#30757);
#7649=VERTEX_POINT('',#30762);
#7650=VERTEX_POINT('',#30763);
#7651=VERTEX_POINT('',#30768);
#7652=VERTEX_POINT('',#30769);
#7653=VERTEX_POINT('',#30774);
#7654=VERTEX_POINT('',#30775);
#7655=VERTEX_POINT('',#30780);
#7656=VERTEX_POINT('',#30781);
#7657=VERTEX_POINT('',#30786);
#7658=VERTEX_POINT('',#30787);
#7659=VERTEX_POINT('',#30792);
#7660=VERTEX_POINT('',#30793);
#7661=VERTEX_POINT('',#30798);
#7662=VERTEX_POINT('',#30799);
#7663=VERTEX_POINT('',#30801);
#7664=VERTEX_POINT('',#30803);
#7665=VERTEX_POINT('',#30807);
#7666=VERTEX_POINT('',#30808);
#7667=VERTEX_POINT('',#30813);
#7668=VERTEX_POINT('',#30814);
#7669=VERTEX_POINT('',#30823);
#7670=VERTEX_POINT('',#30824);
#7671=VERTEX_POINT('',#30829);
#7672=VERTEX_POINT('',#30830);
#7673=VERTEX_POINT('',#30835);
#7674=VERTEX_POINT('',#30836);
#7675=VERTEX_POINT('',#30841);
#7676=VERTEX_POINT('',#30842);
#7677=VERTEX_POINT('',#30847);
#7678=VERTEX_POINT('',#30848);
#7679=VERTEX_POINT('',#30853);
#7680=VERTEX_POINT('',#30861);
#7681=VERTEX_POINT('',#30862);
#7682=VERTEX_POINT('',#30867);
#7683=VERTEX_POINT('',#30868);
#7684=VERTEX_POINT('',#30873);
#7685=VERTEX_POINT('',#30874);
#7686=VERTEX_POINT('',#30879);
#7687=VERTEX_POINT('',#30883);
#7688=VERTEX_POINT('',#30884);
#7689=VERTEX_POINT('',#30889);
#7690=VERTEX_POINT('',#30894);
#7691=VERTEX_POINT('',#30895);
#7692=VERTEX_POINT('',#30900);
#7693=VERTEX_POINT('',#30901);
#7694=VERTEX_POINT('',#30906);
#7695=VERTEX_POINT('',#30907);
#7696=VERTEX_POINT('',#30912);
#7697=VERTEX_POINT('',#30917);
#7698=VERTEX_POINT('',#30921);
#7699=VERTEX_POINT('',#30922);
#7700=VERTEX_POINT('',#30927);
#7701=VERTEX_POINT('',#30928);
#7702=VERTEX_POINT('',#30933);
#7703=VERTEX_POINT('',#30937);
#7704=VERTEX_POINT('',#30938);
#7705=VERTEX_POINT('',#30943);
#7706=VERTEX_POINT('',#30948);
#7707=VERTEX_POINT('',#30949);
#7708=VERTEX_POINT('',#30954);
#7709=VERTEX_POINT('',#30955);
#7710=VERTEX_POINT('',#30960);
#7711=VERTEX_POINT('',#30961);
#7712=VERTEX_POINT('',#30966);
#7713=VERTEX_POINT('',#30971);
#7714=VERTEX_POINT('',#30975);
#7715=VERTEX_POINT('',#30976);
#7716=VERTEX_POINT('',#30981);
#7717=VERTEX_POINT('',#30982);
#7718=VERTEX_POINT('',#30987);
#7719=VERTEX_POINT('',#30991);
#7720=VERTEX_POINT('',#30992);
#7721=VERTEX_POINT('',#30997);
#7722=VERTEX_POINT('',#31002);
#7723=VERTEX_POINT('',#31003);
#7724=VERTEX_POINT('',#31008);
#7725=VERTEX_POINT('',#31009);
#7726=VERTEX_POINT('',#31014);
#7727=VERTEX_POINT('',#31015);
#7728=VERTEX_POINT('',#31020);
#7729=VERTEX_POINT('',#31025);
#7730=VERTEX_POINT('',#31032);
#7731=VERTEX_POINT('',#31036);
#7732=VERTEX_POINT('',#31037);
#7733=VERTEX_POINT('',#31042);
#7734=VERTEX_POINT('',#31047);
#7735=VERTEX_POINT('',#31054);
#7736=VERTEX_POINT('',#31056);
#7737=VERTEX_POINT('',#31059);
#7738=VERTEX_POINT('',#31061);
#7739=VERTEX_POINT('',#31064);
#7740=VERTEX_POINT('',#31066);
#7741=VERTEX_POINT('',#31138);
#7742=VERTEX_POINT('',#31139);
#7743=VERTEX_POINT('',#31151);
#7744=VERTEX_POINT('',#31163);
#7745=VERTEX_POINT('',#31175);
#7746=VERTEX_POINT('',#31181);
#7747=VERTEX_POINT('',#31183);
#7748=VERTEX_POINT('',#31452);
#7749=VERTEX_POINT('',#31453);
#7750=VERTEX_POINT('',#31489);
#7751=VERTEX_POINT('',#31491);
#7752=VERTEX_POINT('',#31497);
#7753=VERTEX_POINT('',#31509);
#7754=VERTEX_POINT('',#31521);
#7755=VERTEX_POINT('',#31542);
#7756=VERTEX_POINT('',#31544);
#7757=VERTEX_POINT('',#31547);
#7758=VERTEX_POINT('',#31549);
#7759=VERTEX_POINT('',#31551);
#7760=VERTEX_POINT('',#31554);
#7761=VERTEX_POINT('',#31572);
#7762=VERTEX_POINT('',#31574);
#7763=VERTEX_POINT('',#31576);
#7764=VERTEX_POINT('',#31590);
#7765=VERTEX_POINT('',#31595);
#7766=VERTEX_POINT('',#31596);
#7767=VERTEX_POINT('',#31598);
#7768=VERTEX_POINT('',#31600);
#7769=VERTEX_POINT('',#31604);
#7770=VERTEX_POINT('',#31608);
#7771=VERTEX_POINT('',#31612);
#7772=VERTEX_POINT('',#31613);
#7773=VERTEX_POINT('',#31615);
#7774=VERTEX_POINT('',#31617);
#7775=VERTEX_POINT('',#31621);
#7776=VERTEX_POINT('',#31625);
#7777=VERTEX_POINT('',#31629);
#7778=VERTEX_POINT('',#31631);
#7779=VERTEX_POINT('',#31636);
#7780=VERTEX_POINT('',#31637);
#7781=VERTEX_POINT('',#31644);
#7782=VERTEX_POINT('',#31646);
#7783=VERTEX_POINT('',#31649);
#7784=VERTEX_POINT('',#31660);
#7785=VERTEX_POINT('',#31667);
#7786=VERTEX_POINT('',#31669);
#7787=VERTEX_POINT('',#31672);
#7788=VERTEX_POINT('',#31674);
#7789=VERTEX_POINT('',#31678);
#7790=VERTEX_POINT('',#31680);
#7791=VERTEX_POINT('',#31683);
#7792=VERTEX_POINT('',#31684);
#7793=VERTEX_POINT('',#31690);
#7794=VERTEX_POINT('',#31692);
#7795=VERTEX_POINT('',#31695);
#7796=VERTEX_POINT('',#31697);
#7797=VERTEX_POINT('',#31700);
#7798=VERTEX_POINT('',#31702);
#7799=VERTEX_POINT('',#31705);
#7800=VERTEX_POINT('',#31707);
#7801=VERTEX_POINT('',#31710);
#7802=VERTEX_POINT('',#31712);
#7803=VERTEX_POINT('',#31715);
#7804=VERTEX_POINT('',#31967);
#7805=VERTEX_POINT('',#31968);
#7806=VERTEX_POINT('',#32030);
#7807=VERTEX_POINT('',#32032);
#7808=VERTEX_POINT('',#32046);
#7809=VERTEX_POINT('',#32060);
#7810=VERTEX_POINT('',#32074);
#7811=VERTEX_POINT('',#32088);
#7812=VERTEX_POINT('',#32283);
#7813=VERTEX_POINT('',#32284);
#7814=VERTEX_POINT('',#32289);
#7815=VERTEX_POINT('',#32583);
#7816=VERTEX_POINT('',#32584);
#7817=VERTEX_POINT('',#32645);
#7818=VERTEX_POINT('',#32646);
#7819=VERTEX_POINT('',#32651);
#7820=VERTEX_POINT('',#32652);
#7821=VERTEX_POINT('',#32654);
#7822=VERTEX_POINT('',#32659);
#7823=VERTEX_POINT('',#32660);
#7824=VERTEX_POINT('',#32662);
#7825=VERTEX_POINT('',#32670);
#7826=VERTEX_POINT('',#32935);
#7827=VERTEX_POINT('',#33095);
#7828=VERTEX_POINT('',#33317);
#7829=VERTEX_POINT('',#33331);
#7830=VERTEX_POINT('',#33345);
#7831=VERTEX_POINT('',#33358);
#7832=VERTEX_POINT('',#33359);
#7833=VERTEX_POINT('',#33361);
#7834=VERTEX_POINT('',#33366);
#7835=VERTEX_POINT('',#33368);
#7836=VERTEX_POINT('',#33403);
#7837=VERTEX_POINT('',#33412);
#7838=VERTEX_POINT('',#33445);
#7839=VERTEX_POINT('',#33475);
#7840=VERTEX_POINT('',#33478);
#7841=VERTEX_POINT('',#33482);
#7842=VERTEX_POINT('',#33485);
#7843=VERTEX_POINT('',#33488);
#7844=VERTEX_POINT('',#33490);
#7845=VERTEX_POINT('',#33498);
#7846=VERTEX_POINT('',#33500);
#7847=VERTEX_POINT('',#33503);
#7848=VERTEX_POINT('',#33505);
#7849=VERTEX_POINT('',#33508);
#7850=VERTEX_POINT('',#33510);
#7851=VERTEX_POINT('',#33513);
#7852=VERTEX_POINT('',#33515);
#7853=VERTEX_POINT('',#33518);
#7854=VERTEX_POINT('',#33520);
#7855=VERTEX_POINT('',#33523);
#7856=VERTEX_POINT('',#33526);
#7857=VERTEX_POINT('',#33529);
#7858=VERTEX_POINT('',#33532);
#7859=VERTEX_POINT('',#33535);
#7860=VERTEX_POINT('',#33539);
#7861=VERTEX_POINT('',#33542);
#7862=VERTEX_POINT('',#33544);
#7863=VERTEX_POINT('',#33547);
#7864=VERTEX_POINT('',#33549);
#7865=VERTEX_POINT('',#33552);
#7866=VERTEX_POINT('',#33555);
#7867=VERTEX_POINT('',#33565);
#7868=VERTEX_POINT('',#33567);
#7869=VERTEX_POINT('',#33687);
#7870=VERTEX_POINT('',#33688);
#7871=VERTEX_POINT('',#33698);
#7872=VERTEX_POINT('',#33708);
#7873=VERTEX_POINT('',#33718);
#7874=VERTEX_POINT('',#33728);
#7875=VERTEX_POINT('',#33738);
#7876=VERTEX_POINT('',#33748);
#7877=VERTEX_POINT('',#33754);
#7878=VERTEX_POINT('',#33756);
#7879=VERTEX_POINT('',#33814);
#7880=VERTEX_POINT('',#33931);
#7881=VERTEX_POINT('',#33932);
#7882=VERTEX_POINT('',#33938);
#7883=VERTEX_POINT('',#33948);
#7884=VERTEX_POINT('',#33958);
#7885=VERTEX_POINT('',#33968);
#7886=VERTEX_POINT('',#33978);
#7887=VERTEX_POINT('',#33988);
#7888=VERTEX_POINT('',#33998);
#7889=VERTEX_POINT('',#34004);
#7890=VERTEX_POINT('',#34006);
#7891=VERTEX_POINT('',#34069);
#7892=VERTEX_POINT('',#34076);
#7893=VERTEX_POINT('',#34079);
#7894=VERTEX_POINT('',#34080);
#7895=VERTEX_POINT('',#34082);
#7896=VERTEX_POINT('',#34084);
#7897=VERTEX_POINT('',#34086);
#7898=VERTEX_POINT('',#34088);
#7899=VERTEX_POINT('',#34090);
#7900=VERTEX_POINT('',#34092);
#7901=VERTEX_POINT('',#34094);
#7902=VERTEX_POINT('',#34096);
#7903=VERTEX_POINT('',#34098);
#7904=VERTEX_POINT('',#34100);
#7905=VERTEX_POINT('',#34102);
#7906=VERTEX_POINT('',#34104);
#7907=VERTEX_POINT('',#34106);
#7908=VERTEX_POINT('',#34108);
#7909=VERTEX_POINT('',#34110);
#7910=VERTEX_POINT('',#34112);
#7911=VERTEX_POINT('',#34114);
#7912=VERTEX_POINT('',#34116);
#7913=VERTEX_POINT('',#34118);
#7914=VERTEX_POINT('',#34120);
#7915=VERTEX_POINT('',#34122);
#7916=VERTEX_POINT('',#34124);
#7917=VERTEX_POINT('',#34126);
#7918=VERTEX_POINT('',#34128);
#7919=VERTEX_POINT('',#34130);
#7920=VERTEX_POINT('',#34132);
#7921=VERTEX_POINT('',#34134);
#7922=VERTEX_POINT('',#34136);
#7923=VERTEX_POINT('',#34138);
#7924=VERTEX_POINT('',#34140);
#7925=VERTEX_POINT('',#34142);
#7926=VERTEX_POINT('',#34144);
#7927=VERTEX_POINT('',#34146);
#7928=VERTEX_POINT('',#34148);
#7929=VERTEX_POINT('',#34150);
#7930=VERTEX_POINT('',#34152);
#7931=VERTEX_POINT('',#34154);
#7932=VERTEX_POINT('',#34156);
#7933=VERTEX_POINT('',#34158);
#7934=VERTEX_POINT('',#34160);
#7935=VERTEX_POINT('',#34162);
#7936=VERTEX_POINT('',#34164);
#7937=VERTEX_POINT('',#34166);
#7938=VERTEX_POINT('',#34168);
#7939=VERTEX_POINT('',#34170);
#7940=VERTEX_POINT('',#34172);
#7941=VERTEX_POINT('',#34174);
#7942=VERTEX_POINT('',#34176);
#7943=VERTEX_POINT('',#34178);
#7944=VERTEX_POINT('',#34180);
#7945=VERTEX_POINT('',#34182);
#7946=VERTEX_POINT('',#34184);
#7947=VERTEX_POINT('',#34186);
#7948=VERTEX_POINT('',#34188);
#7949=VERTEX_POINT('',#34190);
#7950=VERTEX_POINT('',#34192);
#7951=VERTEX_POINT('',#34194);
#7952=VERTEX_POINT('',#34196);
#7953=VERTEX_POINT('',#34198);
#7954=VERTEX_POINT('',#34200);
#7955=VERTEX_POINT('',#34202);
#7956=VERTEX_POINT('',#34204);
#7957=VERTEX_POINT('',#34206);
#7958=VERTEX_POINT('',#34208);
#7959=VERTEX_POINT('',#34210);
#7960=VERTEX_POINT('',#34212);
#7961=VERTEX_POINT('',#34214);
#7962=VERTEX_POINT('',#34216);
#7963=VERTEX_POINT('',#34218);
#7964=VERTEX_POINT('',#34220);
#7965=VERTEX_POINT('',#34222);
#7966=VERTEX_POINT('',#34224);
#7967=VERTEX_POINT('',#34226);
#7968=VERTEX_POINT('',#34228);
#7969=VERTEX_POINT('',#34230);
#7970=VERTEX_POINT('',#34232);
#7971=VERTEX_POINT('',#34234);
#7972=VERTEX_POINT('',#34236);
#7973=VERTEX_POINT('',#34238);
#7974=VERTEX_POINT('',#34240);
#7975=VERTEX_POINT('',#34242);
#7976=VERTEX_POINT('',#34244);
#7977=VERTEX_POINT('',#34246);
#7978=VERTEX_POINT('',#34248);
#7979=VERTEX_POINT('',#34250);
#7980=VERTEX_POINT('',#34252);
#7981=VERTEX_POINT('',#34254);
#7982=VERTEX_POINT('',#34256);
#7983=VERTEX_POINT('',#34258);
#7984=VERTEX_POINT('',#34260);
#7985=VERTEX_POINT('',#34262);
#7986=VERTEX_POINT('',#34264);
#7987=VERTEX_POINT('',#34266);
#7988=VERTEX_POINT('',#34268);
#7989=VERTEX_POINT('',#34270);
#7990=VERTEX_POINT('',#34272);
#7991=VERTEX_POINT('',#34274);
#7992=VERTEX_POINT('',#34276);
#7993=VERTEX_POINT('',#34278);
#7994=VERTEX_POINT('',#34280);
#7995=VERTEX_POINT('',#34282);
#7996=VERTEX_POINT('',#34284);
#7997=VERTEX_POINT('',#34286);
#7998=VERTEX_POINT('',#34288);
#7999=VERTEX_POINT('',#34290);
#8000=VERTEX_POINT('',#34292);
#8001=VERTEX_POINT('',#34294);
#8002=VERTEX_POINT('',#34296);
#8003=VERTEX_POINT('',#34298);
#8004=VERTEX_POINT('',#34300);
#8005=VERTEX_POINT('',#34302);
#8006=VERTEX_POINT('',#34304);
#8007=VERTEX_POINT('',#34306);
#8008=VERTEX_POINT('',#34308);
#8009=VERTEX_POINT('',#34310);
#8010=VERTEX_POINT('',#34312);
#8011=VERTEX_POINT('',#34314);
#8012=VERTEX_POINT('',#34316);
#8013=VERTEX_POINT('',#34318);
#8014=VERTEX_POINT('',#34320);
#8015=VERTEX_POINT('',#34322);
#8016=VERTEX_POINT('',#34324);
#8017=VERTEX_POINT('',#34326);
#8018=VERTEX_POINT('',#34328);
#8019=VERTEX_POINT('',#34330);
#8020=VERTEX_POINT('',#34332);
#8021=VERTEX_POINT('',#34334);
#8022=VERTEX_POINT('',#34336);
#8023=VERTEX_POINT('',#34338);
#8024=VERTEX_POINT('',#34340);
#8025=VERTEX_POINT('',#34342);
#8026=VERTEX_POINT('',#34344);
#8027=VERTEX_POINT('',#34346);
#8028=VERTEX_POINT('',#34348);
#8029=VERTEX_POINT('',#34350);
#8030=VERTEX_POINT('',#34352);
#8031=VERTEX_POINT('',#34354);
#8032=VERTEX_POINT('',#34356);
#8033=VERTEX_POINT('',#34358);
#8034=VERTEX_POINT('',#34360);
#8035=VERTEX_POINT('',#34362);
#8036=VERTEX_POINT('',#34365);
#8037=VERTEX_POINT('',#34368);
#8038=VERTEX_POINT('',#34369);
#8039=VERTEX_POINT('',#34371);
#8040=VERTEX_POINT('',#34373);
#8041=VERTEX_POINT('',#34375);
#8042=VERTEX_POINT('',#34377);
#8043=VERTEX_POINT('',#34379);
#8044=VERTEX_POINT('',#34381);
#8045=VERTEX_POINT('',#34383);
#8046=VERTEX_POINT('',#34385);
#8047=VERTEX_POINT('',#34387);
#8048=VERTEX_POINT('',#34389);
#8049=VERTEX_POINT('',#34391);
#8050=VERTEX_POINT('',#34393);
#8051=VERTEX_POINT('',#34395);
#8052=VERTEX_POINT('',#34397);
#8053=VERTEX_POINT('',#34399);
#8054=VERTEX_POINT('',#34401);
#8055=VERTEX_POINT('',#34403);
#8056=VERTEX_POINT('',#34405);
#8057=VERTEX_POINT('',#34407);
#8058=VERTEX_POINT('',#34409);
#8059=VERTEX_POINT('',#34411);
#8060=VERTEX_POINT('',#34413);
#8061=VERTEX_POINT('',#34415);
#8062=VERTEX_POINT('',#34417);
#8063=VERTEX_POINT('',#34419);
#8064=VERTEX_POINT('',#34421);
#8065=VERTEX_POINT('',#34423);
#8066=VERTEX_POINT('',#34425);
#8067=VERTEX_POINT('',#34427);
#8068=VERTEX_POINT('',#34429);
#8069=VERTEX_POINT('',#34431);
#8070=VERTEX_POINT('',#34433);
#8071=VERTEX_POINT('',#34435);
#8072=VERTEX_POINT('',#34437);
#8073=VERTEX_POINT('',#34439);
#8074=VERTEX_POINT('',#34441);
#8075=VERTEX_POINT('',#34443);
#8076=VERTEX_POINT('',#34445);
#8077=VERTEX_POINT('',#34447);
#8078=VERTEX_POINT('',#34449);
#8079=VERTEX_POINT('',#34451);
#8080=VERTEX_POINT('',#34453);
#8081=VERTEX_POINT('',#34455);
#8082=VERTEX_POINT('',#34457);
#8083=VERTEX_POINT('',#34459);
#8084=VERTEX_POINT('',#34461);
#8085=VERTEX_POINT('',#34463);
#8086=VERTEX_POINT('',#34465);
#8087=VERTEX_POINT('',#34467);
#8088=VERTEX_POINT('',#34469);
#8089=VERTEX_POINT('',#34471);
#8090=VERTEX_POINT('',#34473);
#8091=VERTEX_POINT('',#34475);
#8092=VERTEX_POINT('',#34477);
#8093=VERTEX_POINT('',#34479);
#8094=VERTEX_POINT('',#34481);
#8095=VERTEX_POINT('',#34483);
#8096=VERTEX_POINT('',#34485);
#8097=VERTEX_POINT('',#34487);
#8098=VERTEX_POINT('',#34489);
#8099=VERTEX_POINT('',#34491);
#8100=VERTEX_POINT('',#34493);
#8101=VERTEX_POINT('',#34495);
#8102=VERTEX_POINT('',#34497);
#8103=VERTEX_POINT('',#34499);
#8104=VERTEX_POINT('',#34501);
#8105=VERTEX_POINT('',#34503);
#8106=VERTEX_POINT('',#34505);
#8107=VERTEX_POINT('',#34507);
#8108=VERTEX_POINT('',#34509);
#8109=VERTEX_POINT('',#34511);
#8110=VERTEX_POINT('',#34513);
#8111=VERTEX_POINT('',#34515);
#8112=VERTEX_POINT('',#34517);
#8113=VERTEX_POINT('',#34519);
#8114=VERTEX_POINT('',#34521);
#8115=VERTEX_POINT('',#34523);
#8116=VERTEX_POINT('',#34525);
#8117=VERTEX_POINT('',#34527);
#8118=VERTEX_POINT('',#34529);
#8119=VERTEX_POINT('',#34531);
#8120=VERTEX_POINT('',#34533);
#8121=VERTEX_POINT('',#34535);
#8122=VERTEX_POINT('',#34537);
#8123=VERTEX_POINT('',#34539);
#8124=VERTEX_POINT('',#34541);
#8125=VERTEX_POINT('',#34543);
#8126=VERTEX_POINT('',#34545);
#8127=VERTEX_POINT('',#34547);
#8128=VERTEX_POINT('',#34549);
#8129=VERTEX_POINT('',#34551);
#8130=VERTEX_POINT('',#34553);
#8131=VERTEX_POINT('',#34555);
#8132=VERTEX_POINT('',#34557);
#8133=VERTEX_POINT('',#34559);
#8134=VERTEX_POINT('',#34561);
#8135=VERTEX_POINT('',#34563);
#8136=VERTEX_POINT('',#34565);
#8137=VERTEX_POINT('',#34567);
#8138=VERTEX_POINT('',#34569);
#8139=VERTEX_POINT('',#34571);
#8140=VERTEX_POINT('',#34573);
#8141=VERTEX_POINT('',#34575);
#8142=VERTEX_POINT('',#34577);
#8143=VERTEX_POINT('',#34579);
#8144=VERTEX_POINT('',#34581);
#8145=VERTEX_POINT('',#34583);
#8146=VERTEX_POINT('',#34585);
#8147=VERTEX_POINT('',#34587);
#8148=VERTEX_POINT('',#34589);
#8149=VERTEX_POINT('',#34591);
#8150=VERTEX_POINT('',#34593);
#8151=VERTEX_POINT('',#34595);
#8152=VERTEX_POINT('',#34597);
#8153=VERTEX_POINT('',#34599);
#8154=VERTEX_POINT('',#34601);
#8155=VERTEX_POINT('',#34603);
#8156=VERTEX_POINT('',#34605);
#8157=VERTEX_POINT('',#34607);
#8158=VERTEX_POINT('',#34609);
#8159=VERTEX_POINT('',#34611);
#8160=VERTEX_POINT('',#34613);
#8161=VERTEX_POINT('',#34615);
#8162=VERTEX_POINT('',#34617);
#8163=VERTEX_POINT('',#34619);
#8164=VERTEX_POINT('',#34621);
#8165=VERTEX_POINT('',#34623);
#8166=VERTEX_POINT('',#34625);
#8167=VERTEX_POINT('',#34627);
#8168=VERTEX_POINT('',#34629);
#8169=VERTEX_POINT('',#34631);
#8170=VERTEX_POINT('',#34633);
#8171=VERTEX_POINT('',#34635);
#8172=VERTEX_POINT('',#34637);
#8173=VERTEX_POINT('',#34639);
#8174=VERTEX_POINT('',#34641);
#8175=VERTEX_POINT('',#34643);
#8176=VERTEX_POINT('',#34645);
#8177=VERTEX_POINT('',#34647);
#8178=VERTEX_POINT('',#34649);
#8179=VERTEX_POINT('',#34651);
#8180=VERTEX_POINT('',#34654);
#8181=VERTEX_POINT('',#34944);
#8182=VERTEX_POINT('',#34949);
#8183=VERTEX_POINT('',#34952);
#8184=VERTEX_POINT('',#34958);
#8185=VERTEX_POINT('',#34960);
#8186=VERTEX_POINT('',#34963);
#8187=VERTEX_POINT('',#34965);
#8188=VERTEX_POINT('',#34971);
#8189=VERTEX_POINT('',#34973);
#8190=VERTEX_POINT('',#34976);
#8191=VERTEX_POINT('',#34978);
#8192=VERTEX_POINT('',#34985);
#8193=VERTEX_POINT('',#34986);
#8194=VERTEX_POINT('',#34988);
#8195=VERTEX_POINT('',#34990);
#8196=VERTEX_POINT('',#34994);
#8197=VERTEX_POINT('',#34995);
#8198=VERTEX_POINT('',#35000);
#8199=VERTEX_POINT('',#35001);
#8200=VERTEX_POINT('',#35006);
#8201=VERTEX_POINT('',#35007);
#8202=VERTEX_POINT('',#35009);
#8203=VERTEX_POINT('',#35011);
#8204=VERTEX_POINT('',#35015);
#8205=VERTEX_POINT('',#35016);
#8206=VERTEX_POINT('',#35021);
#8207=VERTEX_POINT('',#35022);
#8208=VERTEX_POINT('',#35027);
#8209=VERTEX_POINT('',#35030);
#8210=VERTEX_POINT('',#35035);
#8211=VERTEX_POINT('',#35037);
#8212=VERTEX_POINT('',#35048);
#8213=VERTEX_POINT('',#35052);
#8214=VERTEX_POINT('',#35053);
#8215=VERTEX_POINT('',#35055);
#8216=VERTEX_POINT('',#35057);
#8217=VERTEX_POINT('',#35061);
#8218=VERTEX_POINT('',#35063);
#8219=VERTEX_POINT('',#35067);
#8220=VERTEX_POINT('',#35069);
#8221=VERTEX_POINT('',#35073);
#8222=VERTEX_POINT('',#35074);
#8223=VERTEX_POINT('',#35076);
#8224=VERTEX_POINT('',#35078);
#8225=VERTEX_POINT('',#35082);
#8226=VERTEX_POINT('',#35083);
#8227=VERTEX_POINT('',#35085);
#8228=VERTEX_POINT('',#35087);
#8229=VERTEX_POINT('',#35094);
#8230=VERTEX_POINT('',#35095);
#8231=VERTEX_POINT('',#35097);
#8232=VERTEX_POINT('',#35099);
#8233=VERTEX_POINT('',#35103);
#8234=VERTEX_POINT('',#35104);
#8235=VERTEX_POINT('',#35106);
#8236=VERTEX_POINT('',#35108);
#8237=VERTEX_POINT('',#35115);
#8238=VERTEX_POINT('',#35117);
#8239=VERTEX_POINT('',#35120);
#8240=VERTEX_POINT('',#35122);
#8241=VERTEX_POINT('',#35125);
#8242=VERTEX_POINT('',#35127);
#8243=VERTEX_POINT('',#35130);
#8244=VERTEX_POINT('',#35132);
#8245=VERTEX_POINT('',#35134);
#8246=VERTEX_POINT('',#35139);
#8247=VERTEX_POINT('',#35141);
#8248=VERTEX_POINT('',#35144);
#8249=VERTEX_POINT('',#35146);
#8250=VERTEX_POINT('',#35148);
#8251=VERTEX_POINT('',#35153);
#8252=VERTEX_POINT('',#35155);
#8253=VERTEX_POINT('',#35158);
#8254=VERTEX_POINT('',#35160);
#8255=VERTEX_POINT('',#35163);
#8256=VERTEX_POINT('',#35165);
#8257=VERTEX_POINT('',#35181);
#8258=VERTEX_POINT('',#35187);
#8259=VERTEX_POINT('',#35188);
#8260=VERTEX_POINT('',#35190);
#8261=VERTEX_POINT('',#35192);
#8262=VERTEX_POINT('',#35196);
#8263=VERTEX_POINT('',#35198);
#8264=VERTEX_POINT('',#35202);
#8265=VERTEX_POINT('',#35204);
#8266=VERTEX_POINT('',#35210);
#8267=VERTEX_POINT('',#35211);
#8268=VERTEX_POINT('',#35213);
#8269=VERTEX_POINT('',#35215);
#8270=VERTEX_POINT('',#35219);
#8271=VERTEX_POINT('',#35221);
#8272=VERTEX_POINT('',#35225);
#8273=VERTEX_POINT('',#35227);
#8274=VERTEX_POINT('',#35233);
#8275=VERTEX_POINT('',#35234);
#8276=VERTEX_POINT('',#35236);
#8277=VERTEX_POINT('',#35238);
#8278=VERTEX_POINT('',#35242);
#8279=VERTEX_POINT('',#35244);
#8280=VERTEX_POINT('',#35248);
#8281=VERTEX_POINT('',#35250);
#8282=VERTEX_POINT('',#35256);
#8283=VERTEX_POINT('',#35258);
#8284=VERTEX_POINT('',#35264);
#8285=VERTEX_POINT('',#35266);
#8286=VERTEX_POINT('',#35275);
#8287=VERTEX_POINT('',#35276);
#8288=VERTEX_POINT('',#35278);
#8289=VERTEX_POINT('',#35280);
#8290=VERTEX_POINT('',#35284);
#8291=VERTEX_POINT('',#35285);
#8292=VERTEX_POINT('',#35287);
#8293=VERTEX_POINT('',#35289);
#8294=VERTEX_POINT('',#35293);
#8295=VERTEX_POINT('',#35294);
#8296=VERTEX_POINT('',#35296);
#8297=VERTEX_POINT('',#35298);
#8298=VERTEX_POINT('',#35302);
#8299=VERTEX_POINT('',#35303);
#8300=VERTEX_POINT('',#35305);
#8301=VERTEX_POINT('',#35307);
#8302=VERTEX_POINT('',#35311);
#8303=VERTEX_POINT('',#35312);
#8304=VERTEX_POINT('',#35314);
#8305=VERTEX_POINT('',#35316);
#8306=VERTEX_POINT('',#35320);
#8307=VERTEX_POINT('',#35321);
#8308=VERTEX_POINT('',#35326);
#8309=VERTEX_POINT('',#35327);
#8310=VERTEX_POINT('',#35332);
#8311=VERTEX_POINT('',#35333);
#8312=VERTEX_POINT('',#35335);
#8313=VERTEX_POINT('',#35337);
#8314=VERTEX_POINT('',#35341);
#8315=VERTEX_POINT('',#35342);
#8316=VERTEX_POINT('',#35347);
#8317=VERTEX_POINT('',#35348);
#8318=VERTEX_POINT('',#35358);
#8319=VERTEX_POINT('',#35379);
#8320=VERTEX_POINT('',#35381);
#8321=VERTEX_POINT('',#35384);
#8322=VERTEX_POINT('',#35385);
#8323=VERTEX_POINT('',#35387);
#8324=VERTEX_POINT('',#35389);
#8325=VERTEX_POINT('',#35393);
#8326=VERTEX_POINT('',#35395);
#8327=VERTEX_POINT('',#35396);
#8328=VERTEX_POINT('',#35398);
#8329=VERTEX_POINT('',#35400);
#8330=VERTEX_POINT('',#35402);
#8331=VERTEX_POINT('',#35404);
#8332=VERTEX_POINT('',#35409);
#8333=VERTEX_POINT('',#35410);
#8334=VERTEX_POINT('',#35415);
#8335=VERTEX_POINT('',#35417);
#8336=VERTEX_POINT('',#35418);
#8337=VERTEX_POINT('',#35422);
#8338=VERTEX_POINT('',#35424);
#8339=VERTEX_POINT('',#35428);
#8340=VERTEX_POINT('',#35430);
#8341=VERTEX_POINT('',#35431);
#8342=VERTEX_POINT('',#35433);
#8343=VERTEX_POINT('',#35435);
#8344=VERTEX_POINT('',#35437);
#8345=VERTEX_POINT('',#35439);
#8346=VERTEX_POINT('',#35441);
#8347=VERTEX_POINT('',#35443);
#8348=VERTEX_POINT('',#35447);
#8349=VERTEX_POINT('',#35448);
#8350=VERTEX_POINT('',#35453);
#8351=VERTEX_POINT('',#35455);
#8352=VERTEX_POINT('',#35456);
#8353=VERTEX_POINT('',#35458);
#8354=VERTEX_POINT('',#35460);
#8355=VERTEX_POINT('',#35463);
#8356=VERTEX_POINT('',#35465);
#8357=VERTEX_POINT('',#35472);
#8358=VERTEX_POINT('',#35474);
#8359=VERTEX_POINT('',#35475);
#8360=VERTEX_POINT('',#35477);
#8361=VERTEX_POINT('',#35479);
#8362=VERTEX_POINT('',#35481);
#8363=VERTEX_POINT('',#35483);
#8364=VERTEX_POINT('',#35485);
#8365=VERTEX_POINT('',#35487);
#8366=VERTEX_POINT('',#35491);
#8367=VERTEX_POINT('',#35493);
#8368=VERTEX_POINT('',#35494);
#8369=VERTEX_POINT('',#35496);
#8370=VERTEX_POINT('',#35498);
#8371=VERTEX_POINT('',#35500);
#8372=VERTEX_POINT('',#35502);
#8373=VERTEX_POINT('',#35504);
#8374=VERTEX_POINT('',#35506);
#8375=VERTEX_POINT('',#35510);
#8376=VERTEX_POINT('',#35512);
#8377=VERTEX_POINT('',#35513);
#8378=VERTEX_POINT('',#35515);
#8379=VERTEX_POINT('',#35517);
#8380=VERTEX_POINT('',#35519);
#8381=VERTEX_POINT('',#35521);
#8382=VERTEX_POINT('',#35523);
#8383=VERTEX_POINT('',#35525);
#8384=VERTEX_POINT('',#35529);
#8385=VERTEX_POINT('',#35530);
#8386=VERTEX_POINT('',#35535);
#8387=VERTEX_POINT('',#35537);
#8388=VERTEX_POINT('',#35538);
#8389=VERTEX_POINT('',#35540);
#8390=VERTEX_POINT('',#35542);
#8391=VERTEX_POINT('',#35545);
#8392=VERTEX_POINT('',#35547);
#8393=VERTEX_POINT('',#35592);
#8394=VERTEX_POINT('',#35724);
#8395=VERTEX_POINT('',#35725);
#8396=VERTEX_POINT('',#35735);
#8397=VERTEX_POINT('',#35745);
#8398=VERTEX_POINT('',#35755);
#8399=VERTEX_POINT('',#35765);
#8400=VERTEX_POINT('',#35775);
#8401=VERTEX_POINT('',#35785);
#8402=VERTEX_POINT('',#35795);
#8403=VERTEX_POINT('',#35805);
#8404=VERTEX_POINT('',#35807);
#8405=VERTEX_POINT('',#36004);
#8406=VERTEX_POINT('',#36005);
#8407=VERTEX_POINT('',#36071);
#8408=VERTEX_POINT('',#36073);
#8409=VERTEX_POINT('',#36083);
#8410=VERTEX_POINT('',#36093);
#8411=VERTEX_POINT('',#36103);
#8412=VERTEX_POINT('',#36113);
#8413=VERTEX_POINT('',#36123);
#8414=VERTEX_POINT('',#36133);
#8415=VERTEX_POINT('',#36143);
#8416=VERTEX_POINT('',#36163);
#8417=VERTEX_POINT('',#37218);
#8418=VERTEX_POINT('',#37219);
#8419=VERTEX_POINT('',#37334);
#8420=VERTEX_POINT('',#37339);
#8421=VERTEX_POINT('',#37345);
#8422=VERTEX_POINT('',#37351);
#8423=VERTEX_POINT('',#37363);
#8424=VERTEX_POINT('',#37375);
#8425=VERTEX_POINT('',#37387);
#8426=VERTEX_POINT('',#37399);
#8427=VERTEX_POINT('',#37411);
#8428=VERTEX_POINT('',#37419);
#8429=VERTEX_POINT('',#37431);
#8430=VERTEX_POINT('',#37432);
#8431=VERTEX_POINT('',#37441);
#8432=VERTEX_POINT('',#37446);
#8433=VERTEX_POINT('',#37453);
#8434=VERTEX_POINT('',#37454);
#8435=VERTEX_POINT('',#37463);
#8436=VERTEX_POINT('',#37468);
#8437=VERTEX_POINT('',#37473);
#8438=VERTEX_POINT('',#38517);
#8439=VERTEX_POINT('',#38518);
#8440=VERTEX_POINT('',#38526);
#8441=VERTEX_POINT('',#38538);
#8442=VERTEX_POINT('',#38550);
#8443=VERTEX_POINT('',#38562);
#8444=VERTEX_POINT('',#38574);
#8445=VERTEX_POINT('',#38586);
#8446=VERTEX_POINT('',#38596);
#8447=VERTEX_POINT('',#38723);
#8448=VERTEX_POINT('',#38775);
#8449=VERTEX_POINT('',#38778);
#8450=VERTEX_POINT('',#38780);
#8451=VERTEX_POINT('',#38783);
#8452=VERTEX_POINT('',#38784);
#8453=VERTEX_POINT('',#38787);
#8454=VERTEX_POINT('',#38790);
#8455=VERTEX_POINT('',#38791);
#8456=VERTEX_POINT('',#38794);
#8457=VERTEX_POINT('',#38797);
#8458=VERTEX_POINT('',#38809);
#8459=VERTEX_POINT('',#38812);
#8460=VERTEX_POINT('',#38814);
#8461=VERTEX_POINT('',#38817);
#8462=VERTEX_POINT('',#38819);
#8463=VERTEX_POINT('',#38822);
#8464=VERTEX_POINT('',#38824);
#8465=VERTEX_POINT('',#39432);
#8466=VERTEX_POINT('',#39443);
#8467=VERTEX_POINT('',#39450);
#8468=VERTEX_POINT('',#39465);
#8469=VERTEX_POINT('',#39466);
#8470=VERTEX_POINT('',#39468);
#8471=VERTEX_POINT('',#39470);
#8472=VERTEX_POINT('',#39474);
#8473=VERTEX_POINT('',#39475);
#8474=VERTEX_POINT('',#39480);
#8475=VERTEX_POINT('',#39481);
#8476=VERTEX_POINT('',#39488);
#8477=VERTEX_POINT('',#39489);
#8478=VERTEX_POINT('',#39491);
#8479=VERTEX_POINT('',#39493);
#8480=VERTEX_POINT('',#39497);
#8481=VERTEX_POINT('',#39498);
#8482=VERTEX_POINT('',#39503);
#8483=VERTEX_POINT('',#39504);
#8484=VERTEX_POINT('',#39511);
#8485=VERTEX_POINT('',#39512);
#8486=VERTEX_POINT('',#39514);
#8487=VERTEX_POINT('',#39516);
#8488=VERTEX_POINT('',#39520);
#8489=VERTEX_POINT('',#39521);
#8490=VERTEX_POINT('',#39526);
#8491=VERTEX_POINT('',#39527);
#8492=VERTEX_POINT('',#39534);
#8493=VERTEX_POINT('',#39536);
#8494=VERTEX_POINT('',#39538);
#8495=VERTEX_POINT('',#39540);
#8496=VERTEX_POINT('',#39542);
#8497=VERTEX_POINT('',#39547);
#8498=VERTEX_POINT('',#39550);
#8499=VERTEX_POINT('',#39552);
#8500=VERTEX_POINT('',#39554);
#8501=VERTEX_POINT('',#39556);
#8502=VERTEX_POINT('',#39558);
#8503=VERTEX_POINT('',#39560);
#8504=VERTEX_POINT('',#39730);
#8505=VERTEX_POINT('',#39731);
#8506=VERTEX_POINT('',#39811);
#8507=VERTEX_POINT('',#39813);
#8508=VERTEX_POINT('',#39819);
#8509=VERTEX_POINT('',#39833);
#8510=VERTEX_POINT('',#39847);
#8511=VERTEX_POINT('',#39861);
#8512=VERTEX_POINT('',#39875);
#8513=VERTEX_POINT('',#39889);
#8514=VERTEX_POINT('',#39903);
#8515=VERTEX_POINT('',#39917);
#8516=VERTEX_POINT('',#40169);
#8517=VERTEX_POINT('',#40170);
#8518=VERTEX_POINT('',#40178);
#8519=VERTEX_POINT('',#40192);
#8520=VERTEX_POINT('',#40206);
#8521=VERTEX_POINT('',#40220);
#8522=VERTEX_POINT('',#40234);
#8523=VERTEX_POINT('',#40248);
#8524=VERTEX_POINT('',#40262);
#8525=VERTEX_POINT('',#40276);
#8526=VERTEX_POINT('',#40281);
#8527=VERTEX_POINT('',#40283);
#8528=VERTEX_POINT('',#40827);
#8529=VERTEX_POINT('',#40828);
#8530=VERTEX_POINT('',#40830);
#8531=VERTEX_POINT('',#40832);
#8532=VERTEX_POINT('',#40836);
#8533=VERTEX_POINT('',#40838);
#8534=VERTEX_POINT('',#40842);
#8535=VERTEX_POINT('',#40843);
#8536=VERTEX_POINT('',#40848);
#8537=VERTEX_POINT('',#40849);
#8538=VERTEX_POINT('',#40851);
#8539=VERTEX_POINT('',#40853);
#8540=VERTEX_POINT('',#40857);
#8541=VERTEX_POINT('',#40859);
#8542=VERTEX_POINT('',#40863);
#8543=VERTEX_POINT('',#40864);
#8544=VERTEX_POINT('',#40869);
#8545=VERTEX_POINT('',#40870);
#8546=VERTEX_POINT('',#40872);
#8547=VERTEX_POINT('',#40874);
#8548=VERTEX_POINT('',#40878);
#8549=VERTEX_POINT('',#40880);
#8550=VERTEX_POINT('',#40884);
#8551=VERTEX_POINT('',#40885);
#8552=VERTEX_POINT('',#40890);
#8553=VERTEX_POINT('',#40891);
#8554=VERTEX_POINT('',#40893);
#8555=VERTEX_POINT('',#40895);
#8556=VERTEX_POINT('',#40899);
#8557=VERTEX_POINT('',#40901);
#8558=VERTEX_POINT('',#40905);
#8559=VERTEX_POINT('',#40906);
#8560=VERTEX_POINT('',#40911);
#8561=VERTEX_POINT('',#40912);
#8562=VERTEX_POINT('',#40914);
#8563=VERTEX_POINT('',#40916);
#8564=VERTEX_POINT('',#40920);
#8565=VERTEX_POINT('',#40922);
#8566=VERTEX_POINT('',#40926);
#8567=VERTEX_POINT('',#40927);
#8568=VERTEX_POINT('',#40932);
#8569=VERTEX_POINT('',#40933);
#8570=VERTEX_POINT('',#40935);
#8571=VERTEX_POINT('',#40937);
#8572=VERTEX_POINT('',#40941);
#8573=VERTEX_POINT('',#40943);
#8574=VERTEX_POINT('',#40947);
#8575=VERTEX_POINT('',#40948);
#8576=VERTEX_POINT('',#40953);
#8577=VERTEX_POINT('',#40954);
#8578=VERTEX_POINT('',#40956);
#8579=VERTEX_POINT('',#40958);
#8580=VERTEX_POINT('',#40962);
#8581=VERTEX_POINT('',#40964);
#8582=VERTEX_POINT('',#40968);
#8583=VERTEX_POINT('',#40969);
#8584=VERTEX_POINT('',#40974);
#8585=VERTEX_POINT('',#40975);
#8586=VERTEX_POINT('',#40977);
#8587=VERTEX_POINT('',#40979);
#8588=VERTEX_POINT('',#40983);
#8589=VERTEX_POINT('',#40985);
#8590=VERTEX_POINT('',#40989);
#8591=VERTEX_POINT('',#40990);
#8592=VERTEX_POINT('',#40995);
#8593=VERTEX_POINT('',#40996);
#8594=VERTEX_POINT('',#40998);
#8595=VERTEX_POINT('',#41000);
#8596=VERTEX_POINT('',#41004);
#8597=VERTEX_POINT('',#41006);
#8598=VERTEX_POINT('',#41010);
#8599=VERTEX_POINT('',#41011);
#8600=VERTEX_POINT('',#41016);
#8601=VERTEX_POINT('',#41017);
#8602=VERTEX_POINT('',#41019);
#8603=VERTEX_POINT('',#41021);
#8604=VERTEX_POINT('',#41025);
#8605=VERTEX_POINT('',#41027);
#8606=VERTEX_POINT('',#41031);
#8607=VERTEX_POINT('',#41032);
#8608=VERTEX_POINT('',#41037);
#8609=VERTEX_POINT('',#41038);
#8610=VERTEX_POINT('',#41040);
#8611=VERTEX_POINT('',#41042);
#8612=VERTEX_POINT('',#41046);
#8613=VERTEX_POINT('',#41048);
#8614=VERTEX_POINT('',#41052);
#8615=VERTEX_POINT('',#41053);
#8616=VERTEX_POINT('',#41069);
#8617=VERTEX_POINT('',#41086);
#8618=VERTEX_POINT('',#41088);
#8619=VERTEX_POINT('',#41105);
#8620=VERTEX_POINT('',#41106);
#8621=VERTEX_POINT('',#41108);
#8622=VERTEX_POINT('',#41110);
#8623=VERTEX_POINT('',#41114);
#8624=VERTEX_POINT('',#41115);
#8625=VERTEX_POINT('',#41120);
#8626=VERTEX_POINT('',#41121);
#8627=VERTEX_POINT('',#41126);
#8628=VERTEX_POINT('',#41127);
#8629=VERTEX_POINT('',#41129);
#8630=VERTEX_POINT('',#41131);
#8631=VERTEX_POINT('',#41135);
#8632=VERTEX_POINT('',#41136);
#8633=VERTEX_POINT('',#41141);
#8634=VERTEX_POINT('',#41142);
#8635=VERTEX_POINT('',#41147);
#8636=VERTEX_POINT('',#41148);
#8637=VERTEX_POINT('',#41150);
#8638=VERTEX_POINT('',#41152);
#8639=VERTEX_POINT('',#41154);
#8640=VERTEX_POINT('',#41156);
#8641=VERTEX_POINT('',#41289);
#8642=VERTEX_POINT('',#41290);
#8643=VERTEX_POINT('',#41356);
#8644=VERTEX_POINT('',#41358);
#8645=VERTEX_POINT('',#41368);
#8646=VERTEX_POINT('',#41378);
#8647=VERTEX_POINT('',#41388);
#8648=VERTEX_POINT('',#41398);
#8649=VERTEX_POINT('',#41408);
#8650=VERTEX_POINT('',#41418);
#8651=VERTEX_POINT('',#41428);
#8652=VERTEX_POINT('',#41569);
#8653=VERTEX_POINT('',#41570);
#8654=VERTEX_POINT('',#41580);
#8655=VERTEX_POINT('',#41590);
#8656=VERTEX_POINT('',#41600);
#8657=VERTEX_POINT('',#41610);
#8658=VERTEX_POINT('',#41620);
#8659=VERTEX_POINT('',#41630);
#8660=VERTEX_POINT('',#41640);
#8661=VERTEX_POINT('',#41650);
#8662=VERTEX_POINT('',#41652);
#8663=VERTEX_POINT('',#41727);
#8664=VERTEX_POINT('',#41728);
#8665=VERTEX_POINT('',#41730);
#8666=VERTEX_POINT('',#41732);
#8667=VERTEX_POINT('',#41736);
#8668=VERTEX_POINT('',#41738);
#8669=VERTEX_POINT('',#41741);
#8670=VERTEX_POINT('',#41743);
#8671=VERTEX_POINT('',#41746);
#8672=VERTEX_POINT('',#41748);
#8673=VERTEX_POINT('',#41752);
#8674=VERTEX_POINT('',#41754);
#8675=VERTEX_POINT('',#41756);
#8676=VERTEX_POINT('',#41758);
#8677=VERTEX_POINT('',#41783);
#8678=VERTEX_POINT('',#41793);
#8679=VERTEX_POINT('',#41794);
#8680=VERTEX_POINT('',#41796);
#8681=VERTEX_POINT('',#41798);
#8682=VERTEX_POINT('',#41800);
#8683=VERTEX_POINT('',#41804);
#8684=VERTEX_POINT('',#41806);
#8685=VERTEX_POINT('',#41810);
#8686=VERTEX_POINT('',#41812);
#8687=VERTEX_POINT('',#41814);
#8688=VERTEX_POINT('',#41821);
#8689=VERTEX_POINT('',#41822);
#8690=VERTEX_POINT('',#41824);
#8691=VERTEX_POINT('',#41826);
#8692=VERTEX_POINT('',#41828);
#8693=VERTEX_POINT('',#41832);
#8694=VERTEX_POINT('',#41834);
#8695=VERTEX_POINT('',#41838);
#8696=VERTEX_POINT('',#41840);
#8697=VERTEX_POINT('',#41842);
#8698=VERTEX_POINT('',#41849);
#8699=VERTEX_POINT('',#41850);
#8700=VERTEX_POINT('',#41852);
#8701=VERTEX_POINT('',#41854);
#8702=VERTEX_POINT('',#41856);
#8703=VERTEX_POINT('',#41860);
#8704=VERTEX_POINT('',#41862);
#8705=VERTEX_POINT('',#41866);
#8706=VERTEX_POINT('',#41868);
#8707=VERTEX_POINT('',#41870);
#8708=VERTEX_POINT('',#41877);
#8709=VERTEX_POINT('',#41878);
#8710=VERTEX_POINT('',#41880);
#8711=VERTEX_POINT('',#41882);
#8712=VERTEX_POINT('',#41884);
#8713=VERTEX_POINT('',#41888);
#8714=VERTEX_POINT('',#41890);
#8715=VERTEX_POINT('',#41894);
#8716=VERTEX_POINT('',#41896);
#8717=VERTEX_POINT('',#41898);
#8718=VERTEX_POINT('',#41905);
#8719=VERTEX_POINT('',#41912);
#8720=VERTEX_POINT('',#41919);
#8721=VERTEX_POINT('',#41930);
#8722=VERTEX_POINT('',#41941);
#8723=VERTEX_POINT('',#41974);
#8724=VERTEX_POINT('',#41975);
#8725=VERTEX_POINT('',#41977);
#8726=VERTEX_POINT('',#41982);
#8727=VERTEX_POINT('',#42005);
#8728=VERTEX_POINT('',#42083);
#8729=VERTEX_POINT('',#42084);
#8730=VERTEX_POINT('',#42089);
#8731=VERTEX_POINT('',#42108);
#8732=VERTEX_POINT('',#42141);
#8733=VERTEX_POINT('',#42143);
#8734=VERTEX_POINT('',#42177);
#8735=VERTEX_POINT('',#42178);
#8736=VERTEX_POINT('',#42180);
#8737=VERTEX_POINT('',#42186);
#8738=VERTEX_POINT('',#42210);
#8739=VERTEX_POINT('',#42260);
#8740=VERTEX_POINT('',#42261);
#8741=VERTEX_POINT('',#42270);
#8742=VERTEX_POINT('',#42284);
#8743=VERTEX_POINT('',#42318);
#8744=VERTEX_POINT('',#42320);
#8745=VERTEX_POINT('',#42952);
#8746=VERTEX_POINT('',#42953);
#8747=VERTEX_POINT('',#43084);
#8748=VERTEX_POINT('',#43117);
#8749=VERTEX_POINT('',#43239);
#8750=VERTEX_POINT('',#43384);
#8751=VERTEX_POINT('',#43519);
#8752=VERTEX_POINT('',#43531);
#8753=VERTEX_POINT('',#43548);
#8754=VERTEX_POINT('',#43562);
#8755=VERTEX_POINT('',#44301);
#8756=VERTEX_POINT('',#44455);
#8757=VERTEX_POINT('',#44467);
#8758=VERTEX_POINT('',#44593);
#8759=VERTEX_POINT('',#44748);
#8760=VERTEX_POINT('',#44760);
#8761=VERTEX_POINT('',#44805);
#8762=VERTEX_POINT('',#44807);
#8763=VERTEX_POINT('',#44810);
#8764=VERTEX_POINT('',#44812);
#8765=VERTEX_POINT('',#44815);
#8766=VERTEX_POINT('',#44817);
#8767=VERTEX_POINT('',#44868);
#8768=VERTEX_POINT('',#44870);
#8769=VERTEX_POINT('',#44873);
#8770=VERTEX_POINT('',#44876);
#8771=VERTEX_POINT('',#45458);
#8772=VERTEX_POINT('',#45460);
#8773=LINE('',#19224,#9601);
#8774=LINE('',#19297,#9602);
#8775=LINE('',#19357,#9603);
#8776=LINE('',#19359,#9604);
#8777=LINE('',#19419,#9605);
#8778=LINE('',#19421,#9606);
#8779=LINE('',#19542,#9607);
#8780=LINE('',#19611,#9608);
#8781=LINE('',#19613,#9609);
#8782=LINE('',#19656,#9610);
#8783=LINE('',#19659,#9611);
#8784=LINE('',#19661,#9612);
#8785=LINE('',#19663,#9613);
#8786=LINE('',#19665,#9614);
#8787=LINE('',#19668,#9615);
#8788=LINE('',#19670,#9616);
#8789=LINE('',#19672,#9617);
#8790=LINE('',#19677,#9618);
#8791=LINE('',#19680,#9619);
#8792=LINE('',#19682,#9620);
#8793=LINE('',#19684,#9621);
#8794=LINE('',#19686,#9622);
#8795=LINE('',#19689,#9623);
#8796=LINE('',#19691,#9624);
#8797=LINE('',#19693,#9625);
#8798=LINE('',#19698,#9626);
#8799=LINE('',#19701,#9627);
#8800=LINE('',#19703,#9628);
#8801=LINE('',#19705,#9629);
#8802=LINE('',#19707,#9630);
#8803=LINE('',#19710,#9631);
#8804=LINE('',#19712,#9632);
#8805=LINE('',#19714,#9633);
#8806=LINE('',#19954,#9634);
#8807=LINE('',#19993,#9635);
#8808=LINE('',#19995,#9636);
#8809=LINE('',#20264,#9637);
#8810=LINE('',#20309,#9638);
#8811=LINE('',#20347,#9639);
#8812=LINE('',#20348,#9640);
#8813=LINE('',#20350,#9641);
#8814=LINE('',#20354,#9642);
#8815=LINE('',#20460,#9643);
#8816=LINE('',#20572,#9644);
#8817=LINE('',#27475,#9645);
#8818=LINE('',#27775,#9646);
#8819=LINE('',#28233,#9647);
#8820=LINE('',#28556,#9648);
#8821=LINE('',#30745,#9649);
#8822=LINE('',#30753,#9650);
#8823=LINE('',#30776,#9651);
#8824=LINE('',#30777,#9652);
#8825=LINE('',#30782,#9653);
#8826=LINE('',#30783,#9654);
#8827=LINE('',#30788,#9655);
#8828=LINE('',#30789,#9656);
#8829=LINE('',#30825,#9657);
#8830=LINE('',#30826,#9658);
#8831=LINE('',#30831,#9659);
#8832=LINE('',#30832,#9660);
#8833=LINE('',#30837,#9661);
#8834=LINE('',#30838,#9662);
#8835=LINE('',#30849,#9663);
#8836=LINE('',#30850,#9664);
#8837=LINE('',#30854,#9665);
#8838=LINE('',#30855,#9666);
#8839=LINE('',#30885,#9667);
#8840=LINE('',#30886,#9668);
#8841=LINE('',#30890,#9669);
#8842=LINE('',#30891,#9670);
#8843=LINE('',#30902,#9671);
#8844=LINE('',#30903,#9672);
#8845=LINE('',#30908,#9673);
#8846=LINE('',#30909,#9674);
#8847=LINE('',#30944,#9675);
#8848=LINE('',#30945,#9676);
#8849=LINE('',#30950,#9677);
#8850=LINE('',#30951,#9678);
#8851=LINE('',#30962,#9679);
#8852=LINE('',#30963,#9680);
#8853=LINE('',#30967,#9681);
#8854=LINE('',#30968,#9682);
#8855=LINE('',#30993,#9683);
#8856=LINE('',#30994,#9684);
#8857=LINE('',#30998,#9685);
#8858=LINE('',#30999,#9686);
#8859=LINE('',#31010,#9687);
#8860=LINE('',#31011,#9688);
#8861=LINE('',#31016,#9689);
#8862=LINE('',#31017,#9690);
#8863=LINE('',#31043,#9691);
#8864=LINE('',#31044,#9692);
#8865=LINE('',#31048,#9693);
#8866=LINE('',#31049,#9694);
#8867=LINE('',#31137,#9695);
#8868=LINE('',#31182,#9696);
#8869=LINE('',#31451,#9697);
#8870=LINE('',#31490,#9698);
#8871=LINE('',#31534,#9699);
#8872=LINE('',#31535,#9700);
#8873=LINE('',#31537,#9701);
#8874=LINE('',#31539,#9702);
#8875=LINE('',#31561,#9703);
#8876=LINE('',#31597,#9704);
#8877=LINE('',#31599,#9705);
#8878=LINE('',#31601,#9706);
#8879=LINE('',#31603,#9707);
#8880=LINE('',#31607,#9708);
#8881=LINE('',#31614,#9709);
#8882=LINE('',#31616,#9710);
#8883=LINE('',#31618,#9711);
#8884=LINE('',#31620,#9712);
#8885=LINE('',#31624,#9713);
#8886=LINE('',#31628,#9714);
#8887=LINE('',#31632,#9715);
#8888=LINE('',#31633,#9716);
#8889=LINE('',#31638,#9717);
#8890=LINE('',#31639,#9718);
#8891=LINE('',#31640,#9719);
#8892=LINE('',#32290,#9720);
#8893=LINE('',#32291,#9721);
#8894=LINE('',#32648,#9722);
#8895=LINE('',#32653,#9723);
#8896=LINE('',#32656,#9724);
#8897=LINE('',#32658,#9725);
#8898=LINE('',#33354,#9726);
#8899=LINE('',#33355,#9727);
#8900=LINE('',#33357,#9728);
#8901=LINE('',#33360,#9729);
#8902=LINE('',#33367,#9730);
#8903=LINE('',#33755,#9731);
#8904=LINE('',#33815,#9732);
#8905=LINE('',#33930,#9733);
#8906=LINE('',#34005,#9734);
#8907=LINE('',#34065,#9735);
#8908=LINE('',#34066,#9736);
#8909=LINE('',#34068,#9737);
#8910=LINE('',#34070,#9738);
#8911=LINE('',#34072,#9739);
#8912=LINE('',#34078,#9740);
#8913=LINE('',#34083,#9741);
#8914=LINE('',#34085,#9742);
#8915=LINE('',#34089,#9743);
#8916=LINE('',#34091,#9744);
#8917=LINE('',#34095,#9745);
#8918=LINE('',#34097,#9746);
#8919=LINE('',#34101,#9747);
#8920=LINE('',#34103,#9748);
#8921=LINE('',#34107,#9749);
#8922=LINE('',#34109,#9750);
#8923=LINE('',#34113,#9751);
#8924=LINE('',#34115,#9752);
#8925=LINE('',#34119,#9753);
#8926=LINE('',#34121,#9754);
#8927=LINE('',#34125,#9755);
#8928=LINE('',#34127,#9756);
#8929=LINE('',#34131,#9757);
#8930=LINE('',#34133,#9758);
#8931=LINE('',#34137,#9759);
#8932=LINE('',#34139,#9760);
#8933=LINE('',#34143,#9761);
#8934=LINE('',#34145,#9762);
#8935=LINE('',#34149,#9763);
#8936=LINE('',#34151,#9764);
#8937=LINE('',#34155,#9765);
#8938=LINE('',#34157,#9766);
#8939=LINE('',#34161,#9767);
#8940=LINE('',#34163,#9768);
#8941=LINE('',#34167,#9769);
#8942=LINE('',#34169,#9770);
#8943=LINE('',#34173,#9771);
#8944=LINE('',#34175,#9772);
#8945=LINE('',#34179,#9773);
#8946=LINE('',#34181,#9774);
#8947=LINE('',#34185,#9775);
#8948=LINE('',#34187,#9776);
#8949=LINE('',#34191,#9777);
#8950=LINE('',#34193,#9778);
#8951=LINE('',#34197,#9779);
#8952=LINE('',#34199,#9780);
#8953=LINE('',#34203,#9781);
#8954=LINE('',#34205,#9782);
#8955=LINE('',#34209,#9783);
#8956=LINE('',#34211,#9784);
#8957=LINE('',#34215,#9785);
#8958=LINE('',#34217,#9786);
#8959=LINE('',#34221,#9787);
#8960=LINE('',#34223,#9788);
#8961=LINE('',#34227,#9789);
#8962=LINE('',#34229,#9790);
#8963=LINE('',#34233,#9791);
#8964=LINE('',#34235,#9792);
#8965=LINE('',#34239,#9793);
#8966=LINE('',#34241,#9794);
#8967=LINE('',#34245,#9795);
#8968=LINE('',#34247,#9796);
#8969=LINE('',#34251,#9797);
#8970=LINE('',#34253,#9798);
#8971=LINE('',#34257,#9799);
#8972=LINE('',#34259,#9800);
#8973=LINE('',#34263,#9801);
#8974=LINE('',#34265,#9802);
#8975=LINE('',#34269,#9803);
#8976=LINE('',#34271,#9804);
#8977=LINE('',#34275,#9805);
#8978=LINE('',#34277,#9806);
#8979=LINE('',#34281,#9807);
#8980=LINE('',#34283,#9808);
#8981=LINE('',#34287,#9809);
#8982=LINE('',#34289,#9810);
#8983=LINE('',#34293,#9811);
#8984=LINE('',#34295,#9812);
#8985=LINE('',#34299,#9813);
#8986=LINE('',#34301,#9814);
#8987=LINE('',#34305,#9815);
#8988=LINE('',#34307,#9816);
#8989=LINE('',#34311,#9817);
#8990=LINE('',#34313,#9818);
#8991=LINE('',#34317,#9819);
#8992=LINE('',#34319,#9820);
#8993=LINE('',#34323,#9821);
#8994=LINE('',#34325,#9822);
#8995=LINE('',#34329,#9823);
#8996=LINE('',#34331,#9824);
#8997=LINE('',#34335,#9825);
#8998=LINE('',#34337,#9826);
#8999=LINE('',#34339,#9827);
#9000=LINE('',#34341,#9828);
#9001=LINE('',#34345,#9829);
#9002=LINE('',#34347,#9830);
#9003=LINE('',#34351,#9831);
#9004=LINE('',#34353,#9832);
#9005=LINE('',#34357,#9833);
#9006=LINE('',#34359,#9834);
#9007=LINE('',#34363,#9835);
#9008=LINE('',#34367,#9836);
#9009=LINE('',#34370,#9837);
#9010=LINE('',#34374,#9838);
#9011=LINE('',#34376,#9839);
#9012=LINE('',#34380,#9840);
#9013=LINE('',#34382,#9841);
#9014=LINE('',#34386,#9842);
#9015=LINE('',#34388,#9843);
#9016=LINE('',#34392,#9844);
#9017=LINE('',#34394,#9845);
#9018=LINE('',#34396,#9846);
#9019=LINE('',#34398,#9847);
#9020=LINE('',#34402,#9848);
#9021=LINE('',#34404,#9849);
#9022=LINE('',#34408,#9850);
#9023=LINE('',#34410,#9851);
#9024=LINE('',#34414,#9852);
#9025=LINE('',#34416,#9853);
#9026=LINE('',#34420,#9854);
#9027=LINE('',#34422,#9855);
#9028=LINE('',#34426,#9856);
#9029=LINE('',#34428,#9857);
#9030=LINE('',#34432,#9858);
#9031=LINE('',#34434,#9859);
#9032=LINE('',#34438,#9860);
#9033=LINE('',#34440,#9861);
#9034=LINE('',#34444,#9862);
#9035=LINE('',#34446,#9863);
#9036=LINE('',#34450,#9864);
#9037=LINE('',#34452,#9865);
#9038=LINE('',#34456,#9866);
#9039=LINE('',#34458,#9867);
#9040=LINE('',#34462,#9868);
#9041=LINE('',#34464,#9869);
#9042=LINE('',#34468,#9870);
#9043=LINE('',#34470,#9871);
#9044=LINE('',#34474,#9872);
#9045=LINE('',#34476,#9873);
#9046=LINE('',#34480,#9874);
#9047=LINE('',#34482,#9875);
#9048=LINE('',#34486,#9876);
#9049=LINE('',#34488,#9877);
#9050=LINE('',#34492,#9878);
#9051=LINE('',#34494,#9879);
#9052=LINE('',#34498,#9880);
#9053=LINE('',#34500,#9881);
#9054=LINE('',#34504,#9882);
#9055=LINE('',#34506,#9883);
#9056=LINE('',#34510,#9884);
#9057=LINE('',#34512,#9885);
#9058=LINE('',#34516,#9886);
#9059=LINE('',#34518,#9887);
#9060=LINE('',#34522,#9888);
#9061=LINE('',#34524,#9889);
#9062=LINE('',#34528,#9890);
#9063=LINE('',#34530,#9891);
#9064=LINE('',#34534,#9892);
#9065=LINE('',#34536,#9893);
#9066=LINE('',#34540,#9894);
#9067=LINE('',#34542,#9895);
#9068=LINE('',#34546,#9896);
#9069=LINE('',#34548,#9897);
#9070=LINE('',#34552,#9898);
#9071=LINE('',#34554,#9899);
#9072=LINE('',#34558,#9900);
#9073=LINE('',#34560,#9901);
#9074=LINE('',#34564,#9902);
#9075=LINE('',#34566,#9903);
#9076=LINE('',#34570,#9904);
#9077=LINE('',#34572,#9905);
#9078=LINE('',#34576,#9906);
#9079=LINE('',#34578,#9907);
#9080=LINE('',#34582,#9908);
#9081=LINE('',#34584,#9909);
#9082=LINE('',#34588,#9910);
#9083=LINE('',#34590,#9911);
#9084=LINE('',#34594,#9912);
#9085=LINE('',#34596,#9913);
#9086=LINE('',#34600,#9914);
#9087=LINE('',#34602,#9915);
#9088=LINE('',#34606,#9916);
#9089=LINE('',#34608,#9917);
#9090=LINE('',#34612,#9918);
#9091=LINE('',#34614,#9919);
#9092=LINE('',#34618,#9920);
#9093=LINE('',#34620,#9921);
#9094=LINE('',#34624,#9922);
#9095=LINE('',#34626,#9923);
#9096=LINE('',#34630,#9924);
#9097=LINE('',#34632,#9925);
#9098=LINE('',#34636,#9926);
#9099=LINE('',#34638,#9927);
#9100=LINE('',#34642,#9928);
#9101=LINE('',#34644,#9929);
#9102=LINE('',#34648,#9930);
#9103=LINE('',#34650,#9931);
#9104=LINE('',#34656,#9932);
#9105=LINE('',#34657,#9933);
#9106=LINE('',#34659,#9934);
#9107=LINE('',#34661,#9935);
#9108=LINE('',#34663,#9936);
#9109=LINE('',#34665,#9937);
#9110=LINE('',#34667,#9938);
#9111=LINE('',#34669,#9939);
#9112=LINE('',#34671,#9940);
#9113=LINE('',#34673,#9941);
#9114=LINE('',#34675,#9942);
#9115=LINE('',#34677,#9943);
#9116=LINE('',#34679,#9944);
#9117=LINE('',#34681,#9945);
#9118=LINE('',#34683,#9946);
#9119=LINE('',#34685,#9947);
#9120=LINE('',#34687,#9948);
#9121=LINE('',#34689,#9949);
#9122=LINE('',#34691,#9950);
#9123=LINE('',#34693,#9951);
#9124=LINE('',#34695,#9952);
#9125=LINE('',#34697,#9953);
#9126=LINE('',#34699,#9954);
#9127=LINE('',#34701,#9955);
#9128=LINE('',#34703,#9956);
#9129=LINE('',#34705,#9957);
#9130=LINE('',#34707,#9958);
#9131=LINE('',#34709,#9959);
#9132=LINE('',#34711,#9960);
#9133=LINE('',#34713,#9961);
#9134=LINE('',#34715,#9962);
#9135=LINE('',#34717,#9963);
#9136=LINE('',#34719,#9964);
#9137=LINE('',#34721,#9965);
#9138=LINE('',#34723,#9966);
#9139=LINE('',#34725,#9967);
#9140=LINE('',#34727,#9968);
#9141=LINE('',#34729,#9969);
#9142=LINE('',#34731,#9970);
#9143=LINE('',#34733,#9971);
#9144=LINE('',#34735,#9972);
#9145=LINE('',#34737,#9973);
#9146=LINE('',#34739,#9974);
#9147=LINE('',#34741,#9975);
#9148=LINE('',#34743,#9976);
#9149=LINE('',#34745,#9977);
#9150=LINE('',#34747,#9978);
#9151=LINE('',#34749,#9979);
#9152=LINE('',#34751,#9980);
#9153=LINE('',#34753,#9981);
#9154=LINE('',#34755,#9982);
#9155=LINE('',#34757,#9983);
#9156=LINE('',#34759,#9984);
#9157=LINE('',#34761,#9985);
#9158=LINE('',#34763,#9986);
#9159=LINE('',#34765,#9987);
#9160=LINE('',#34767,#9988);
#9161=LINE('',#34769,#9989);
#9162=LINE('',#34771,#9990);
#9163=LINE('',#34773,#9991);
#9164=LINE('',#34775,#9992);
#9165=LINE('',#34777,#9993);
#9166=LINE('',#34779,#9994);
#9167=LINE('',#34781,#9995);
#9168=LINE('',#34783,#9996);
#9169=LINE('',#34785,#9997);
#9170=LINE('',#34787,#9998);
#9171=LINE('',#34789,#9999);
#9172=LINE('',#34791,#10000);
#9173=LINE('',#34793,#10001);
#9174=LINE('',#34795,#10002);
#9175=LINE('',#34797,#10003);
#9176=LINE('',#34799,#10004);
#9177=LINE('',#34801,#10005);
#9178=LINE('',#34803,#10006);
#9179=LINE('',#34805,#10007);
#9180=LINE('',#34807,#10008);
#9181=LINE('',#34809,#10009);
#9182=LINE('',#34811,#10010);
#9183=LINE('',#34813,#10011);
#9184=LINE('',#34815,#10012);
#9185=LINE('',#34817,#10013);
#9186=LINE('',#34819,#10014);
#9187=LINE('',#34821,#10015);
#9188=LINE('',#34823,#10016);
#9189=LINE('',#34825,#10017);
#9190=LINE('',#34827,#10018);
#9191=LINE('',#34829,#10019);
#9192=LINE('',#34831,#10020);
#9193=LINE('',#34833,#10021);
#9194=LINE('',#34835,#10022);
#9195=LINE('',#34837,#10023);
#9196=LINE('',#34839,#10024);
#9197=LINE('',#34841,#10025);
#9198=LINE('',#34843,#10026);
#9199=LINE('',#34845,#10027);
#9200=LINE('',#34847,#10028);
#9201=LINE('',#34849,#10029);
#9202=LINE('',#34851,#10030);
#9203=LINE('',#34853,#10031);
#9204=LINE('',#34855,#10032);
#9205=LINE('',#34857,#10033);
#9206=LINE('',#34859,#10034);
#9207=LINE('',#34861,#10035);
#9208=LINE('',#34863,#10036);
#9209=LINE('',#34865,#10037);
#9210=LINE('',#34867,#10038);
#9211=LINE('',#34869,#10039);
#9212=LINE('',#34871,#10040);
#9213=LINE('',#34873,#10041);
#9214=LINE('',#34875,#10042);
#9215=LINE('',#34877,#10043);
#9216=LINE('',#34879,#10044);
#9217=LINE('',#34881,#10045);
#9218=LINE('',#34883,#10046);
#9219=LINE('',#34885,#10047);
#9220=LINE('',#34887,#10048);
#9221=LINE('',#34889,#10049);
#9222=LINE('',#34891,#10050);
#9223=LINE('',#34893,#10051);
#9224=LINE('',#34895,#10052);
#9225=LINE('',#34897,#10053);
#9226=LINE('',#34899,#10054);
#9227=LINE('',#34901,#10055);
#9228=LINE('',#34903,#10056);
#9229=LINE('',#34905,#10057);
#9230=LINE('',#34907,#10058);
#9231=LINE('',#34909,#10059);
#9232=LINE('',#34911,#10060);
#9233=LINE('',#34913,#10061);
#9234=LINE('',#34915,#10062);
#9235=LINE('',#34917,#10063);
#9236=LINE('',#34919,#10064);
#9237=LINE('',#34921,#10065);
#9238=LINE('',#34923,#10066);
#9239=LINE('',#34925,#10067);
#9240=LINE('',#34927,#10068);
#9241=LINE('',#34929,#10069);
#9242=LINE('',#34931,#10070);
#9243=LINE('',#34933,#10071);
#9244=LINE('',#34935,#10072);
#9245=LINE('',#34937,#10073);
#9246=LINE('',#34939,#10074);
#9247=LINE('',#34996,#10075);
#9248=LINE('',#34997,#10076);
#9249=LINE('',#35002,#10077);
#9250=LINE('',#35003,#10078);
#9251=LINE('',#35017,#10079);
#9252=LINE('',#35018,#10080);
#9253=LINE('',#35023,#10081);
#9254=LINE('',#35024,#10082);
#9255=LINE('',#35051,#10083);
#9256=LINE('',#35054,#10084);
#9257=LINE('',#35056,#10085);
#9258=LINE('',#35058,#10086);
#9259=LINE('',#35062,#10087);
#9260=LINE('',#35066,#10088);
#9261=LINE('',#35068,#10089);
#9262=LINE('',#35070,#10090);
#9263=LINE('',#35072,#10091);
#9264=LINE('',#35075,#10092);
#9265=LINE('',#35077,#10093);
#9266=LINE('',#35079,#10094);
#9267=LINE('',#35081,#10095);
#9268=LINE('',#35084,#10096);
#9269=LINE('',#35086,#10097);
#9270=LINE('',#35088,#10098);
#9271=LINE('',#35093,#10099);
#9272=LINE('',#35096,#10100);
#9273=LINE('',#35098,#10101);
#9274=LINE('',#35100,#10102);
#9275=LINE('',#35102,#10103);
#9276=LINE('',#35105,#10104);
#9277=LINE('',#35107,#10105);
#9278=LINE('',#35109,#10106);
#9279=LINE('',#35189,#10107);
#9280=LINE('',#35193,#10108);
#9281=LINE('',#35195,#10109);
#9282=LINE('',#35197,#10110);
#9283=LINE('',#35199,#10111);
#9284=LINE('',#35201,#10112);
#9285=LINE('',#35203,#10113);
#9286=LINE('',#35205,#10114);
#9287=LINE('',#35212,#10115);
#9288=LINE('',#35216,#10116);
#9289=LINE('',#35218,#10117);
#9290=LINE('',#35220,#10118);
#9291=LINE('',#35222,#10119);
#9292=LINE('',#35224,#10120);
#9293=LINE('',#35226,#10121);
#9294=LINE('',#35228,#10122);
#9295=LINE('',#35235,#10123);
#9296=LINE('',#35239,#10124);
#9297=LINE('',#35241,#10125);
#9298=LINE('',#35243,#10126);
#9299=LINE('',#35245,#10127);
#9300=LINE('',#35247,#10128);
#9301=LINE('',#35249,#10129);
#9302=LINE('',#35251,#10130);
#9303=LINE('',#35274,#10131);
#9304=LINE('',#35277,#10132);
#9305=LINE('',#35279,#10133);
#9306=LINE('',#35281,#10134);
#9307=LINE('',#35283,#10135);
#9308=LINE('',#35286,#10136);
#9309=LINE('',#35288,#10137);
#9310=LINE('',#35290,#10138);
#9311=LINE('',#35292,#10139);
#9312=LINE('',#35295,#10140);
#9313=LINE('',#35297,#10141);
#9314=LINE('',#35299,#10142);
#9315=LINE('',#35301,#10143);
#9316=LINE('',#35304,#10144);
#9317=LINE('',#35306,#10145);
#9318=LINE('',#35308,#10146);
#9319=LINE('',#35322,#10147);
#9320=LINE('',#35323,#10148);
#9321=LINE('',#35328,#10149);
#9322=LINE('',#35329,#10150);
#9323=LINE('',#35343,#10151);
#9324=LINE('',#35344,#10152);
#9325=LINE('',#35349,#10153);
#9326=LINE('',#35350,#10154);
#9327=LINE('',#35386,#10155);
#9328=LINE('',#35390,#10156);
#9329=LINE('',#35397,#10157);
#9330=LINE('',#35401,#10158);
#9331=LINE('',#35406,#10159);
#9332=LINE('',#35411,#10160);
#9333=LINE('',#35412,#10161);
#9334=LINE('',#35419,#10162);
#9335=LINE('',#35421,#10163);
#9336=LINE('',#35425,#10164);
#9337=LINE('',#35432,#10165);
#9338=LINE('',#35436,#10166);
#9339=LINE('',#35444,#10167);
#9340=LINE('',#35449,#10168);
#9341=LINE('',#35450,#10169);
#9342=LINE('',#35457,#10170);
#9343=LINE('',#35462,#10171);
#9344=LINE('',#35466,#10172);
#9345=LINE('',#35468,#10173);
#9346=LINE('',#35469,#10174);
#9347=LINE('',#35476,#10175);
#9348=LINE('',#35480,#10176);
#9349=LINE('',#35488,#10177);
#9350=LINE('',#35495,#10178);
#9351=LINE('',#35503,#10179);
#9352=LINE('',#35507,#10180);
#9353=LINE('',#35514,#10181);
#9354=LINE('',#35518,#10182);
#9355=LINE('',#35526,#10183);
#9356=LINE('',#35531,#10184);
#9357=LINE('',#35532,#10185);
#9358=LINE('',#35539,#10186);
#9359=LINE('',#35544,#10187);
#9360=LINE('',#35548,#10188);
#9361=LINE('',#35550,#10189);
#9362=LINE('',#35551,#10190);
#9363=LINE('',#35553,#10191);
#9364=LINE('',#35555,#10192);
#9365=LINE('',#35557,#10193);
#9366=LINE('',#35559,#10194);
#9367=LINE('',#35562,#10195);
#9368=LINE('',#35563,#10196);
#9369=LINE('',#35565,#10197);
#9370=LINE('',#35567,#10198);
#9371=LINE('',#35571,#10199);
#9372=LINE('',#35572,#10200);
#9373=LINE('',#35574,#10201);
#9374=LINE('',#35576,#10202);
#9375=LINE('',#35578,#10203);
#9376=LINE('',#35580,#10204);
#9377=LINE('',#35582,#10205);
#9378=LINE('',#35583,#10206);
#9379=LINE('',#35585,#10207);
#9380=LINE('',#35587,#10208);
#9381=LINE('',#35723,#10209);
#9382=LINE('',#35806,#10210);
#9383=LINE('',#36003,#10211);
#9384=LINE('',#36072,#10212);
#9385=LINE('',#36154,#10213);
#9386=LINE('',#36155,#10214);
#9387=LINE('',#36157,#10215);
#9388=LINE('',#36159,#10216);
#9389=LINE('',#39457,#10217);
#9390=LINE('',#39459,#10218);
#9391=LINE('',#39467,#10219);
#9392=LINE('',#39471,#10220);
#9393=LINE('',#39473,#10221);
#9394=LINE('',#39476,#10222);
#9395=LINE('',#39477,#10223);
#9396=LINE('',#39479,#10224);
#9397=LINE('',#39482,#10225);
#9398=LINE('',#39483,#10226);
#9399=LINE('',#39490,#10227);
#9400=LINE('',#39494,#10228);
#9401=LINE('',#39496,#10229);
#9402=LINE('',#39499,#10230);
#9403=LINE('',#39500,#10231);
#9404=LINE('',#39502,#10232);
#9405=LINE('',#39505,#10233);
#9406=LINE('',#39506,#10234);
#9407=LINE('',#39513,#10235);
#9408=LINE('',#39517,#10236);
#9409=LINE('',#39519,#10237);
#9410=LINE('',#39522,#10238);
#9411=LINE('',#39523,#10239);
#9412=LINE('',#39525,#10240);
#9413=LINE('',#39528,#10241);
#9414=LINE('',#39529,#10242);
#9415=LINE('',#39729,#10243);
#9416=LINE('',#39812,#10244);
#9417=LINE('',#40168,#10245);
#9418=LINE('',#40282,#10246);
#9419=LINE('',#40819,#10247);
#9420=LINE('',#40820,#10248);
#9421=LINE('',#40822,#10249);
#9422=LINE('',#40824,#10250);
#9423=LINE('',#40826,#10251);
#9424=LINE('',#40829,#10252);
#9425=LINE('',#40831,#10253);
#9426=LINE('',#40833,#10254);
#9427=LINE('',#40835,#10255);
#9428=LINE('',#40837,#10256);
#9429=LINE('',#40839,#10257);
#9430=LINE('',#40841,#10258);
#9431=LINE('',#40844,#10259);
#9432=LINE('',#40845,#10260);
#9433=LINE('',#40847,#10261);
#9434=LINE('',#40850,#10262);
#9435=LINE('',#40852,#10263);
#9436=LINE('',#40854,#10264);
#9437=LINE('',#40856,#10265);
#9438=LINE('',#40858,#10266);
#9439=LINE('',#40860,#10267);
#9440=LINE('',#40862,#10268);
#9441=LINE('',#40865,#10269);
#9442=LINE('',#40866,#10270);
#9443=LINE('',#40868,#10271);
#9444=LINE('',#40871,#10272);
#9445=LINE('',#40873,#10273);
#9446=LINE('',#40875,#10274);
#9447=LINE('',#40877,#10275);
#9448=LINE('',#40879,#10276);
#9449=LINE('',#40881,#10277);
#9450=LINE('',#40883,#10278);
#9451=LINE('',#40886,#10279);
#9452=LINE('',#40887,#10280);
#9453=LINE('',#40889,#10281);
#9454=LINE('',#40892,#10282);
#9455=LINE('',#40894,#10283);
#9456=LINE('',#40896,#10284);
#9457=LINE('',#40898,#10285);
#9458=LINE('',#40900,#10286);
#9459=LINE('',#40902,#10287);
#9460=LINE('',#40904,#10288);
#9461=LINE('',#40907,#10289);
#9462=LINE('',#40908,#10290);
#9463=LINE('',#40910,#10291);
#9464=LINE('',#40913,#10292);
#9465=LINE('',#40915,#10293);
#9466=LINE('',#40917,#10294);
#9467=LINE('',#40919,#10295);
#9468=LINE('',#40921,#10296);
#9469=LINE('',#40923,#10297);
#9470=LINE('',#40925,#10298);
#9471=LINE('',#40928,#10299);
#9472=LINE('',#40929,#10300);
#9473=LINE('',#40931,#10301);
#9474=LINE('',#40934,#10302);
#9475=LINE('',#40936,#10303);
#9476=LINE('',#40938,#10304);
#9477=LINE('',#40940,#10305);
#9478=LINE('',#40942,#10306);
#9479=LINE('',#40944,#10307);
#9480=LINE('',#40946,#10308);
#9481=LINE('',#40949,#10309);
#9482=LINE('',#40950,#10310);
#9483=LINE('',#40952,#10311);
#9484=LINE('',#40955,#10312);
#9485=LINE('',#40957,#10313);
#9486=LINE('',#40959,#10314);
#9487=LINE('',#40961,#10315);
#9488=LINE('',#40963,#10316);
#9489=LINE('',#40965,#10317);
#9490=LINE('',#40967,#10318);
#9491=LINE('',#40970,#10319);
#9492=LINE('',#40971,#10320);
#9493=LINE('',#40973,#10321);
#9494=LINE('',#40976,#10322);
#9495=LINE('',#40978,#10323);
#9496=LINE('',#40980,#10324);
#9497=LINE('',#40982,#10325);
#9498=LINE('',#40984,#10326);
#9499=LINE('',#40986,#10327);
#9500=LINE('',#40988,#10328);
#9501=LINE('',#40991,#10329);
#9502=LINE('',#40992,#10330);
#9503=LINE('',#40994,#10331);
#9504=LINE('',#40997,#10332);
#9505=LINE('',#40999,#10333);
#9506=LINE('',#41001,#10334);
#9507=LINE('',#41003,#10335);
#9508=LINE('',#41005,#10336);
#9509=LINE('',#41007,#10337);
#9510=LINE('',#41009,#10338);
#9511=LINE('',#41012,#10339);
#9512=LINE('',#41013,#10340);
#9513=LINE('',#41015,#10341);
#9514=LINE('',#41018,#10342);
#9515=LINE('',#41020,#10343);
#9516=LINE('',#41022,#10344);
#9517=LINE('',#41024,#10345);
#9518=LINE('',#41026,#10346);
#9519=LINE('',#41028,#10347);
#9520=LINE('',#41030,#10348);
#9521=LINE('',#41033,#10349);
#9522=LINE('',#41034,#10350);
#9523=LINE('',#41036,#10351);
#9524=LINE('',#41039,#10352);
#9525=LINE('',#41041,#10353);
#9526=LINE('',#41043,#10354);
#9527=LINE('',#41045,#10355);
#9528=LINE('',#41047,#10356);
#9529=LINE('',#41049,#10357);
#9530=LINE('',#41051,#10358);
#9531=LINE('',#41054,#10359);
#9532=LINE('',#41055,#10360);
#9533=LINE('',#41116,#10361);
#9534=LINE('',#41117,#10362);
#9535=LINE('',#41122,#10363);
#9536=LINE('',#41123,#10364);
#9537=LINE('',#41137,#10365);
#9538=LINE('',#41138,#10366);
#9539=LINE('',#41143,#10367);
#9540=LINE('',#41144,#10368);
#9541=LINE('',#41146,#10369);
#9542=LINE('',#41155,#10370);
#9543=LINE('',#41288,#10371);
#9544=LINE('',#41357,#10372);
#9545=LINE('',#41568,#10373);
#9546=LINE('',#41651,#10374);
#9547=LINE('',#41719,#10375);
#9548=LINE('',#41720,#10376);
#9549=LINE('',#41722,#10377);
#9550=LINE('',#41724,#10378);
#9551=LINE('',#41726,#10379);
#9552=LINE('',#41731,#10380);
#9553=LINE('',#41740,#10381);
#9554=LINE('',#41744,#10382);
#9555=LINE('',#41745,#10383);
#9556=LINE('',#41749,#10384);
#9557=LINE('',#41755,#10385);
#9558=LINE('',#41759,#10386);
#9559=LINE('',#41761,#10387);
#9560=LINE('',#41763,#10388);
#9561=LINE('',#41792,#10389);
#9562=LINE('',#41795,#10390);
#9563=LINE('',#41797,#10391);
#9564=LINE('',#41799,#10392);
#9565=LINE('',#41801,#10393);
#9566=LINE('',#41805,#10394);
#9567=LINE('',#41809,#10395);
#9568=LINE('',#41811,#10396);
#9569=LINE('',#41813,#10397);
#9570=LINE('',#41815,#10398);
#9571=LINE('',#41820,#10399);
#9572=LINE('',#41823,#10400);
#9573=LINE('',#41825,#10401);
#9574=LINE('',#41827,#10402);
#9575=LINE('',#41829,#10403);
#9576=LINE('',#41833,#10404);
#9577=LINE('',#41837,#10405);
#9578=LINE('',#41839,#10406);
#9579=LINE('',#41841,#10407);
#9580=LINE('',#41843,#10408);
#9581=LINE('',#41848,#10409);
#9582=LINE('',#41851,#10410);
#9583=LINE('',#41853,#10411);
#9584=LINE('',#41855,#10412);
#9585=LINE('',#41857,#10413);
#9586=LINE('',#41861,#10414);
#9587=LINE('',#41865,#10415);
#9588=LINE('',#41867,#10416);
#9589=LINE('',#41869,#10417);
#9590=LINE('',#41871,#10418);
#9591=LINE('',#41876,#10419);
#9592=LINE('',#41879,#10420);
#9593=LINE('',#41881,#10421);
#9594=LINE('',#41883,#10422);
#9595=LINE('',#41885,#10423);
#9596=LINE('',#41889,#10424);
#9597=LINE('',#41893,#10425);
#9598=LINE('',#41895,#10426);
#9599=LINE('',#41897,#10427);
#9600=LINE('',#41899,#10428);
#9601=VECTOR('',#15297,1.);
#9602=VECTOR('',#15298,1.);
#9603=VECTOR('',#15301,1.);
#9604=VECTOR('',#15302,1.);
#9605=VECTOR('',#15305,1.);
#9606=VECTOR('',#15306,1.);
#9607=VECTOR('',#15307,1.);
#9608=VECTOR('',#15310,1.);
#9609=VECTOR('',#15311,1.);
#9610=VECTOR('',#15336,1.);
#9611=VECTOR('',#15337,1.);
#9612=VECTOR('',#15338,1.);
#9613=VECTOR('',#15339,1.);
#9614=VECTOR('',#15342,1.);
#9615=VECTOR('',#15343,1.);
#9616=VECTOR('',#15344,1.);
#9617=VECTOR('',#15345,1.);
#9618=VECTOR('',#15354,1.);
#9619=VECTOR('',#15355,1.);
#9620=VECTOR('',#15356,1.);
#9621=VECTOR('',#15357,1.);
#9622=VECTOR('',#15360,1.);
#9623=VECTOR('',#15361,1.);
#9624=VECTOR('',#15362,1.);
#9625=VECTOR('',#15363,1.);
#9626=VECTOR('',#15372,1.);
#9627=VECTOR('',#15373,1.);
#9628=VECTOR('',#15374,1.);
#9629=VECTOR('',#15375,1.);
#9630=VECTOR('',#15378,1.);
#9631=VECTOR('',#15379,1.);
#9632=VECTOR('',#15380,1.);
#9633=VECTOR('',#15381,1.);
#9634=VECTOR('',#15544,1.);
#9635=VECTOR('',#15545,1.);
#9636=VECTOR('',#15546,1.);
#9637=VECTOR('',#15549,1.);
#9638=VECTOR('',#15550,1.);
#9639=VECTOR('',#15553,1.);
#9640=VECTOR('',#15554,1.);
#9641=VECTOR('',#15557,1.);
#9642=VECTOR('',#15562,1.);
#9643=VECTOR('',#15707,1.);
#9644=VECTOR('',#15712,1.);
#9645=VECTOR('',#15719,1.);
#9646=VECTOR('',#15726,1.);
#9647=VECTOR('',#15729,1.);
#9648=VECTOR('',#15734,1.);
#9649=VECTOR('',#15761,1.);
#9650=VECTOR('',#15762,1.);
#9651=VECTOR('',#15791,1.);
#9652=VECTOR('',#15792,1.);
#9653=VECTOR('',#15797,1.);
#9654=VECTOR('',#15798,1.);
#9655=VECTOR('',#15803,1.);
#9656=VECTOR('',#15804,1.);
#9657=VECTOR('',#15841,1.);
#9658=VECTOR('',#15842,1.);
#9659=VECTOR('',#15847,1.);
#9660=VECTOR('',#15848,1.);
#9661=VECTOR('',#15853,1.);
#9662=VECTOR('',#15854,1.);
#9663=VECTOR('',#15867,1.);
#9664=VECTOR('',#15868,1.);
#9665=VECTOR('',#15873,1.);
#9666=VECTOR('',#15874,1.);
#9667=VECTOR('',#15915,1.);
#9668=VECTOR('',#15916,1.);
#9669=VECTOR('',#15921,1.);
#9670=VECTOR('',#15922,1.);
#9671=VECTOR('',#15935,1.);
#9672=VECTOR('',#15936,1.);
#9673=VECTOR('',#15941,1.);
#9674=VECTOR('',#15942,1.);
#9675=VECTOR('',#15991,1.);
#9676=VECTOR('',#15992,1.);
#9677=VECTOR('',#15997,1.);
#9678=VECTOR('',#15998,1.);
#9679=VECTOR('',#16011,1.);
#9680=VECTOR('',#16012,1.);
#9681=VECTOR('',#16017,1.);
#9682=VECTOR('',#16018,1.);
#9683=VECTOR('',#16051,1.);
#9684=VECTOR('',#16052,1.);
#9685=VECTOR('',#16057,1.);
#9686=VECTOR('',#16058,1.);
#9687=VECTOR('',#16071,1.);
#9688=VECTOR('',#16072,1.);
#9689=VECTOR('',#16077,1.);
#9690=VECTOR('',#16078,1.);
#9691=VECTOR('',#16117,1.);
#9692=VECTOR('',#16118,1.);
#9693=VECTOR('',#16123,1.);
#9694=VECTOR('',#16124,1.);
#9695=VECTOR('',#16147,1.);
#9696=VECTOR('',#16148,1.);
#9697=VECTOR('',#16149,1.);
#9698=VECTOR('',#16150,1.);
#9699=VECTOR('',#16153,1.);
#9700=VECTOR('',#16154,1.);
#9701=VECTOR('',#16157,1.);
#9702=VECTOR('',#16160,1.);
#9703=VECTOR('',#16191,1.);
#9704=VECTOR('',#16250,1.);
#9705=VECTOR('',#16251,1.);
#9706=VECTOR('',#16252,1.);
#9707=VECTOR('',#16255,1.);
#9708=VECTOR('',#16260,1.);
#9709=VECTOR('',#16267,1.);
#9710=VECTOR('',#16268,1.);
#9711=VECTOR('',#16269,1.);
#9712=VECTOR('',#16272,1.);
#9713=VECTOR('',#16277,1.);
#9714=VECTOR('',#16282,1.);
#9715=VECTOR('',#16285,1.);
#9716=VECTOR('',#16286,1.);
#9717=VECTOR('',#16291,1.);
#9718=VECTOR('',#16292,1.);
#9719=VECTOR('',#16293,1.);
#9720=VECTOR('',#16414,1.);
#9721=VECTOR('',#16415,1.);
#9722=VECTOR('',#16422,1.);
#9723=VECTOR('',#16427,1.);
#9724=VECTOR('',#16430,1.);
#9725=VECTOR('',#16433,1.);
#9726=VECTOR('',#16440,1.);
#9727=VECTOR('',#16441,1.);
#9728=VECTOR('',#16444,1.);
#9729=VECTOR('',#16445,1.);
#9730=VECTOR('',#16446,1.);
#9731=VECTOR('',#16587,1.);
#9732=VECTOR('',#16588,1.);
#9733=VECTOR('',#16589,1.);
#9734=VECTOR('',#16590,1.);
#9735=VECTOR('',#16593,1.);
#9736=VECTOR('',#16594,1.);
#9737=VECTOR('',#16597,1.);
#9738=VECTOR('',#16598,1.);
#9739=VECTOR('',#16601,1.);
#9740=VECTOR('',#16610,1.);
#9741=VECTOR('',#16613,1.);
#9742=VECTOR('',#16614,1.);
#9743=VECTOR('',#16617,1.);
#9744=VECTOR('',#16618,1.);
#9745=VECTOR('',#16621,1.);
#9746=VECTOR('',#16622,1.);
#9747=VECTOR('',#16625,1.);
#9748=VECTOR('',#16626,1.);
#9749=VECTOR('',#16629,1.);
#9750=VECTOR('',#16630,1.);
#9751=VECTOR('',#16633,1.);
#9752=VECTOR('',#16634,1.);
#9753=VECTOR('',#16637,1.);
#9754=VECTOR('',#16638,1.);
#9755=VECTOR('',#16641,1.);
#9756=VECTOR('',#16642,1.);
#9757=VECTOR('',#16645,1.);
#9758=VECTOR('',#16646,1.);
#9759=VECTOR('',#16649,1.);
#9760=VECTOR('',#16650,1.);
#9761=VECTOR('',#16653,1.);
#9762=VECTOR('',#16654,1.);
#9763=VECTOR('',#16657,1.);
#9764=VECTOR('',#16658,1.);
#9765=VECTOR('',#16661,1.);
#9766=VECTOR('',#16662,1.);
#9767=VECTOR('',#16665,1.);
#9768=VECTOR('',#16666,1.);
#9769=VECTOR('',#16669,1.);
#9770=VECTOR('',#16670,1.);
#9771=VECTOR('',#16673,1.);
#9772=VECTOR('',#16674,1.);
#9773=VECTOR('',#16677,1.);
#9774=VECTOR('',#16678,1.);
#9775=VECTOR('',#16681,1.);
#9776=VECTOR('',#16682,1.);
#9777=VECTOR('',#16685,1.);
#9778=VECTOR('',#16686,1.);
#9779=VECTOR('',#16689,1.);
#9780=VECTOR('',#16690,1.);
#9781=VECTOR('',#16693,1.);
#9782=VECTOR('',#16694,1.);
#9783=VECTOR('',#16697,1.);
#9784=VECTOR('',#16698,1.);
#9785=VECTOR('',#16701,1.);
#9786=VECTOR('',#16702,1.);
#9787=VECTOR('',#16705,1.);
#9788=VECTOR('',#16706,1.);
#9789=VECTOR('',#16709,1.);
#9790=VECTOR('',#16710,1.);
#9791=VECTOR('',#16713,1.);
#9792=VECTOR('',#16714,1.);
#9793=VECTOR('',#16717,1.);
#9794=VECTOR('',#16718,1.);
#9795=VECTOR('',#16721,1.);
#9796=VECTOR('',#16722,1.);
#9797=VECTOR('',#16725,1.);
#9798=VECTOR('',#16726,1.);
#9799=VECTOR('',#16729,1.);
#9800=VECTOR('',#16730,1.);
#9801=VECTOR('',#16733,1.);
#9802=VECTOR('',#16734,1.);
#9803=VECTOR('',#16737,1.);
#9804=VECTOR('',#16738,1.);
#9805=VECTOR('',#16741,1.);
#9806=VECTOR('',#16742,1.);
#9807=VECTOR('',#16745,1.);
#9808=VECTOR('',#16746,1.);
#9809=VECTOR('',#16749,1.);
#9810=VECTOR('',#16750,1.);
#9811=VECTOR('',#16753,1.);
#9812=VECTOR('',#16754,1.);
#9813=VECTOR('',#16757,1.);
#9814=VECTOR('',#16758,1.);
#9815=VECTOR('',#16761,1.);
#9816=VECTOR('',#16762,1.);
#9817=VECTOR('',#16765,1.);
#9818=VECTOR('',#16766,1.);
#9819=VECTOR('',#16769,1.);
#9820=VECTOR('',#16770,1.);
#9821=VECTOR('',#16773,1.);
#9822=VECTOR('',#16774,1.);
#9823=VECTOR('',#16777,1.);
#9824=VECTOR('',#16778,1.);
#9825=VECTOR('',#16781,1.);
#9826=VECTOR('',#16782,1.);
#9827=VECTOR('',#16783,1.);
#9828=VECTOR('',#16784,1.);
#9829=VECTOR('',#16787,1.);
#9830=VECTOR('',#16788,1.);
#9831=VECTOR('',#16791,1.);
#9832=VECTOR('',#16792,1.);
#9833=VECTOR('',#16795,1.);
#9834=VECTOR('',#16796,1.);
#9835=VECTOR('',#16799,1.);
#9836=VECTOR('',#16804,1.);
#9837=VECTOR('',#16805,1.);
#9838=VECTOR('',#16808,1.);
#9839=VECTOR('',#16809,1.);
#9840=VECTOR('',#16812,1.);
#9841=VECTOR('',#16813,1.);
#9842=VECTOR('',#16816,1.);
#9843=VECTOR('',#16817,1.);
#9844=VECTOR('',#16820,1.);
#9845=VECTOR('',#16821,1.);
#9846=VECTOR('',#16822,1.);
#9847=VECTOR('',#16823,1.);
#9848=VECTOR('',#16826,1.);
#9849=VECTOR('',#16827,1.);
#9850=VECTOR('',#16830,1.);
#9851=VECTOR('',#16831,1.);
#9852=VECTOR('',#16834,1.);
#9853=VECTOR('',#16835,1.);
#9854=VECTOR('',#16838,1.);
#9855=VECTOR('',#16839,1.);
#9856=VECTOR('',#16842,1.);
#9857=VECTOR('',#16843,1.);
#9858=VECTOR('',#16846,1.);
#9859=VECTOR('',#16847,1.);
#9860=VECTOR('',#16850,1.);
#9861=VECTOR('',#16851,1.);
#9862=VECTOR('',#16854,1.);
#9863=VECTOR('',#16855,1.);
#9864=VECTOR('',#16858,1.);
#9865=VECTOR('',#16859,1.);
#9866=VECTOR('',#16862,1.);
#9867=VECTOR('',#16863,1.);
#9868=VECTOR('',#16866,1.);
#9869=VECTOR('',#16867,1.);
#9870=VECTOR('',#16870,1.);
#9871=VECTOR('',#16871,1.);
#9872=VECTOR('',#16874,1.);
#9873=VECTOR('',#16875,1.);
#9874=VECTOR('',#16878,1.);
#9875=VECTOR('',#16879,1.);
#9876=VECTOR('',#16882,1.);
#9877=VECTOR('',#16883,1.);
#9878=VECTOR('',#16886,1.);
#9879=VECTOR('',#16887,1.);
#9880=VECTOR('',#16890,1.);
#9881=VECTOR('',#16891,1.);
#9882=VECTOR('',#16894,1.);
#9883=VECTOR('',#16895,1.);
#9884=VECTOR('',#16898,1.);
#9885=VECTOR('',#16899,1.);
#9886=VECTOR('',#16902,1.);
#9887=VECTOR('',#16903,1.);
#9888=VECTOR('',#16906,1.);
#9889=VECTOR('',#16907,1.);
#9890=VECTOR('',#16910,1.);
#9891=VECTOR('',#16911,1.);
#9892=VECTOR('',#16914,1.);
#9893=VECTOR('',#16915,1.);
#9894=VECTOR('',#16918,1.);
#9895=VECTOR('',#16919,1.);
#9896=VECTOR('',#16922,1.);
#9897=VECTOR('',#16923,1.);
#9898=VECTOR('',#16926,1.);
#9899=VECTOR('',#16927,1.);
#9900=VECTOR('',#16930,1.);
#9901=VECTOR('',#16931,1.);
#9902=VECTOR('',#16934,1.);
#9903=VECTOR('',#16935,1.);
#9904=VECTOR('',#16938,1.);
#9905=VECTOR('',#16939,1.);
#9906=VECTOR('',#16942,1.);
#9907=VECTOR('',#16943,1.);
#9908=VECTOR('',#16946,1.);
#9909=VECTOR('',#16947,1.);
#9910=VECTOR('',#16950,1.);
#9911=VECTOR('',#16951,1.);
#9912=VECTOR('',#16954,1.);
#9913=VECTOR('',#16955,1.);
#9914=VECTOR('',#16958,1.);
#9915=VECTOR('',#16959,1.);
#9916=VECTOR('',#16962,1.);
#9917=VECTOR('',#16963,1.);
#9918=VECTOR('',#16966,1.);
#9919=VECTOR('',#16967,1.);
#9920=VECTOR('',#16970,1.);
#9921=VECTOR('',#16971,1.);
#9922=VECTOR('',#16974,1.);
#9923=VECTOR('',#16975,1.);
#9924=VECTOR('',#16978,1.);
#9925=VECTOR('',#16979,1.);
#9926=VECTOR('',#16982,1.);
#9927=VECTOR('',#16983,1.);
#9928=VECTOR('',#16986,1.);
#9929=VECTOR('',#16987,1.);
#9930=VECTOR('',#16990,1.);
#9931=VECTOR('',#16991,1.);
#9932=VECTOR('',#16998,1.);
#9933=VECTOR('',#16999,1.);
#9934=VECTOR('',#17002,1.);
#9935=VECTOR('',#17005,1.);
#9936=VECTOR('',#17008,1.);
#9937=VECTOR('',#17011,1.);
#9938=VECTOR('',#17014,1.);
#9939=VECTOR('',#17017,1.);
#9940=VECTOR('',#17020,1.);
#9941=VECTOR('',#17023,1.);
#9942=VECTOR('',#17026,1.);
#9943=VECTOR('',#17029,1.);
#9944=VECTOR('',#17032,1.);
#9945=VECTOR('',#17035,1.);
#9946=VECTOR('',#17038,1.);
#9947=VECTOR('',#17041,1.);
#9948=VECTOR('',#17044,1.);
#9949=VECTOR('',#17047,1.);
#9950=VECTOR('',#17050,1.);
#9951=VECTOR('',#17053,1.);
#9952=VECTOR('',#17056,1.);
#9953=VECTOR('',#17059,1.);
#9954=VECTOR('',#17062,1.);
#9955=VECTOR('',#17065,1.);
#9956=VECTOR('',#17068,1.);
#9957=VECTOR('',#17071,1.);
#9958=VECTOR('',#17074,1.);
#9959=VECTOR('',#17077,1.);
#9960=VECTOR('',#17080,1.);
#9961=VECTOR('',#17083,1.);
#9962=VECTOR('',#17086,1.);
#9963=VECTOR('',#17089,1.);
#9964=VECTOR('',#17092,1.);
#9965=VECTOR('',#17095,1.);
#9966=VECTOR('',#17098,1.);
#9967=VECTOR('',#17101,1.);
#9968=VECTOR('',#17104,1.);
#9969=VECTOR('',#17107,1.);
#9970=VECTOR('',#17110,1.);
#9971=VECTOR('',#17113,1.);
#9972=VECTOR('',#17116,1.);
#9973=VECTOR('',#17119,1.);
#9974=VECTOR('',#17122,1.);
#9975=VECTOR('',#17125,1.);
#9976=VECTOR('',#17128,1.);
#9977=VECTOR('',#17131,1.);
#9978=VECTOR('',#17134,1.);
#9979=VECTOR('',#17137,1.);
#9980=VECTOR('',#17140,1.);
#9981=VECTOR('',#17143,1.);
#9982=VECTOR('',#17146,1.);
#9983=VECTOR('',#17149,1.);
#9984=VECTOR('',#17152,1.);
#9985=VECTOR('',#17155,1.);
#9986=VECTOR('',#17158,1.);
#9987=VECTOR('',#17161,1.);
#9988=VECTOR('',#17164,1.);
#9989=VECTOR('',#17167,1.);
#9990=VECTOR('',#17170,1.);
#9991=VECTOR('',#17173,1.);
#9992=VECTOR('',#17176,1.);
#9993=VECTOR('',#17179,1.);
#9994=VECTOR('',#17182,1.);
#9995=VECTOR('',#17185,1.);
#9996=VECTOR('',#17188,1.);
#9997=VECTOR('',#17191,1.);
#9998=VECTOR('',#17194,1.);
#9999=VECTOR('',#17197,1.);
#10000=VECTOR('',#17200,1.);
#10001=VECTOR('',#17203,1.);
#10002=VECTOR('',#17206,1.);
#10003=VECTOR('',#17209,1.);
#10004=VECTOR('',#17212,1.);
#10005=VECTOR('',#17215,1.);
#10006=VECTOR('',#17218,1.);
#10007=VECTOR('',#17221,1.);
#10008=VECTOR('',#17224,1.);
#10009=VECTOR('',#17227,1.);
#10010=VECTOR('',#17230,1.);
#10011=VECTOR('',#17233,1.);
#10012=VECTOR('',#17236,1.);
#10013=VECTOR('',#17239,1.);
#10014=VECTOR('',#17242,1.);
#10015=VECTOR('',#17245,1.);
#10016=VECTOR('',#17248,1.);
#10017=VECTOR('',#17251,1.);
#10018=VECTOR('',#17254,1.);
#10019=VECTOR('',#17257,1.);
#10020=VECTOR('',#17260,1.);
#10021=VECTOR('',#17263,1.);
#10022=VECTOR('',#17266,1.);
#10023=VECTOR('',#17269,1.);
#10024=VECTOR('',#17272,1.);
#10025=VECTOR('',#17275,1.);
#10026=VECTOR('',#17278,1.);
#10027=VECTOR('',#17281,1.);
#10028=VECTOR('',#17284,1.);
#10029=VECTOR('',#17287,1.);
#10030=VECTOR('',#17290,1.);
#10031=VECTOR('',#17293,1.);
#10032=VECTOR('',#17296,1.);
#10033=VECTOR('',#17299,1.);
#10034=VECTOR('',#17302,1.);
#10035=VECTOR('',#17305,1.);
#10036=VECTOR('',#17308,1.);
#10037=VECTOR('',#17311,1.);
#10038=VECTOR('',#17314,1.);
#10039=VECTOR('',#17317,1.);
#10040=VECTOR('',#17320,1.);
#10041=VECTOR('',#17323,1.);
#10042=VECTOR('',#17326,1.);
#10043=VECTOR('',#17329,1.);
#10044=VECTOR('',#17332,1.);
#10045=VECTOR('',#17335,1.);
#10046=VECTOR('',#17338,1.);
#10047=VECTOR('',#17341,1.);
#10048=VECTOR('',#17344,1.);
#10049=VECTOR('',#17347,1.);
#10050=VECTOR('',#17350,1.);
#10051=VECTOR('',#17353,1.);
#10052=VECTOR('',#17356,1.);
#10053=VECTOR('',#17359,1.);
#10054=VECTOR('',#17362,1.);
#10055=VECTOR('',#17365,1.);
#10056=VECTOR('',#17368,1.);
#10057=VECTOR('',#17371,1.);
#10058=VECTOR('',#17374,1.);
#10059=VECTOR('',#17377,1.);
#10060=VECTOR('',#17380,1.);
#10061=VECTOR('',#17383,1.);
#10062=VECTOR('',#17386,1.);
#10063=VECTOR('',#17389,1.);
#10064=VECTOR('',#17392,1.);
#10065=VECTOR('',#17395,1.);
#10066=VECTOR('',#17398,1.);
#10067=VECTOR('',#17401,1.);
#10068=VECTOR('',#17404,1.);
#10069=VECTOR('',#17407,1.);
#10070=VECTOR('',#17410,1.);
#10071=VECTOR('',#17413,1.);
#10072=VECTOR('',#17416,1.);
#10073=VECTOR('',#17419,1.);
#10074=VECTOR('',#17422,1.);
#10075=VECTOR('',#17501,1.);
#10076=VECTOR('',#17502,1.);
#10077=VECTOR('',#17507,1.);
#10078=VECTOR('',#17508,1.);
#10079=VECTOR('',#17523,1.);
#10080=VECTOR('',#17524,1.);
#10081=VECTOR('',#17529,1.);
#10082=VECTOR('',#17530,1.);
#10083=VECTOR('',#17573,1.);
#10084=VECTOR('',#17574,1.);
#10085=VECTOR('',#17575,1.);
#10086=VECTOR('',#17576,1.);
#10087=VECTOR('',#17581,1.);
#10088=VECTOR('',#17586,1.);
#10089=VECTOR('',#17587,1.);
#10090=VECTOR('',#17588,1.);
#10091=VECTOR('',#17591,1.);
#10092=VECTOR('',#17592,1.);
#10093=VECTOR('',#17593,1.);
#10094=VECTOR('',#17594,1.);
#10095=VECTOR('',#17597,1.);
#10096=VECTOR('',#17598,1.);
#10097=VECTOR('',#17599,1.);
#10098=VECTOR('',#17600,1.);
#10099=VECTOR('',#17609,1.);
#10100=VECTOR('',#17610,1.);
#10101=VECTOR('',#17611,1.);
#10102=VECTOR('',#17612,1.);
#10103=VECTOR('',#17615,1.);
#10104=VECTOR('',#17616,1.);
#10105=VECTOR('',#17617,1.);
#10106=VECTOR('',#17618,1.);
#10107=VECTOR('',#17731,1.);
#10108=VECTOR('',#17734,1.);
#10109=VECTOR('',#17737,1.);
#10110=VECTOR('',#17738,1.);
#10111=VECTOR('',#17739,1.);
#10112=VECTOR('',#17742,1.);
#10113=VECTOR('',#17743,1.);
#10114=VECTOR('',#17744,1.);
#10115=VECTOR('',#17753,1.);
#10116=VECTOR('',#17756,1.);
#10117=VECTOR('',#17759,1.);
#10118=VECTOR('',#17760,1.);
#10119=VECTOR('',#17761,1.);
#10120=VECTOR('',#17764,1.);
#10121=VECTOR('',#17765,1.);
#10122=VECTOR('',#17766,1.);
#10123=VECTOR('',#17775,1.);
#10124=VECTOR('',#17778,1.);
#10125=VECTOR('',#17781,1.);
#10126=VECTOR('',#17782,1.);
#10127=VECTOR('',#17783,1.);
#10128=VECTOR('',#17786,1.);
#10129=VECTOR('',#17787,1.);
#10130=VECTOR('',#17788,1.);
#10131=VECTOR('',#17825,1.);
#10132=VECTOR('',#17826,1.);
#10133=VECTOR('',#17827,1.);
#10134=VECTOR('',#17828,1.);
#10135=VECTOR('',#17831,1.);
#10136=VECTOR('',#17832,1.);
#10137=VECTOR('',#17833,1.);
#10138=VECTOR('',#17834,1.);
#10139=VECTOR('',#17837,1.);
#10140=VECTOR('',#17838,1.);
#10141=VECTOR('',#17839,1.);
#10142=VECTOR('',#17840,1.);
#10143=VECTOR('',#17843,1.);
#10144=VECTOR('',#17844,1.);
#10145=VECTOR('',#17845,1.);
#10146=VECTOR('',#17846,1.);
#10147=VECTOR('',#17861,1.);
#10148=VECTOR('',#17862,1.);
#10149=VECTOR('',#17867,1.);
#10150=VECTOR('',#17868,1.);
#10151=VECTOR('',#17883,1.);
#10152=VECTOR('',#17884,1.);
#10153=VECTOR('',#17889,1.);
#10154=VECTOR('',#17890,1.);
#10155=VECTOR('',#17951,1.);
#10156=VECTOR('',#17954,1.);
#10157=VECTOR('',#17961,1.);
#10158=VECTOR('',#17964,1.);
#10159=VECTOR('',#17969,1.);
#10160=VECTOR('',#17974,1.);
#10161=VECTOR('',#17975,1.);
#10162=VECTOR('',#17982,1.);
#10163=VECTOR('',#17985,1.);
#10164=VECTOR('',#17988,1.);
#10165=VECTOR('',#17995,1.);
#10166=VECTOR('',#17998,1.);
#10167=VECTOR('',#18005,1.);
#10168=VECTOR('',#18010,1.);
#10169=VECTOR('',#18011,1.);
#10170=VECTOR('',#18018,1.);
#10171=VECTOR('',#18023,1.);
#10172=VECTOR('',#18026,1.);
#10173=VECTOR('',#18029,1.);
#10174=VECTOR('',#18030,1.);
#10175=VECTOR('',#18037,1.);
#10176=VECTOR('',#18040,1.);
#10177=VECTOR('',#18047,1.);
#10178=VECTOR('',#18054,1.);
#10179=VECTOR('',#18061,1.);
#10180=VECTOR('',#18064,1.);
#10181=VECTOR('',#18071,1.);
#10182=VECTOR('',#18074,1.);
#10183=VECTOR('',#18081,1.);
#10184=VECTOR('',#18086,1.);
#10185=VECTOR('',#18087,1.);
#10186=VECTOR('',#18094,1.);
#10187=VECTOR('',#18099,1.);
#10188=VECTOR('',#18102,1.);
#10189=VECTOR('',#18105,1.);
#10190=VECTOR('',#18106,1.);
#10191=VECTOR('',#18109,1.);
#10192=VECTOR('',#18112,1.);
#10193=VECTOR('',#18115,1.);
#10194=VECTOR('',#18118,1.);
#10195=VECTOR('',#18123,1.);
#10196=VECTOR('',#18124,1.);
#10197=VECTOR('',#18127,1.);
#10198=VECTOR('',#18130,1.);
#10199=VECTOR('',#18137,1.);
#10200=VECTOR('',#18138,1.);
#10201=VECTOR('',#18141,1.);
#10202=VECTOR('',#18144,1.);
#10203=VECTOR('',#18147,1.);
#10204=VECTOR('',#18150,1.);
#10205=VECTOR('',#18153,1.);
#10206=VECTOR('',#18154,1.);
#10207=VECTOR('',#18157,1.);
#10208=VECTOR('',#18160,1.);
#10209=VECTOR('',#18169,1.);
#10210=VECTOR('',#18170,1.);
#10211=VECTOR('',#18171,1.);
#10212=VECTOR('',#18172,1.);
#10213=VECTOR('',#18175,1.);
#10214=VECTOR('',#18176,1.);
#10215=VECTOR('',#18179,1.);
#10216=VECTOR('',#18182,1.);
#10217=VECTOR('',#18301,1.);
#10218=VECTOR('',#18304,1.);
#10219=VECTOR('',#18315,1.);
#10220=VECTOR('',#18318,1.);
#10221=VECTOR('',#18321,1.);
#10222=VECTOR('',#18322,1.);
#10223=VECTOR('',#18323,1.);
#10224=VECTOR('',#18326,1.);
#10225=VECTOR('',#18327,1.);
#10226=VECTOR('',#18328,1.);
#10227=VECTOR('',#18337,1.);
#10228=VECTOR('',#18340,1.);
#10229=VECTOR('',#18343,1.);
#10230=VECTOR('',#18344,1.);
#10231=VECTOR('',#18345,1.);
#10232=VECTOR('',#18348,1.);
#10233=VECTOR('',#18349,1.);
#10234=VECTOR('',#18350,1.);
#10235=VECTOR('',#18359,1.);
#10236=VECTOR('',#18362,1.);
#10237=VECTOR('',#18365,1.);
#10238=VECTOR('',#18366,1.);
#10239=VECTOR('',#18367,1.);
#10240=VECTOR('',#18370,1.);
#10241=VECTOR('',#18371,1.);
#10242=VECTOR('',#18372,1.);
#10243=VECTOR('',#18431,1.);
#10244=VECTOR('',#18432,1.);
#10245=VECTOR('',#18433,1.);
#10246=VECTOR('',#18434,1.);
#10247=VECTOR('',#18435,1.);
#10248=VECTOR('',#18436,1.);
#10249=VECTOR('',#18439,1.);
#10250=VECTOR('',#18442,1.);
#10251=VECTOR('',#18445,1.);
#10252=VECTOR('',#18446,1.);
#10253=VECTOR('',#18447,1.);
#10254=VECTOR('',#18448,1.);
#10255=VECTOR('',#18451,1.);
#10256=VECTOR('',#18452,1.);
#10257=VECTOR('',#18453,1.);
#10258=VECTOR('',#18456,1.);
#10259=VECTOR('',#18457,1.);
#10260=VECTOR('',#18458,1.);
#10261=VECTOR('',#18461,1.);
#10262=VECTOR('',#18462,1.);
#10263=VECTOR('',#18463,1.);
#10264=VECTOR('',#18464,1.);
#10265=VECTOR('',#18467,1.);
#10266=VECTOR('',#18468,1.);
#10267=VECTOR('',#18469,1.);
#10268=VECTOR('',#18472,1.);
#10269=VECTOR('',#18473,1.);
#10270=VECTOR('',#18474,1.);
#10271=VECTOR('',#18477,1.);
#10272=VECTOR('',#18478,1.);
#10273=VECTOR('',#18479,1.);
#10274=VECTOR('',#18480,1.);
#10275=VECTOR('',#18483,1.);
#10276=VECTOR('',#18484,1.);
#10277=VECTOR('',#18485,1.);
#10278=VECTOR('',#18488,1.);
#10279=VECTOR('',#18489,1.);
#10280=VECTOR('',#18490,1.);
#10281=VECTOR('',#18493,1.);
#10282=VECTOR('',#18494,1.);
#10283=VECTOR('',#18495,1.);
#10284=VECTOR('',#18496,1.);
#10285=VECTOR('',#18499,1.);
#10286=VECTOR('',#18500,1.);
#10287=VECTOR('',#18501,1.);
#10288=VECTOR('',#18504,1.);
#10289=VECTOR('',#18505,1.);
#10290=VECTOR('',#18506,1.);
#10291=VECTOR('',#18509,1.);
#10292=VECTOR('',#18510,1.);
#10293=VECTOR('',#18511,1.);
#10294=VECTOR('',#18512,1.);
#10295=VECTOR('',#18515,1.);
#10296=VECTOR('',#18516,1.);
#10297=VECTOR('',#18517,1.);
#10298=VECTOR('',#18520,1.);
#10299=VECTOR('',#18521,1.);
#10300=VECTOR('',#18522,1.);
#10301=VECTOR('',#18525,1.);
#10302=VECTOR('',#18526,1.);
#10303=VECTOR('',#18527,1.);
#10304=VECTOR('',#18528,1.);
#10305=VECTOR('',#18531,1.);
#10306=VECTOR('',#18532,1.);
#10307=VECTOR('',#18533,1.);
#10308=VECTOR('',#18536,1.);
#10309=VECTOR('',#18537,1.);
#10310=VECTOR('',#18538,1.);
#10311=VECTOR('',#18541,1.);
#10312=VECTOR('',#18542,1.);
#10313=VECTOR('',#18543,1.);
#10314=VECTOR('',#18544,1.);
#10315=VECTOR('',#18547,1.);
#10316=VECTOR('',#18548,1.);
#10317=VECTOR('',#18549,1.);
#10318=VECTOR('',#18552,1.);
#10319=VECTOR('',#18553,1.);
#10320=VECTOR('',#18554,1.);
#10321=VECTOR('',#18557,1.);
#10322=VECTOR('',#18558,1.);
#10323=VECTOR('',#18559,1.);
#10324=VECTOR('',#18560,1.);
#10325=VECTOR('',#18563,1.);
#10326=VECTOR('',#18564,1.);
#10327=VECTOR('',#18565,1.);
#10328=VECTOR('',#18568,1.);
#10329=VECTOR('',#18569,1.);
#10330=VECTOR('',#18570,1.);
#10331=VECTOR('',#18573,1.);
#10332=VECTOR('',#18574,1.);
#10333=VECTOR('',#18575,1.);
#10334=VECTOR('',#18576,1.);
#10335=VECTOR('',#18579,1.);
#10336=VECTOR('',#18580,1.);
#10337=VECTOR('',#18581,1.);
#10338=VECTOR('',#18584,1.);
#10339=VECTOR('',#18585,1.);
#10340=VECTOR('',#18586,1.);
#10341=VECTOR('',#18589,1.);
#10342=VECTOR('',#18590,1.);
#10343=VECTOR('',#18591,1.);
#10344=VECTOR('',#18592,1.);
#10345=VECTOR('',#18595,1.);
#10346=VECTOR('',#18596,1.);
#10347=VECTOR('',#18597,1.);
#10348=VECTOR('',#18600,1.);
#10349=VECTOR('',#18601,1.);
#10350=VECTOR('',#18602,1.);
#10351=VECTOR('',#18605,1.);
#10352=VECTOR('',#18606,1.);
#10353=VECTOR('',#18607,1.);
#10354=VECTOR('',#18608,1.);
#10355=VECTOR('',#18611,1.);
#10356=VECTOR('',#18612,1.);
#10357=VECTOR('',#18613,1.);
#10358=VECTOR('',#18616,1.);
#10359=VECTOR('',#18617,1.);
#10360=VECTOR('',#18618,1.);
#10361=VECTOR('',#18721,1.);
#10362=VECTOR('',#18722,1.);
#10363=VECTOR('',#18727,1.);
#10364=VECTOR('',#18728,1.);
#10365=VECTOR('',#18743,1.);
#10366=VECTOR('',#18744,1.);
#10367=VECTOR('',#18749,1.);
#10368=VECTOR('',#18750,1.);
#10369=VECTOR('',#18753,1.);
#10370=VECTOR('',#18760,1.);
#10371=VECTOR('',#18763,1.);
#10372=VECTOR('',#18764,1.);
#10373=VECTOR('',#18765,1.);
#10374=VECTOR('',#18766,1.);
#10375=VECTOR('',#18769,1.);
#10376=VECTOR('',#18770,1.);
#10377=VECTOR('',#18773,1.);
#10378=VECTOR('',#18776,1.);
#10379=VECTOR('',#18779,1.);
#10380=VECTOR('',#18782,1.);
#10381=VECTOR('',#18793,1.);
#10382=VECTOR('',#18796,1.);
#10383=VECTOR('',#18797,1.);
#10384=VECTOR('',#18800,1.);
#10385=VECTOR('',#18807,1.);
#10386=VECTOR('',#18810,1.);
#10387=VECTOR('',#18813,1.);
#10388=VECTOR('',#18816,1.);
#10389=VECTOR('',#18861,1.);
#10390=VECTOR('',#18862,1.);
#10391=VECTOR('',#18863,1.);
#10392=VECTOR('',#18864,1.);
#10393=VECTOR('',#18865,1.);
#10394=VECTOR('',#18870,1.);
#10395=VECTOR('',#18875,1.);
#10396=VECTOR('',#18876,1.);
#10397=VECTOR('',#18877,1.);
#10398=VECTOR('',#18878,1.);
#10399=VECTOR('',#18887,1.);
#10400=VECTOR('',#18888,1.);
#10401=VECTOR('',#18889,1.);
#10402=VECTOR('',#18890,1.);
#10403=VECTOR('',#18891,1.);
#10404=VECTOR('',#18896,1.);
#10405=VECTOR('',#18901,1.);
#10406=VECTOR('',#18902,1.);
#10407=VECTOR('',#18903,1.);
#10408=VECTOR('',#18904,1.);
#10409=VECTOR('',#18913,1.);
#10410=VECTOR('',#18914,1.);
#10411=VECTOR('',#18915,1.);
#10412=VECTOR('',#18916,1.);
#10413=VECTOR('',#18917,1.);
#10414=VECTOR('',#18922,1.);
#10415=VECTOR('',#18927,1.);
#10416=VECTOR('',#18928,1.);
#10417=VECTOR('',#18929,1.);
#10418=VECTOR('',#18930,1.);
#10419=VECTOR('',#18939,1.);
#10420=VECTOR('',#18940,1.);
#10421=VECTOR('',#18941,1.);
#10422=VECTOR('',#18942,1.);
#10423=VECTOR('',#18943,1.);
#10424=VECTOR('',#18948,1.);
#10425=VECTOR('',#18953,1.);
#10426=VECTOR('',#18954,1.);
#10427=VECTOR('',#18955,1.);
#10428=VECTOR('',#18956,1.);
#10429=EDGE_LOOP('',(#1966,#1967,#1968,#1969,#1970,#1971,#1972,#1973,#1974,
#1975));
#10430=EDGE_LOOP('',(#1976,#1977,#1978,#1979));
#10431=EDGE_LOOP('',(#1980,#1981,#1982,#1983));
#10432=EDGE_LOOP('',(#1984,#1985,#1986,#1987,#1988,#1989,#1990,#1991,#1992,
#1993,#1994));
#10433=EDGE_LOOP('',(#1995,#1996,#1997,#1998,#1999));
#10434=EDGE_LOOP('',(#2000));
#10435=EDGE_LOOP('',(#2001,#2002,#2003));
#10436=EDGE_LOOP('',(#2004,#2005,#2006,#2007));
#10437=EDGE_LOOP('',(#2008,#2009));
#10438=EDGE_LOOP('',(#2010));
#10439=EDGE_LOOP('',(#2011));
#10440=EDGE_LOOP('',(#2012));
#10441=EDGE_LOOP('',(#2013,#2014,#2015,#2016));
#10442=EDGE_LOOP('',(#2017,#2018,#2019,#2020));
#10443=EDGE_LOOP('',(#2021,#2022,#2023,#2024));
#10444=EDGE_LOOP('',(#2025,#2026,#2027,#2028));
#10445=EDGE_LOOP('',(#2029,#2030,#2031,#2032));
#10446=EDGE_LOOP('',(#2033,#2034,#2035,#2036));
#10447=EDGE_LOOP('',(#2037,#2038,#2039,#2040));
#10448=EDGE_LOOP('',(#2041,#2042,#2043,#2044));
#10449=EDGE_LOOP('',(#2045,#2046,#2047,#2048));
#10450=EDGE_LOOP('',(#2049));
#10451=EDGE_LOOP('',(#2050));
#10452=EDGE_LOOP('',(#2051));
#10453=EDGE_LOOP('',(#2052));
#10454=EDGE_LOOP('',(#2053));
#10455=EDGE_LOOP('',(#2054));
#10456=EDGE_LOOP('',(#2055));
#10457=EDGE_LOOP('',(#2056));
#10458=EDGE_LOOP('',(#2057));
#10459=EDGE_LOOP('',(#2058));
#10460=EDGE_LOOP('',(#2059));
#10461=EDGE_LOOP('',(#2060));
#10462=EDGE_LOOP('',(#2061));
#10463=EDGE_LOOP('',(#2062));
#10464=EDGE_LOOP('',(#2063));
#10465=EDGE_LOOP('',(#2064));
#10466=EDGE_LOOP('',(#2065));
#10467=EDGE_LOOP('',(#2066,#2067,#2068,#2069));
#10468=EDGE_LOOP('',(#2070,#2071,#2072,#2073));
#10469=EDGE_LOOP('',(#2074,#2075,#2076,#2077));
#10470=EDGE_LOOP('',(#2078));
#10471=EDGE_LOOP('',(#2079));
#10472=EDGE_LOOP('',(#2080));
#10473=EDGE_LOOP('',(#2081));
#10474=EDGE_LOOP('',(#2082));
#10475=EDGE_LOOP('',(#2083));
#10476=EDGE_LOOP('',(#2084));
#10477=EDGE_LOOP('',(#2085));
#10478=EDGE_LOOP('',(#2086));
#10479=EDGE_LOOP('',(#2087));
#10480=EDGE_LOOP('',(#2088,#2089,#2090,#2091));
#10481=EDGE_LOOP('',(#2092,#2093,#2094,#2095));
#10482=EDGE_LOOP('',(#2096,#2097,#2098,#2099));
#10483=EDGE_LOOP('',(#2100));
#10484=EDGE_LOOP('',(#2101));
#10485=EDGE_LOOP('',(#2102));
#10486=EDGE_LOOP('',(#2103));
#10487=EDGE_LOOP('',(#2104));
#10488=EDGE_LOOP('',(#2105));
#10489=EDGE_LOOP('',(#2106));
#10490=EDGE_LOOP('',(#2107));
#10491=EDGE_LOOP('',(#2108));
#10492=EDGE_LOOP('',(#2109));
#10493=EDGE_LOOP('',(#2110));
#10494=EDGE_LOOP('',(#2111));
#10495=EDGE_LOOP('',(#2112));
#10496=EDGE_LOOP('',(#2113));
#10497=EDGE_LOOP('',(#2114));
#10498=EDGE_LOOP('',(#2115));
#10499=EDGE_LOOP('',(#2116));
#10500=EDGE_LOOP('',(#2117));
#10501=EDGE_LOOP('',(#2118));
#10502=EDGE_LOOP('',(#2119));
#10503=EDGE_LOOP('',(#2120));
#10504=EDGE_LOOP('',(#2121));
#10505=EDGE_LOOP('',(#2122));
#10506=EDGE_LOOP('',(#2123));
#10507=EDGE_LOOP('',(#2124));
#10508=EDGE_LOOP('',(#2125));
#10509=EDGE_LOOP('',(#2126));
#10510=EDGE_LOOP('',(#2127));
#10511=EDGE_LOOP('',(#2128));
#10512=EDGE_LOOP('',(#2129));
#10513=EDGE_LOOP('',(#2130));
#10514=EDGE_LOOP('',(#2131));
#10515=EDGE_LOOP('',(#2132));
#10516=EDGE_LOOP('',(#2133));
#10517=EDGE_LOOP('',(#2134));
#10518=EDGE_LOOP('',(#2135));
#10519=EDGE_LOOP('',(#2136));
#10520=EDGE_LOOP('',(#2137,#2138,#2139,#2140));
#10521=EDGE_LOOP('',(#2141,#2142,#2143,#2144));
#10522=EDGE_LOOP('',(#2145,#2146,#2147,#2148));
#10523=EDGE_LOOP('',(#2149));
#10524=EDGE_LOOP('',(#2150));
#10525=EDGE_LOOP('',(#2151));
#10526=EDGE_LOOP('',(#2152));
#10527=EDGE_LOOP('',(#2153,#2154,#2155,#2156,#2157,#2158,#2159,#2160,#2161,
#2162,#2163,#2164,#2165,#2166,#2167,#2168,#2169));
#10528=EDGE_LOOP('',(#2170,#2171));
#10529=EDGE_LOOP('',(#2172));
#10530=EDGE_LOOP('',(#2173));
#10531=EDGE_LOOP('',(#2174,#2175,#2176,#2177));
#10532=EDGE_LOOP('',(#2178));
#10533=EDGE_LOOP('',(#2179));
#10534=EDGE_LOOP('',(#2180));
#10535=EDGE_LOOP('',(#2181));
#10536=EDGE_LOOP('',(#2182,#2183,#2184,#2185,#2186,#2187,#2188,#2189,#2190));
#10537=EDGE_LOOP('',(#2191,#2192,#2193,#2194,#2195,#2196,#2197));
#10538=EDGE_LOOP('',(#2198,#2199,#2200,#2201));
#10539=EDGE_LOOP('',(#2202,#2203,#2204,#2205,#2206,#2207));
#10540=EDGE_LOOP('',(#2208,#2209,#2210,#2211));
#10541=EDGE_LOOP('',(#2212));
#10542=EDGE_LOOP('',(#2213));
#10543=EDGE_LOOP('',(#2214));
#10544=EDGE_LOOP('',(#2215));
#10545=EDGE_LOOP('',(#2216));
#10546=EDGE_LOOP('',(#2217));
#10547=EDGE_LOOP('',(#2218));
#10548=EDGE_LOOP('',(#2219));
#10549=EDGE_LOOP('',(#2220));
#10550=EDGE_LOOP('',(#2221));
#10551=EDGE_LOOP('',(#2222));
#10552=EDGE_LOOP('',(#2223));
#10553=EDGE_LOOP('',(#2224));
#10554=EDGE_LOOP('',(#2225));
#10555=EDGE_LOOP('',(#2226));
#10556=EDGE_LOOP('',(#2227));
#10557=EDGE_LOOP('',(#2228));
#10558=EDGE_LOOP('',(#2229));
#10559=EDGE_LOOP('',(#2230));
#10560=EDGE_LOOP('',(#2231));
#10561=EDGE_LOOP('',(#2232,#2233,#2234,#2235,#2236,#2237,#2238,#2239,#2240,
#2241,#2242));
#10562=EDGE_LOOP('',(#2243));
#10563=EDGE_LOOP('',(#2244));
#10564=EDGE_LOOP('',(#2245));
#10565=EDGE_LOOP('',(#2246));
#10566=EDGE_LOOP('',(#2247));
#10567=EDGE_LOOP('',(#2248));
#10568=EDGE_LOOP('',(#2249));
#10569=EDGE_LOOP('',(#2250));
#10570=EDGE_LOOP('',(#2251));
#10571=EDGE_LOOP('',(#2252));
#10572=EDGE_LOOP('',(#2253));
#10573=EDGE_LOOP('',(#2254));
#10574=EDGE_LOOP('',(#2255));
#10575=EDGE_LOOP('',(#2256));
#10576=EDGE_LOOP('',(#2257));
#10577=EDGE_LOOP('',(#2258));
#10578=EDGE_LOOP('',(#2259));
#10579=EDGE_LOOP('',(#2260));
#10580=EDGE_LOOP('',(#2261));
#10581=EDGE_LOOP('',(#2262));
#10582=EDGE_LOOP('',(#2263));
#10583=EDGE_LOOP('',(#2264));
#10584=EDGE_LOOP('',(#2265));
#10585=EDGE_LOOP('',(#2266));
#10586=EDGE_LOOP('',(#2267));
#10587=EDGE_LOOP('',(#2268));
#10588=EDGE_LOOP('',(#2269));
#10589=EDGE_LOOP('',(#2270));
#10590=EDGE_LOOP('',(#2271));
#10591=EDGE_LOOP('',(#2272));
#10592=EDGE_LOOP('',(#2273));
#10593=EDGE_LOOP('',(#2274));
#10594=EDGE_LOOP('',(#2275));
#10595=EDGE_LOOP('',(#2276));
#10596=EDGE_LOOP('',(#2277));
#10597=EDGE_LOOP('',(#2278,#2279,#2280));
#10598=EDGE_LOOP('',(#2281));
#10599=EDGE_LOOP('',(#2282));
#10600=EDGE_LOOP('',(#2283));
#10601=EDGE_LOOP('',(#2284));
#10602=EDGE_LOOP('',(#2285));
#10603=EDGE_LOOP('',(#2286));
#10604=EDGE_LOOP('',(#2287));
#10605=EDGE_LOOP('',(#2288));
#10606=EDGE_LOOP('',(#2289));
#10607=EDGE_LOOP('',(#2290));
#10608=EDGE_LOOP('',(#2291));
#10609=EDGE_LOOP('',(#2292));
#10610=EDGE_LOOP('',(#2293));
#10611=EDGE_LOOP('',(#2294));
#10612=EDGE_LOOP('',(#2295));
#10613=EDGE_LOOP('',(#2296,#2297));
#10614=EDGE_LOOP('',(#2298,#2299));
#10615=EDGE_LOOP('',(#2300,#2301));
#10616=EDGE_LOOP('',(#2302,#2303,#2304,#2305));
#10617=EDGE_LOOP('',(#2306,#2307,#2308,#2309));
#10618=EDGE_LOOP('',(#2310,#2311));
#10619=EDGE_LOOP('',(#2312,#2313,#2314,#2315));
#10620=EDGE_LOOP('',(#2316,#2317,#2318,#2319));
#10621=EDGE_LOOP('',(#2320,#2321,#2322,#2323));
#10622=EDGE_LOOP('',(#2324,#2325,#2326,#2327));
#10623=EDGE_LOOP('',(#2328,#2329,#2330,#2331));
#10624=EDGE_LOOP('',(#2332,#2333,#2334,#2335));
#10625=EDGE_LOOP('',(#2336,#2337,#2338,#2339));
#10626=EDGE_LOOP('',(#2340,#2341,#2342,#2343));
#10627=EDGE_LOOP('',(#2344,#2345,#2346,#2347));
#10628=EDGE_LOOP('',(#2348,#2349,#2350,#2351));
#10629=EDGE_LOOP('',(#2352,#2353,#2354,#2355,#2356,#2357,#2358));
#10630=EDGE_LOOP('',(#2359,#2360,#2361,#2362));
#10631=EDGE_LOOP('',(#2363,#2364,#2365,#2366));
#10632=EDGE_LOOP('',(#2367,#2368,#2369,#2370));
#10633=EDGE_LOOP('',(#2371,#2372,#2373,#2374));
#10634=EDGE_LOOP('',(#2375,#2376,#2377,#2378));
#10635=EDGE_LOOP('',(#2379,#2380,#2381,#2382,#2383,#2384,#2385,#2386));
#10636=EDGE_LOOP('',(#2387,#2388,#2389,#2390,#2391,#2392,#2393,#2394));
#10637=EDGE_LOOP('',(#2395,#2396,#2397,#2398,#2399,#2400,#2401,#2402));
#10638=EDGE_LOOP('',(#2403));
#10639=EDGE_LOOP('',(#2404,#2405,#2406,#2407,#2408,#2409,#2410,#2411,#2412,
#2413,#2414));
#10640=EDGE_LOOP('',(#2415));
#10641=EDGE_LOOP('',(#2416));
#10642=EDGE_LOOP('',(#2417));
#10643=EDGE_LOOP('',(#2418));
#10644=EDGE_LOOP('',(#2419));
#10645=EDGE_LOOP('',(#2420,#2421,#2422,#2423));
#10646=EDGE_LOOP('',(#2424,#2425,#2426,#2427));
#10647=EDGE_LOOP('',(#2428,#2429,#2430,#2431));
#10648=EDGE_LOOP('',(#2432,#2433,#2434,#2435));
#10649=EDGE_LOOP('',(#2436,#2437,#2438,#2439));
#10650=EDGE_LOOP('',(#2440,#2441,#2442,#2443));
#10651=EDGE_LOOP('',(#2444,#2445,#2446,#2447));
#10652=EDGE_LOOP('',(#2448,#2449,#2450,#2451));
#10653=EDGE_LOOP('',(#2452,#2453,#2454,#2455));
#10654=EDGE_LOOP('',(#2456,#2457,#2458,#2459));
#10655=EDGE_LOOP('',(#2460,#2461,#2462,#2463));
#10656=EDGE_LOOP('',(#2464,#2465,#2466,#2467));
#10657=EDGE_LOOP('',(#2468,#2469,#2470,#2471));
#10658=EDGE_LOOP('',(#2472,#2473,#2474,#2475));
#10659=EDGE_LOOP('',(#2476,#2477,#2478,#2479));
#10660=EDGE_LOOP('',(#2480,#2481,#2482,#2483));
#10661=EDGE_LOOP('',(#2484,#2485,#2486,#2487));
#10662=EDGE_LOOP('',(#2488,#2489,#2490,#2491));
#10663=EDGE_LOOP('',(#2492,#2493,#2494,#2495));
#10664=EDGE_LOOP('',(#2496,#2497,#2498,#2499));
#10665=EDGE_LOOP('',(#2500,#2501,#2502,#2503));
#10666=EDGE_LOOP('',(#2504,#2505,#2506,#2507));
#10667=EDGE_LOOP('',(#2508,#2509,#2510,#2511));
#10668=EDGE_LOOP('',(#2512,#2513,#2514,#2515));
#10669=EDGE_LOOP('',(#2516,#2517,#2518,#2519));
#10670=EDGE_LOOP('',(#2520,#2521,#2522,#2523));
#10671=EDGE_LOOP('',(#2524,#2525,#2526,#2527));
#10672=EDGE_LOOP('',(#2528,#2529,#2530,#2531));
#10673=EDGE_LOOP('',(#2532,#2533,#2534,#2535));
#10674=EDGE_LOOP('',(#2536,#2537,#2538,#2539));
#10675=EDGE_LOOP('',(#2540,#2541,#2542,#2543));
#10676=EDGE_LOOP('',(#2544,#2545,#2546,#2547));
#10677=EDGE_LOOP('',(#2548,#2549,#2550,#2551));
#10678=EDGE_LOOP('',(#2552,#2553,#2554,#2555));
#10679=EDGE_LOOP('',(#2556,#2557,#2558,#2559));
#10680=EDGE_LOOP('',(#2560,#2561,#2562,#2563));
#10681=EDGE_LOOP('',(#2564,#2565,#2566,#2567));
#10682=EDGE_LOOP('',(#2568,#2569,#2570,#2571));
#10683=EDGE_LOOP('',(#2572,#2573,#2574,#2575));
#10684=EDGE_LOOP('',(#2576,#2577,#2578,#2579));
#10685=EDGE_LOOP('',(#2580,#2581,#2582,#2583));
#10686=EDGE_LOOP('',(#2584,#2585,#2586,#2587));
#10687=EDGE_LOOP('',(#2588,#2589,#2590,#2591));
#10688=EDGE_LOOP('',(#2592,#2593,#2594,#2595));
#10689=EDGE_LOOP('',(#2596,#2597,#2598,#2599));
#10690=EDGE_LOOP('',(#2600,#2601,#2602,#2603));
#10691=EDGE_LOOP('',(#2604,#2605,#2606,#2607));
#10692=EDGE_LOOP('',(#2608,#2609,#2610,#2611));
#10693=EDGE_LOOP('',(#2612,#2613,#2614,#2615));
#10694=EDGE_LOOP('',(#2616,#2617,#2618,#2619));
#10695=EDGE_LOOP('',(#2620,#2621,#2622,#2623));
#10696=EDGE_LOOP('',(#2624,#2625,#2626,#2627));
#10697=EDGE_LOOP('',(#2628,#2629,#2630,#2631));
#10698=EDGE_LOOP('',(#2632,#2633,#2634,#2635));
#10699=EDGE_LOOP('',(#2636,#2637,#2638,#2639));
#10700=EDGE_LOOP('',(#2640));
#10701=EDGE_LOOP('',(#2641));
#10702=EDGE_LOOP('',(#2642));
#10703=EDGE_LOOP('',(#2643));
#10704=EDGE_LOOP('',(#2644));
#10705=EDGE_LOOP('',(#2645));
#10706=EDGE_LOOP('',(#2646,#2647,#2648,#2649,#2650,#2651,#2652));
#10707=EDGE_LOOP('',(#2653,#2654,#2655,#2656,#2657,#2658,#2659));
#10708=EDGE_LOOP('',(#2660,#2661,#2662,#2663));
#10709=EDGE_LOOP('',(#2664,#2665,#2666,#2667));
#10710=EDGE_LOOP('',(#2668,#2669,#2670,#2671));
#10711=EDGE_LOOP('',(#2672));
#10712=EDGE_LOOP('',(#2673));
#10713=EDGE_LOOP('',(#2674));
#10714=EDGE_LOOP('',(#2675));
#10715=EDGE_LOOP('',(#2676));
#10716=EDGE_LOOP('',(#2677,#2678,#2679,#2680,#2681,#2682,#2683,#2684,#2685,
#2686,#2687,#2688,#2689,#2690,#2691,#2692,#2693,#2694,#2695,#2696,#2697,
#2698,#2699));
#10717=EDGE_LOOP('',(#2700));
#10718=EDGE_LOOP('',(#2701,#2702,#2703,#2704));
#10719=EDGE_LOOP('',(#2705,#2706,#2707,#2708));
#10720=EDGE_LOOP('',(#2709,#2710,#2711,#2712));
#10721=EDGE_LOOP('',(#2713,#2714,#2715,#2716));
#10722=EDGE_LOOP('',(#2717,#2718,#2719,#2720));
#10723=EDGE_LOOP('',(#2721,#2722,#2723,#2724));
#10724=EDGE_LOOP('',(#2725,#2726,#2727,#2728));
#10725=EDGE_LOOP('',(#2729,#2730,#2731,#2732));
#10726=EDGE_LOOP('',(#2733,#2734,#2735,#2736));
#10727=EDGE_LOOP('',(#2737,#2738,#2739,#2740));
#10728=EDGE_LOOP('',(#2741,#2742,#2743,#2744));
#10729=EDGE_LOOP('',(#2745,#2746,#2747,#2748,#2749,#2750,#2751,#2752,#2753,
#2754,#2755,#2756,#2757,#2758,#2759,#2760,#2761,#2762,#2763,#2764,#2765,
#2766,#2767));
#10730=EDGE_LOOP('',(#2768));
#10731=EDGE_LOOP('',(#2769));
#10732=EDGE_LOOP('',(#2770));
#10733=EDGE_LOOP('',(#2771));
#10734=EDGE_LOOP('',(#2772,#2773,#2774,#2775,#2776,#2777,#2778,#2779,#2780,
#2781,#2782));
#10735=EDGE_LOOP('',(#2783));
#10736=EDGE_LOOP('',(#2784,#2785,#2786,#2787));
#10737=EDGE_LOOP('',(#2788));
#10738=EDGE_LOOP('',(#2789));
#10739=EDGE_LOOP('',(#2790));
#10740=EDGE_LOOP('',(#2791));
#10741=EDGE_LOOP('',(#2792));
#10742=EDGE_LOOP('',(#2793));
#10743=EDGE_LOOP('',(#2794));
#10744=EDGE_LOOP('',(#2795));
#10745=EDGE_LOOP('',(#2796));
#10746=EDGE_LOOP('',(#2797));
#10747=EDGE_LOOP('',(#2798));
#10748=EDGE_LOOP('',(#2799));
#10749=EDGE_LOOP('',(#2800,#2801,#2802,#2803));
#10750=EDGE_LOOP('',(#2804,#2805,#2806,#2807));
#10751=EDGE_LOOP('',(#2808));
#10752=EDGE_LOOP('',(#2809));
#10753=EDGE_LOOP('',(#2810));
#10754=EDGE_LOOP('',(#2811));
#10755=EDGE_LOOP('',(#2812,#2813,#2814,#2815));
#10756=EDGE_LOOP('',(#2816,#2817,#2818));
#10757=EDGE_LOOP('',(#2819,#2820,#2821));
#10758=EDGE_LOOP('',(#2822,#2823,#2824,#2825));
#10759=EDGE_LOOP('',(#2826,#2827,#2828));
#10760=EDGE_LOOP('',(#2829,#2830,#2831));
#10761=EDGE_LOOP('',(#2832,#2833,#2834,#2835));
#10762=EDGE_LOOP('',(#2836,#2837,#2838,#2839));
#10763=EDGE_LOOP('',(#2840,#2841,#2842,#2843));
#10764=EDGE_LOOP('',(#2844));
#10765=EDGE_LOOP('',(#2845));
#10766=EDGE_LOOP('',(#2846));
#10767=EDGE_LOOP('',(#2847,#2848,#2849));
#10768=EDGE_LOOP('',(#2850,#2851,#2852));
#10769=EDGE_LOOP('',(#2853,#2854,#2855));
#10770=EDGE_LOOP('',(#2856,#2857,#2858));
#10771=EDGE_LOOP('',(#2859,#2860,#2861,#2862,#2863,#2864,#2865,#2866,#2867,
#2868,#2869,#2870));
#10772=EDGE_LOOP('',(#2871));
#10773=EDGE_LOOP('',(#2872));
#10774=EDGE_LOOP('',(#2873));
#10775=EDGE_LOOP('',(#2874));
#10776=EDGE_LOOP('',(#2875));
#10777=EDGE_LOOP('',(#2876));
#10778=EDGE_LOOP('',(#2877));
#10779=EDGE_LOOP('',(#2878));
#10780=EDGE_LOOP('',(#2879));
#10781=EDGE_LOOP('',(#2880));
#10782=EDGE_LOOP('',(#2881));
#10783=EDGE_LOOP('',(#2882));
#10784=EDGE_LOOP('',(#2883));
#10785=EDGE_LOOP('',(#2884));
#10786=EDGE_LOOP('',(#2885));
#10787=EDGE_LOOP('',(#2886));
#10788=EDGE_LOOP('',(#2887));
#10789=EDGE_LOOP('',(#2888));
#10790=EDGE_LOOP('',(#2889));
#10791=EDGE_LOOP('',(#2890));
#10792=EDGE_LOOP('',(#2891));
#10793=EDGE_LOOP('',(#2892));
#10794=EDGE_LOOP('',(#2893));
#10795=EDGE_LOOP('',(#2894));
#10796=EDGE_LOOP('',(#2895));
#10797=EDGE_LOOP('',(#2896));
#10798=EDGE_LOOP('',(#2897));
#10799=EDGE_LOOP('',(#2898));
#10800=EDGE_LOOP('',(#2899));
#10801=EDGE_LOOP('',(#2900));
#10802=EDGE_LOOP('',(#2901));
#10803=EDGE_LOOP('',(#2902));
#10804=EDGE_LOOP('',(#2903));
#10805=EDGE_LOOP('',(#2904));
#10806=EDGE_LOOP('',(#2905));
#10807=EDGE_LOOP('',(#2906));
#10808=EDGE_LOOP('',(#2907));
#10809=EDGE_LOOP('',(#2908));
#10810=EDGE_LOOP('',(#2909));
#10811=EDGE_LOOP('',(#2910,#2911,#2912,#2913,#2914,#2915,#2916,#2917));
#10812=EDGE_LOOP('',(#2918,#2919,#2920,#2921,#2922));
#10813=EDGE_LOOP('',(#2923,#2924,#2925,#2926));
#10814=EDGE_LOOP('',(#2927,#2928,#2929,#2930));
#10815=EDGE_LOOP('',(#2931,#2932,#2933,#2934,#2935,#2936,#2937,#2938));
#10816=EDGE_LOOP('',(#2939,#2940,#2941,#2942));
#10817=EDGE_LOOP('',(#2943,#2944,#2945,#2946));
#10818=EDGE_LOOP('',(#2947,#2948,#2949,#2950));
#10819=EDGE_LOOP('',(#2951,#2952,#2953,#2954,#2955,#2956,#2957,#2958));
#10820=EDGE_LOOP('',(#2959,#2960,#2961,#2962,#2963));
#10821=EDGE_LOOP('',(#2964,#2965,#2966,#2967,#2968));
#10822=EDGE_LOOP('',(#2969,#2970,#2971,#2972));
#10823=EDGE_LOOP('',(#2973,#2974,#2975,#2976));
#10824=EDGE_LOOP('',(#2977,#2978,#2979));
#10825=EDGE_LOOP('',(#2980,#2981,#2982));
#10826=EDGE_LOOP('',(#2983));
#10827=EDGE_LOOP('',(#2984));
#10828=EDGE_LOOP('',(#2985));
#10829=EDGE_LOOP('',(#2986,#2987,#2988,#2989,#2990));
#10830=EDGE_LOOP('',(#2991,#2992));
#10831=EDGE_LOOP('',(#2993));
#10832=EDGE_LOOP('',(#2994));
#10833=EDGE_LOOP('',(#2995));
#10834=EDGE_LOOP('',(#2996));
#10835=EDGE_LOOP('',(#2997,#2998,#2999,#3000,#3001,#3002,#3003,#3004));
#10836=EDGE_LOOP('',(#3005));
#10837=EDGE_LOOP('',(#3006));
#10838=EDGE_LOOP('',(#3007));
#10839=EDGE_LOOP('',(#3008));
#10840=EDGE_LOOP('',(#3009,#3010,#3011,#3012,#3013,#3014,#3015,#3016,#3017,
#3018,#3019,#3020,#3021));
#10841=EDGE_LOOP('',(#3022));
#10842=EDGE_LOOP('',(#3023));
#10843=EDGE_LOOP('',(#3024));
#10844=EDGE_LOOP('',(#3025));
#10845=EDGE_LOOP('',(#3026));
#10846=EDGE_LOOP('',(#3027));
#10847=EDGE_LOOP('',(#3028));
#10848=EDGE_LOOP('',(#3029));
#10849=EDGE_LOOP('',(#3030));
#10850=EDGE_LOOP('',(#3031));
#10851=EDGE_LOOP('',(#3032));
#10852=EDGE_LOOP('',(#3033));
#10853=EDGE_LOOP('',(#3034));
#10854=EDGE_LOOP('',(#3035));
#10855=EDGE_LOOP('',(#3036));
#10856=EDGE_LOOP('',(#3037));
#10857=EDGE_LOOP('',(#3038));
#10858=EDGE_LOOP('',(#3039));
#10859=EDGE_LOOP('',(#3040));
#10860=EDGE_LOOP('',(#3041));
#10861=EDGE_LOOP('',(#3042));
#10862=EDGE_LOOP('',(#3043));
#10863=EDGE_LOOP('',(#3044));
#10864=EDGE_LOOP('',(#3045));
#10865=EDGE_LOOP('',(#3046));
#10866=EDGE_LOOP('',(#3047));
#10867=EDGE_LOOP('',(#3048));
#10868=EDGE_LOOP('',(#3049));
#10869=EDGE_LOOP('',(#3050));
#10870=EDGE_LOOP('',(#3051));
#10871=EDGE_LOOP('',(#3052));
#10872=EDGE_LOOP('',(#3053));
#10873=EDGE_LOOP('',(#3054));
#10874=EDGE_LOOP('',(#3055));
#10875=EDGE_LOOP('',(#3056));
#10876=EDGE_LOOP('',(#3057));
#10877=EDGE_LOOP('',(#3058));
#10878=EDGE_LOOP('',(#3059));
#10879=EDGE_LOOP('',(#3060));
#10880=EDGE_LOOP('',(#3061));
#10881=EDGE_LOOP('',(#3062));
#10882=EDGE_LOOP('',(#3063));
#10883=EDGE_LOOP('',(#3064));
#10884=EDGE_LOOP('',(#3065));
#10885=EDGE_LOOP('',(#3066));
#10886=EDGE_LOOP('',(#3067));
#10887=EDGE_LOOP('',(#3068));
#10888=EDGE_LOOP('',(#3069));
#10889=EDGE_LOOP('',(#3070,#3071,#3072,#3073,#3074,#3075,#3076,#3077,#3078,
#3079,#3080));
#10890=EDGE_LOOP('',(#3081,#3082,#3083,#3084,#3085,#3086,#3087,#3088,#3089,
#3090,#3091));
#10891=EDGE_LOOP('',(#3092,#3093,#3094,#3095));
#10892=EDGE_LOOP('',(#3096,#3097,#3098,#3099,#3100));
#10893=EDGE_LOOP('',(#3101,#3102,#3103,#3104));
#10894=EDGE_LOOP('',(#3105));
#10895=EDGE_LOOP('',(#3106));
#10896=EDGE_LOOP('',(#3107,#3108,#3109,#3110,#3111,#3112,#3113,#3114,#3115,
#3116,#3117,#3118,#3119,#3120,#3121,#3122,#3123,#3124,#3125,#3126,#3127,
#3128,#3129,#3130,#3131,#3132,#3133,#3134,#3135,#3136,#3137,#3138,#3139,
#3140,#3141,#3142,#3143,#3144,#3145,#3146,#3147,#3148,#3149,#3150,#3151,
#3152,#3153,#3154,#3155,#3156,#3157,#3158,#3159,#3160,#3161,#3162,#3163,
#3164,#3165,#3166,#3167,#3168,#3169,#3170,#3171,#3172,#3173,#3174,#3175,
#3176,#3177,#3178,#3179,#3180,#3181,#3182,#3183,#3184,#3185,#3186,#3187,
#3188,#3189,#3190,#3191,#3192,#3193,#3194,#3195,#3196,#3197,#3198,#3199,
#3200,#3201,#3202,#3203,#3204,#3205,#3206,#3207,#3208,#3209,#3210,#3211,
#3212,#3213,#3214,#3215,#3216,#3217,#3218,#3219,#3220,#3221,#3222,#3223,
#3224,#3225,#3226,#3227,#3228,#3229,#3230,#3231,#3232,#3233,#3234,#3235,
#3236,#3237,#3238,#3239,#3240,#3241,#3242,#3243,#3244,#3245,#3246,#3247,
#3248,#3249));
#10897=EDGE_LOOP('',(#3250));
#10898=EDGE_LOOP('',(#3251,#3252,#3253,#3254,#3255,#3256,#3257,#3258,#3259,
#3260,#3261,#3262,#3263,#3264,#3265,#3266,#3267,#3268,#3269,#3270,#3271,
#3272,#3273,#3274,#3275,#3276,#3277,#3278,#3279,#3280,#3281,#3282,#3283,
#3284,#3285,#3286,#3287,#3288,#3289,#3290,#3291,#3292,#3293,#3294,#3295,
#3296,#3297,#3298,#3299,#3300,#3301,#3302,#3303,#3304,#3305,#3306,#3307,
#3308,#3309,#3310,#3311,#3312,#3313,#3314,#3315,#3316,#3317,#3318,#3319,
#3320,#3321,#3322,#3323,#3324,#3325,#3326,#3327,#3328,#3329,#3330,#3331,
#3332,#3333,#3334,#3335,#3336,#3337,#3338,#3339,#3340,#3341,#3342,#3343,
#3344,#3345,#3346,#3347,#3348,#3349,#3350,#3351,#3352,#3353,#3354,#3355,
#3356,#3357,#3358,#3359,#3360,#3361,#3362,#3363,#3364,#3365,#3366,#3367,
#3368,#3369,#3370,#3371,#3372,#3373,#3374,#3375,#3376,#3377,#3378,#3379,
#3380,#3381,#3382,#3383,#3384,#3385,#3386,#3387,#3388,#3389,#3390,#3391,
#3392,#3393));
#10899=EDGE_LOOP('',(#3394));
#10900=EDGE_LOOP('',(#3395,#3396,#3397,#3398));
#10901=EDGE_LOOP('',(#3399,#3400,#3401,#3402));
#10902=EDGE_LOOP('',(#3403,#3404,#3405,#3406));
#10903=EDGE_LOOP('',(#3407,#3408,#3409,#3410));
#10904=EDGE_LOOP('',(#3411,#3412,#3413,#3414));
#10905=EDGE_LOOP('',(#3415,#3416,#3417,#3418));
#10906=EDGE_LOOP('',(#3419,#3420,#3421,#3422));
#10907=EDGE_LOOP('',(#3423,#3424,#3425,#3426));
#10908=EDGE_LOOP('',(#3427,#3428,#3429,#3430));
#10909=EDGE_LOOP('',(#3431,#3432,#3433,#3434));
#10910=EDGE_LOOP('',(#3435,#3436,#3437,#3438));
#10911=EDGE_LOOP('',(#3439,#3440,#3441,#3442));
#10912=EDGE_LOOP('',(#3443,#3444,#3445,#3446));
#10913=EDGE_LOOP('',(#3447,#3448,#3449,#3450));
#10914=EDGE_LOOP('',(#3451,#3452,#3453,#3454));
#10915=EDGE_LOOP('',(#3455,#3456,#3457,#3458));
#10916=EDGE_LOOP('',(#3459,#3460,#3461,#3462));
#10917=EDGE_LOOP('',(#3463,#3464,#3465,#3466));
#10918=EDGE_LOOP('',(#3467,#3468,#3469,#3470));
#10919=EDGE_LOOP('',(#3471,#3472,#3473,#3474));
#10920=EDGE_LOOP('',(#3475,#3476,#3477,#3478));
#10921=EDGE_LOOP('',(#3479,#3480,#3481,#3482));
#10922=EDGE_LOOP('',(#3483,#3484,#3485,#3486));
#10923=EDGE_LOOP('',(#3487,#3488,#3489,#3490));
#10924=EDGE_LOOP('',(#3491,#3492,#3493,#3494));
#10925=EDGE_LOOP('',(#3495,#3496,#3497,#3498));
#10926=EDGE_LOOP('',(#3499,#3500,#3501,#3502));
#10927=EDGE_LOOP('',(#3503,#3504,#3505,#3506));
#10928=EDGE_LOOP('',(#3507,#3508,#3509,#3510));
#10929=EDGE_LOOP('',(#3511,#3512,#3513,#3514));
#10930=EDGE_LOOP('',(#3515,#3516,#3517,#3518));
#10931=EDGE_LOOP('',(#3519,#3520,#3521,#3522));
#10932=EDGE_LOOP('',(#3523,#3524,#3525,#3526));
#10933=EDGE_LOOP('',(#3527,#3528,#3529,#3530));
#10934=EDGE_LOOP('',(#3531,#3532,#3533,#3534));
#10935=EDGE_LOOP('',(#3535,#3536,#3537,#3538));
#10936=EDGE_LOOP('',(#3539,#3540,#3541,#3542));
#10937=EDGE_LOOP('',(#3543,#3544,#3545,#3546));
#10938=EDGE_LOOP('',(#3547,#3548,#3549,#3550));
#10939=EDGE_LOOP('',(#3551,#3552,#3553,#3554));
#10940=EDGE_LOOP('',(#3555,#3556,#3557,#3558));
#10941=EDGE_LOOP('',(#3559,#3560,#3561,#3562));
#10942=EDGE_LOOP('',(#3563,#3564,#3565,#3566));
#10943=EDGE_LOOP('',(#3567,#3568,#3569,#3570));
#10944=EDGE_LOOP('',(#3571,#3572,#3573,#3574));
#10945=EDGE_LOOP('',(#3575,#3576,#3577,#3578));
#10946=EDGE_LOOP('',(#3579,#3580,#3581,#3582));
#10947=EDGE_LOOP('',(#3583,#3584,#3585,#3586));
#10948=EDGE_LOOP('',(#3587,#3588,#3589,#3590));
#10949=EDGE_LOOP('',(#3591,#3592,#3593,#3594));
#10950=EDGE_LOOP('',(#3595,#3596,#3597,#3598));
#10951=EDGE_LOOP('',(#3599,#3600,#3601,#3602));
#10952=EDGE_LOOP('',(#3603,#3604,#3605,#3606));
#10953=EDGE_LOOP('',(#3607,#3608,#3609,#3610));
#10954=EDGE_LOOP('',(#3611,#3612,#3613,#3614));
#10955=EDGE_LOOP('',(#3615,#3616,#3617,#3618));
#10956=EDGE_LOOP('',(#3619,#3620,#3621,#3622));
#10957=EDGE_LOOP('',(#3623,#3624,#3625,#3626));
#10958=EDGE_LOOP('',(#3627,#3628,#3629,#3630));
#10959=EDGE_LOOP('',(#3631,#3632,#3633,#3634));
#10960=EDGE_LOOP('',(#3635,#3636,#3637,#3638));
#10961=EDGE_LOOP('',(#3639,#3640,#3641,#3642));
#10962=EDGE_LOOP('',(#3643,#3644,#3645,#3646));
#10963=EDGE_LOOP('',(#3647,#3648,#3649,#3650));
#10964=EDGE_LOOP('',(#3651,#3652,#3653,#3654));
#10965=EDGE_LOOP('',(#3655,#3656,#3657,#3658));
#10966=EDGE_LOOP('',(#3659,#3660,#3661,#3662));
#10967=EDGE_LOOP('',(#3663,#3664,#3665,#3666));
#10968=EDGE_LOOP('',(#3667,#3668,#3669,#3670));
#10969=EDGE_LOOP('',(#3671,#3672,#3673,#3674));
#10970=EDGE_LOOP('',(#3675,#3676,#3677,#3678));
#10971=EDGE_LOOP('',(#3679,#3680,#3681,#3682));
#10972=EDGE_LOOP('',(#3683,#3684,#3685,#3686));
#10973=EDGE_LOOP('',(#3687,#3688,#3689,#3690));
#10974=EDGE_LOOP('',(#3691,#3692,#3693,#3694));
#10975=EDGE_LOOP('',(#3695,#3696,#3697,#3698));
#10976=EDGE_LOOP('',(#3699,#3700,#3701,#3702));
#10977=EDGE_LOOP('',(#3703,#3704,#3705,#3706));
#10978=EDGE_LOOP('',(#3707,#3708,#3709,#3710));
#10979=EDGE_LOOP('',(#3711,#3712,#3713,#3714));
#10980=EDGE_LOOP('',(#3715,#3716,#3717,#3718));
#10981=EDGE_LOOP('',(#3719,#3720,#3721,#3722));
#10982=EDGE_LOOP('',(#3723,#3724,#3725,#3726));
#10983=EDGE_LOOP('',(#3727,#3728,#3729,#3730));
#10984=EDGE_LOOP('',(#3731,#3732,#3733,#3734));
#10985=EDGE_LOOP('',(#3735,#3736,#3737,#3738));
#10986=EDGE_LOOP('',(#3739,#3740,#3741,#3742));
#10987=EDGE_LOOP('',(#3743,#3744,#3745,#3746));
#10988=EDGE_LOOP('',(#3747,#3748,#3749,#3750));
#10989=EDGE_LOOP('',(#3751,#3752,#3753,#3754));
#10990=EDGE_LOOP('',(#3755,#3756,#3757,#3758));
#10991=EDGE_LOOP('',(#3759,#3760,#3761,#3762));
#10992=EDGE_LOOP('',(#3763,#3764,#3765,#3766));
#10993=EDGE_LOOP('',(#3767,#3768,#3769,#3770));
#10994=EDGE_LOOP('',(#3771,#3772,#3773,#3774));
#10995=EDGE_LOOP('',(#3775,#3776,#3777,#3778));
#10996=EDGE_LOOP('',(#3779,#3780,#3781,#3782));
#10997=EDGE_LOOP('',(#3783,#3784,#3785,#3786));
#10998=EDGE_LOOP('',(#3787,#3788,#3789,#3790));
#10999=EDGE_LOOP('',(#3791,#3792,#3793,#3794));
#11000=EDGE_LOOP('',(#3795,#3796,#3797,#3798));
#11001=EDGE_LOOP('',(#3799,#3800,#3801,#3802));
#11002=EDGE_LOOP('',(#3803,#3804,#3805,#3806));
#11003=EDGE_LOOP('',(#3807,#3808,#3809,#3810));
#11004=EDGE_LOOP('',(#3811,#3812,#3813,#3814));
#11005=EDGE_LOOP('',(#3815,#3816,#3817,#3818));
#11006=EDGE_LOOP('',(#3819,#3820,#3821,#3822));
#11007=EDGE_LOOP('',(#3823,#3824,#3825,#3826));
#11008=EDGE_LOOP('',(#3827,#3828,#3829,#3830));
#11009=EDGE_LOOP('',(#3831,#3832,#3833,#3834));
#11010=EDGE_LOOP('',(#3835,#3836,#3837,#3838));
#11011=EDGE_LOOP('',(#3839,#3840,#3841,#3842));
#11012=EDGE_LOOP('',(#3843,#3844,#3845,#3846));
#11013=EDGE_LOOP('',(#3847,#3848,#3849,#3850));
#11014=EDGE_LOOP('',(#3851,#3852,#3853,#3854));
#11015=EDGE_LOOP('',(#3855,#3856,#3857,#3858));
#11016=EDGE_LOOP('',(#3859,#3860,#3861,#3862));
#11017=EDGE_LOOP('',(#3863,#3864,#3865,#3866));
#11018=EDGE_LOOP('',(#3867,#3868,#3869,#3870));
#11019=EDGE_LOOP('',(#3871,#3872,#3873,#3874));
#11020=EDGE_LOOP('',(#3875,#3876,#3877,#3878));
#11021=EDGE_LOOP('',(#3879,#3880,#3881,#3882));
#11022=EDGE_LOOP('',(#3883,#3884,#3885,#3886));
#11023=EDGE_LOOP('',(#3887,#3888,#3889,#3890));
#11024=EDGE_LOOP('',(#3891,#3892,#3893,#3894));
#11025=EDGE_LOOP('',(#3895,#3896,#3897,#3898));
#11026=EDGE_LOOP('',(#3899,#3900,#3901,#3902));
#11027=EDGE_LOOP('',(#3903,#3904,#3905,#3906));
#11028=EDGE_LOOP('',(#3907,#3908,#3909,#3910));
#11029=EDGE_LOOP('',(#3911,#3912,#3913,#3914));
#11030=EDGE_LOOP('',(#3915,#3916,#3917,#3918));
#11031=EDGE_LOOP('',(#3919,#3920,#3921,#3922));
#11032=EDGE_LOOP('',(#3923,#3924,#3925,#3926));
#11033=EDGE_LOOP('',(#3927,#3928,#3929,#3930));
#11034=EDGE_LOOP('',(#3931,#3932,#3933,#3934));
#11035=EDGE_LOOP('',(#3935,#3936,#3937,#3938));
#11036=EDGE_LOOP('',(#3939,#3940,#3941,#3942));
#11037=EDGE_LOOP('',(#3943,#3944,#3945,#3946));
#11038=EDGE_LOOP('',(#3947,#3948,#3949,#3950));
#11039=EDGE_LOOP('',(#3951,#3952,#3953,#3954));
#11040=EDGE_LOOP('',(#3955,#3956,#3957,#3958));
#11041=EDGE_LOOP('',(#3959,#3960,#3961,#3962));
#11042=EDGE_LOOP('',(#3963,#3964,#3965,#3966));
#11043=EDGE_LOOP('',(#3967,#3968,#3969));
#11044=EDGE_LOOP('',(#3970));
#11045=EDGE_LOOP('',(#3971,#3972,#3973,#3974,#3975,#3976,#3977,#3978,#3979,
#3980,#3981,#3982,#3983,#3984,#3985,#3986,#3987,#3988,#3989));
#11046=EDGE_LOOP('',(#3990));
#11047=EDGE_LOOP('',(#3991));
#11048=EDGE_LOOP('',(#3992));
#11049=EDGE_LOOP('',(#3993));
#11050=EDGE_LOOP('',(#3994));
#11051=EDGE_LOOP('',(#3995));
#11052=EDGE_LOOP('',(#3996));
#11053=EDGE_LOOP('',(#3997));
#11054=EDGE_LOOP('',(#3998));
#11055=EDGE_LOOP('',(#3999));
#11056=EDGE_LOOP('',(#4000));
#11057=EDGE_LOOP('',(#4001));
#11058=EDGE_LOOP('',(#4002));
#11059=EDGE_LOOP('',(#4003));
#11060=EDGE_LOOP('',(#4004));
#11061=EDGE_LOOP('',(#4005));
#11062=EDGE_LOOP('',(#4006));
#11063=EDGE_LOOP('',(#4007));
#11064=EDGE_LOOP('',(#4008));
#11065=EDGE_LOOP('',(#4009));
#11066=EDGE_LOOP('',(#4010));
#11067=EDGE_LOOP('',(#4011));
#11068=EDGE_LOOP('',(#4012));
#11069=EDGE_LOOP('',(#4013));
#11070=EDGE_LOOP('',(#4014));
#11071=EDGE_LOOP('',(#4015));
#11072=EDGE_LOOP('',(#4016,#4017,#4018,#4019));
#11073=EDGE_LOOP('',(#4020,#4021,#4022,#4023));
#11074=EDGE_LOOP('',(#4024,#4025,#4026,#4027));
#11075=EDGE_LOOP('',(#4028,#4029,#4030,#4031));
#11076=EDGE_LOOP('',(#4032,#4033,#4034,#4035));
#11077=EDGE_LOOP('',(#4036,#4037,#4038,#4039));
#11078=EDGE_LOOP('',(#4040));
#11079=EDGE_LOOP('',(#4041));
#11080=EDGE_LOOP('',(#4042,#4043,#4044,#4045));
#11081=EDGE_LOOP('',(#4046));
#11082=EDGE_LOOP('',(#4047));
#11083=EDGE_LOOP('',(#4048,#4049,#4050,#4051));
#11084=EDGE_LOOP('',(#4052));
#11085=EDGE_LOOP('',(#4053));
#11086=EDGE_LOOP('',(#4054));
#11087=EDGE_LOOP('',(#4055));
#11088=EDGE_LOOP('',(#4056,#4057,#4058,#4059));
#11089=EDGE_LOOP('',(#4060,#4061,#4062,#4063));
#11090=EDGE_LOOP('',(#4064,#4065,#4066,#4067));
#11091=EDGE_LOOP('',(#4068,#4069,#4070,#4071));
#11092=EDGE_LOOP('',(#4072,#4073,#4074,#4075));
#11093=EDGE_LOOP('',(#4076,#4077,#4078,#4079));
#11094=EDGE_LOOP('',(#4080,#4081,#4082,#4083));
#11095=EDGE_LOOP('',(#4084,#4085,#4086,#4087));
#11096=EDGE_LOOP('',(#4088,#4089,#4090,#4091));
#11097=EDGE_LOOP('',(#4092,#4093,#4094,#4095));
#11098=EDGE_LOOP('',(#4096,#4097,#4098,#4099));
#11099=EDGE_LOOP('',(#4100,#4101,#4102,#4103));
#11100=EDGE_LOOP('',(#4104,#4105,#4106,#4107));
#11101=EDGE_LOOP('',(#4108));
#11102=EDGE_LOOP('',(#4109));
#11103=EDGE_LOOP('',(#4110));
#11104=EDGE_LOOP('',(#4111));
#11105=EDGE_LOOP('',(#4112));
#11106=EDGE_LOOP('',(#4113));
#11107=EDGE_LOOP('',(#4114));
#11108=EDGE_LOOP('',(#4115));
#11109=EDGE_LOOP('',(#4116));
#11110=EDGE_LOOP('',(#4117,#4118,#4119,#4120));
#11111=EDGE_LOOP('',(#4121,#4122,#4123,#4124));
#11112=EDGE_LOOP('',(#4125,#4126,#4127,#4128));
#11113=EDGE_LOOP('',(#4129));
#11114=EDGE_LOOP('',(#4130));
#11115=EDGE_LOOP('',(#4131));
#11116=EDGE_LOOP('',(#4132));
#11117=EDGE_LOOP('',(#4133));
#11118=EDGE_LOOP('',(#4134,#4135,#4136,#4137));
#11119=EDGE_LOOP('',(#4138,#4139,#4140,#4141));
#11120=EDGE_LOOP('',(#4142,#4143,#4144,#4145));
#11121=EDGE_LOOP('',(#4146));
#11122=EDGE_LOOP('',(#4147));
#11123=EDGE_LOOP('',(#4148));
#11124=EDGE_LOOP('',(#4149));
#11125=EDGE_LOOP('',(#4150));
#11126=EDGE_LOOP('',(#4151));
#11127=EDGE_LOOP('',(#4152));
#11128=EDGE_LOOP('',(#4153));
#11129=EDGE_LOOP('',(#4154));
#11130=EDGE_LOOP('',(#4155));
#11131=EDGE_LOOP('',(#4156));
#11132=EDGE_LOOP('',(#4157));
#11133=EDGE_LOOP('',(#4158));
#11134=EDGE_LOOP('',(#4159));
#11135=EDGE_LOOP('',(#4160));
#11136=EDGE_LOOP('',(#4161));
#11137=EDGE_LOOP('',(#4162));
#11138=EDGE_LOOP('',(#4163));
#11139=EDGE_LOOP('',(#4164,#4165,#4166,#4167));
#11140=EDGE_LOOP('',(#4168,#4169,#4170,#4171));
#11141=EDGE_LOOP('',(#4172,#4173,#4174,#4175));
#11142=EDGE_LOOP('',(#4176));
#11143=EDGE_LOOP('',(#4177));
#11144=EDGE_LOOP('',(#4178));
#11145=EDGE_LOOP('',(#4179));
#11146=EDGE_LOOP('',(#4180));
#11147=EDGE_LOOP('',(#4181));
#11148=EDGE_LOOP('',(#4182));
#11149=EDGE_LOOP('',(#4183));
#11150=EDGE_LOOP('',(#4184,#4185,#4186,#4187));
#11151=EDGE_LOOP('',(#4188,#4189,#4190,#4191));
#11152=EDGE_LOOP('',(#4192,#4193,#4194,#4195));
#11153=EDGE_LOOP('',(#4196,#4197,#4198,#4199));
#11154=EDGE_LOOP('',(#4200,#4201,#4202,#4203));
#11155=EDGE_LOOP('',(#4204,#4205,#4206,#4207));
#11156=EDGE_LOOP('',(#4208,#4209,#4210,#4211));
#11157=EDGE_LOOP('',(#4212,#4213,#4214,#4215));
#11158=EDGE_LOOP('',(#4216,#4217,#4218,#4219));
#11159=EDGE_LOOP('',(#4220,#4221,#4222,#4223));
#11160=EDGE_LOOP('',(#4224,#4225,#4226,#4227));
#11161=EDGE_LOOP('',(#4228,#4229,#4230,#4231));
#11162=EDGE_LOOP('',(#4232));
#11163=EDGE_LOOP('',(#4233));
#11164=EDGE_LOOP('',(#4234,#4235,#4236,#4237));
#11165=EDGE_LOOP('',(#4238,#4239,#4240,#4241));
#11166=EDGE_LOOP('',(#4242,#4243,#4244,#4245));
#11167=EDGE_LOOP('',(#4246));
#11168=EDGE_LOOP('',(#4247));
#11169=EDGE_LOOP('',(#4248));
#11170=EDGE_LOOP('',(#4249));
#11171=EDGE_LOOP('',(#4250));
#11172=EDGE_LOOP('',(#4251));
#11173=EDGE_LOOP('',(#4252,#4253,#4254,#4255));
#11174=EDGE_LOOP('',(#4256,#4257,#4258,#4259));
#11175=EDGE_LOOP('',(#4260,#4261,#4262,#4263));
#11176=EDGE_LOOP('',(#4264,#4265,#4266,#4267));
#11177=EDGE_LOOP('',(#4268,#4269,#4270,#4271));
#11178=EDGE_LOOP('',(#4272,#4273,#4274,#4275));
#11179=EDGE_LOOP('',(#4276,#4277,#4278,#4279));
#11180=EDGE_LOOP('',(#4280,#4281,#4282,#4283));
#11181=EDGE_LOOP('',(#4284,#4285,#4286,#4287));
#11182=EDGE_LOOP('',(#4288,#4289,#4290,#4291));
#11183=EDGE_LOOP('',(#4292,#4293,#4294,#4295));
#11184=EDGE_LOOP('',(#4296,#4297,#4298,#4299));
#11185=EDGE_LOOP('',(#4300,#4301,#4302,#4303));
#11186=EDGE_LOOP('',(#4304,#4305,#4306,#4307,#4308,#4309,#4310,#4311));
#11187=EDGE_LOOP('',(#4312));
#11188=EDGE_LOOP('',(#4313,#4314,#4315,#4316));
#11189=EDGE_LOOP('',(#4317,#4318,#4319,#4320));
#11190=EDGE_LOOP('',(#4321,#4322,#4323,#4324));
#11191=EDGE_LOOP('',(#4325,#4326,#4327,#4328));
#11192=EDGE_LOOP('',(#4329,#4330,#4331,#4332));
#11193=EDGE_LOOP('',(#4333,#4334,#4335,#4336,#4337,#4338,#4339,#4340));
#11194=EDGE_LOOP('',(#4341));
#11195=EDGE_LOOP('',(#4342,#4343,#4344,#4345));
#11196=EDGE_LOOP('',(#4346,#4347,#4348,#4349));
#11197=EDGE_LOOP('',(#4350,#4351,#4352,#4353));
#11198=EDGE_LOOP('',(#4354,#4355,#4356,#4357));
#11199=EDGE_LOOP('',(#4358,#4359,#4360,#4361));
#11200=EDGE_LOOP('',(#4362));
#11201=EDGE_LOOP('',(#4363));
#11202=EDGE_LOOP('',(#4364,#4365,#4366,#4367));
#11203=EDGE_LOOP('',(#4368));
#11204=EDGE_LOOP('',(#4369,#4370,#4371,#4372,#4373,#4374,#4375,#4376));
#11205=EDGE_LOOP('',(#4377,#4378,#4379,#4380));
#11206=EDGE_LOOP('',(#4381));
#11207=EDGE_LOOP('',(#4382,#4383,#4384,#4385,#4386,#4387,#4388,#4389));
#11208=EDGE_LOOP('',(#4390));
#11209=EDGE_LOOP('',(#4391,#4392,#4393,#4394,#4395,#4396,#4397,#4398));
#11210=EDGE_LOOP('',(#4399,#4400,#4401,#4402));
#11211=EDGE_LOOP('',(#4403));
#11212=EDGE_LOOP('',(#4404,#4405,#4406,#4407,#4408,#4409,#4410,#4411));
#11213=EDGE_LOOP('',(#4412,#4413,#4414,#4415));
#11214=EDGE_LOOP('',(#4416));
#11215=EDGE_LOOP('',(#4417,#4418,#4419,#4420,#4421,#4422,#4423,#4424));
#11216=EDGE_LOOP('',(#4425));
#11217=EDGE_LOOP('',(#4426,#4427,#4428,#4429,#4430,#4431,#4432,#4433));
#11218=EDGE_LOOP('',(#4434));
#11219=EDGE_LOOP('',(#4435,#4436,#4437,#4438,#4439,#4440,#4441,#4442));
#11220=EDGE_LOOP('',(#4443,#4444,#4445,#4446));
#11221=EDGE_LOOP('',(#4447));
#11222=EDGE_LOOP('',(#4448,#4449,#4450,#4451,#4452,#4453,#4454,#4455));
#11223=EDGE_LOOP('',(#4456,#4457,#4458,#4459));
#11224=EDGE_LOOP('',(#4460,#4461,#4462,#4463));
#11225=EDGE_LOOP('',(#4464,#4465,#4466,#4467));
#11226=EDGE_LOOP('',(#4468,#4469,#4470,#4471));
#11227=EDGE_LOOP('',(#4472,#4473,#4474,#4475));
#11228=EDGE_LOOP('',(#4476,#4477,#4478,#4479));
#11229=EDGE_LOOP('',(#4480,#4481,#4482,#4483));
#11230=EDGE_LOOP('',(#4484,#4485,#4486,#4487));
#11231=EDGE_LOOP('',(#4488,#4489,#4490,#4491));
#11232=EDGE_LOOP('',(#4492,#4493,#4494,#4495));
#11233=EDGE_LOOP('',(#4496,#4497,#4498,#4499));
#11234=EDGE_LOOP('',(#4500,#4501,#4502,#4503));
#11235=EDGE_LOOP('',(#4504,#4505,#4506,#4507));
#11236=EDGE_LOOP('',(#4508,#4509,#4510,#4511));
#11237=EDGE_LOOP('',(#4512,#4513,#4514,#4515));
#11238=EDGE_LOOP('',(#4516,#4517,#4518,#4519));
#11239=EDGE_LOOP('',(#4520,#4521,#4522,#4523));
#11240=EDGE_LOOP('',(#4524,#4525,#4526,#4527));
#11241=EDGE_LOOP('',(#4528,#4529,#4530,#4531));
#11242=EDGE_LOOP('',(#4532,#4533,#4534,#4535));
#11243=EDGE_LOOP('',(#4536,#4537,#4538,#4539));
#11244=EDGE_LOOP('',(#4540));
#11245=EDGE_LOOP('',(#4541,#4542,#4543,#4544,#4545,#4546,#4547,#4548,#4549,
#4550,#4551));
#11246=EDGE_LOOP('',(#4552,#4553,#4554,#4555,#4556,#4557,#4558,#4559,#4560,
#4561,#4562));
#11247=EDGE_LOOP('',(#4563,#4564,#4565,#4566));
#11248=EDGE_LOOP('',(#4567,#4568,#4569,#4570));
#11249=EDGE_LOOP('',(#4571,#4572,#4573,#4574));
#11250=EDGE_LOOP('',(#4575));
#11251=EDGE_LOOP('',(#4576));
#11252=EDGE_LOOP('',(#4577,#4578,#4579,#4580,#4581,#4582,#4583,#4584,#4585,
#4586,#4587,#4588));
#11253=EDGE_LOOP('',(#4589,#4590,#4591,#4592,#4593,#4594));
#11254=EDGE_LOOP('',(#4595,#4596,#4597,#4598,#4599,#4600,#4601));
#11255=EDGE_LOOP('',(#4602,#4603,#4604,#4605,#4606,#4607,#4608,#4609,#4610,
#4611,#4612));
#11256=EDGE_LOOP('',(#4613,#4614,#4615));
#11257=EDGE_LOOP('',(#4616,#4617,#4618,#4619,#4620));
#11258=EDGE_LOOP('',(#4621,#4622));
#11259=EDGE_LOOP('',(#4623,#4624));
#11260=EDGE_LOOP('',(#4625));
#11261=EDGE_LOOP('',(#4626));
#11262=EDGE_LOOP('',(#4627));
#11263=EDGE_LOOP('',(#4628,#4629));
#11264=EDGE_LOOP('',(#4630));
#11265=EDGE_LOOP('',(#4631,#4632));
#11266=EDGE_LOOP('',(#4633));
#11267=EDGE_LOOP('',(#4634));
#11268=EDGE_LOOP('',(#4635,#4636));
#11269=EDGE_LOOP('',(#4637,#4638,#4639,#4640,#4641,#4642,#4643,#4644,#4645,
#4646,#4647,#4648,#4649,#4650,#4651,#4652,#4653,#4654,#4655));
#11270=EDGE_LOOP('',(#4656,#4657));
#11271=EDGE_LOOP('',(#4658,#4659,#4660,#4661,#4662,#4663,#4664,#4665,#4666,
#4667,#4668,#4669,#4670,#4671,#4672,#4673,#4674));
#11272=EDGE_LOOP('',(#4675));
#11273=EDGE_LOOP('',(#4676));
#11274=EDGE_LOOP('',(#4677));
#11275=EDGE_LOOP('',(#4678));
#11276=EDGE_LOOP('',(#4679));
#11277=EDGE_LOOP('',(#4680));
#11278=EDGE_LOOP('',(#4681));
#11279=EDGE_LOOP('',(#4682));
#11280=EDGE_LOOP('',(#4683));
#11281=EDGE_LOOP('',(#4684,#4685,#4686,#4687,#4688,#4689,#4690,#4691,#4692,
#4693,#4694,#4695));
#11282=EDGE_LOOP('',(#4696));
#11283=EDGE_LOOP('',(#4697,#4698,#4699));
#11284=EDGE_LOOP('',(#4700));
#11285=EDGE_LOOP('',(#4701));
#11286=EDGE_LOOP('',(#4702));
#11287=EDGE_LOOP('',(#4703));
#11288=EDGE_LOOP('',(#4704));
#11289=EDGE_LOOP('',(#4705));
#11290=EDGE_LOOP('',(#4706,#4707));
#11291=EDGE_LOOP('',(#4708));
#11292=EDGE_LOOP('',(#4709));
#11293=EDGE_LOOP('',(#4710));
#11294=EDGE_LOOP('',(#4711));
#11295=EDGE_LOOP('',(#4712));
#11296=EDGE_LOOP('',(#4713));
#11297=EDGE_LOOP('',(#4714));
#11298=EDGE_LOOP('',(#4715));
#11299=EDGE_LOOP('',(#4716,#4717));
#11300=EDGE_LOOP('',(#4718));
#11301=EDGE_LOOP('',(#4719));
#11302=EDGE_LOOP('',(#4720));
#11303=EDGE_LOOP('',(#4721));
#11304=EDGE_LOOP('',(#4722));
#11305=EDGE_LOOP('',(#4723));
#11306=EDGE_LOOP('',(#4724));
#11307=EDGE_LOOP('',(#4725));
#11308=EDGE_LOOP('',(#4726));
#11309=EDGE_LOOP('',(#4727));
#11310=EDGE_LOOP('',(#4728));
#11311=EDGE_LOOP('',(#4729));
#11312=EDGE_LOOP('',(#4730,#4731,#4732,#4733));
#11313=EDGE_LOOP('',(#4734,#4735,#4736,#4737));
#11314=EDGE_LOOP('',(#4738,#4739,#4740,#4741));
#11315=EDGE_LOOP('',(#4742));
#11316=EDGE_LOOP('',(#4743));
#11317=EDGE_LOOP('',(#4744,#4745,#4746,#4747));
#11318=EDGE_LOOP('',(#4748,#4749,#4750,#4751));
#11319=EDGE_LOOP('',(#4752,#4753,#4754,#4755));
#11320=EDGE_LOOP('',(#4756,#4757,#4758,#4759));
#11321=EDGE_LOOP('',(#4760,#4761,#4762,#4763));
#11322=EDGE_LOOP('',(#4764,#4765,#4766,#4767));
#11323=EDGE_LOOP('',(#4768,#4769,#4770,#4771));
#11324=EDGE_LOOP('',(#4772,#4773,#4774,#4775));
#11325=EDGE_LOOP('',(#4776,#4777,#4778,#4779));
#11326=EDGE_LOOP('',(#4780,#4781,#4782,#4783));
#11327=EDGE_LOOP('',(#4784,#4785,#4786,#4787));
#11328=EDGE_LOOP('',(#4788,#4789,#4790,#4791));
#11329=EDGE_LOOP('',(#4792,#4793,#4794,#4795));
#11330=EDGE_LOOP('',(#4796,#4797,#4798,#4799));
#11331=EDGE_LOOP('',(#4800,#4801,#4802,#4803));
#11332=EDGE_LOOP('',(#4804));
#11333=EDGE_LOOP('',(#4805));
#11334=EDGE_LOOP('',(#4806));
#11335=EDGE_LOOP('',(#4807));
#11336=EDGE_LOOP('',(#4808));
#11337=EDGE_LOOP('',(#4809,#4810,#4811,#4812));
#11338=EDGE_LOOP('',(#4813,#4814,#4815,#4816));
#11339=EDGE_LOOP('',(#4817,#4818,#4819,#4820));
#11340=EDGE_LOOP('',(#4821));
#11341=EDGE_LOOP('',(#4822));
#11342=EDGE_LOOP('',(#4823));
#11343=EDGE_LOOP('',(#4824));
#11344=EDGE_LOOP('',(#4825));
#11345=EDGE_LOOP('',(#4826));
#11346=EDGE_LOOP('',(#4827));
#11347=EDGE_LOOP('',(#4828));
#11348=EDGE_LOOP('',(#4829));
#11349=EDGE_LOOP('',(#4830));
#11350=EDGE_LOOP('',(#4831));
#11351=EDGE_LOOP('',(#4832));
#11352=EDGE_LOOP('',(#4833));
#11353=EDGE_LOOP('',(#4834));
#11354=EDGE_LOOP('',(#4835));
#11355=EDGE_LOOP('',(#4836));
#11356=EDGE_LOOP('',(#4837));
#11357=EDGE_LOOP('',(#4838,#4839,#4840,#4841));
#11358=EDGE_LOOP('',(#4842,#4843,#4844,#4845));
#11359=EDGE_LOOP('',(#4846,#4847,#4848,#4849));
#11360=EDGE_LOOP('',(#4850));
#11361=EDGE_LOOP('',(#4851));
#11362=EDGE_LOOP('',(#4852,#4853,#4854,#4855,#4856,#4857,#4858,#4859,#4860,
#4861,#4862,#4863));
#11363=EDGE_LOOP('',(#4864,#4865,#4866,#4867,#4868,#4869,#4870,#4871,#4872,
#4873,#4874,#4875));
#11364=EDGE_LOOP('',(#4876,#4877,#4878,#4879));
#11365=EDGE_LOOP('',(#4880,#4881,#4882,#4883));
#11366=EDGE_LOOP('',(#4884,#4885,#4886,#4887));
#11367=EDGE_LOOP('',(#4888,#4889,#4890,#4891));
#11368=EDGE_LOOP('',(#4892,#4893,#4894,#4895));
#11369=EDGE_LOOP('',(#4896,#4897,#4898,#4899));
#11370=EDGE_LOOP('',(#4900,#4901,#4902,#4903));
#11371=EDGE_LOOP('',(#4904,#4905,#4906,#4907));
#11372=EDGE_LOOP('',(#4908,#4909,#4910,#4911));
#11373=EDGE_LOOP('',(#4912,#4913,#4914,#4915));
#11374=EDGE_LOOP('',(#4916,#4917,#4918,#4919));
#11375=EDGE_LOOP('',(#4920,#4921,#4922,#4923));
#11376=EDGE_LOOP('',(#4924,#4925,#4926,#4927));
#11377=EDGE_LOOP('',(#4928,#4929,#4930,#4931));
#11378=EDGE_LOOP('',(#4932,#4933,#4934,#4935));
#11379=EDGE_LOOP('',(#4936,#4937,#4938,#4939));
#11380=EDGE_LOOP('',(#4940,#4941,#4942,#4943));
#11381=EDGE_LOOP('',(#4944,#4945,#4946,#4947));
#11382=EDGE_LOOP('',(#4948,#4949,#4950,#4951));
#11383=EDGE_LOOP('',(#4952,#4953,#4954,#4955));
#11384=EDGE_LOOP('',(#4956,#4957,#4958,#4959));
#11385=EDGE_LOOP('',(#4960,#4961,#4962,#4963));
#11386=EDGE_LOOP('',(#4964,#4965,#4966,#4967));
#11387=EDGE_LOOP('',(#4968,#4969,#4970,#4971));
#11388=EDGE_LOOP('',(#4972,#4973,#4974,#4975));
#11389=EDGE_LOOP('',(#4976,#4977,#4978,#4979));
#11390=EDGE_LOOP('',(#4980,#4981,#4982,#4983));
#11391=EDGE_LOOP('',(#4984,#4985,#4986,#4987));
#11392=EDGE_LOOP('',(#4988,#4989,#4990,#4991));
#11393=EDGE_LOOP('',(#4992,#4993,#4994,#4995));
#11394=EDGE_LOOP('',(#4996,#4997,#4998,#4999));
#11395=EDGE_LOOP('',(#5000,#5001,#5002,#5003));
#11396=EDGE_LOOP('',(#5004,#5005,#5006,#5007));
#11397=EDGE_LOOP('',(#5008,#5009,#5010,#5011));
#11398=EDGE_LOOP('',(#5012,#5013,#5014,#5015));
#11399=EDGE_LOOP('',(#5016,#5017,#5018,#5019));
#11400=EDGE_LOOP('',(#5020,#5021,#5022,#5023,#5024,#5025,#5026,#5027,#5028,
#5029,#5030,#5031,#5032,#5033,#5034,#5035,#5036,#5037,#5038,#5039,#5040,
#5041,#5042,#5043,#5044,#5045,#5046,#5047,#5048,#5049,#5050,#5051,#5052,
#5053,#5054,#5055,#5056,#5057,#5058,#5059,#5060,#5061,#5062,#5063));
#11401=EDGE_LOOP('',(#5064));
#11402=EDGE_LOOP('',(#5065,#5066,#5067,#5068,#5069,#5070,#5071,#5072,#5073,
#5074,#5075,#5076,#5077,#5078,#5079,#5080,#5081,#5082,#5083,#5084,#5085,
#5086,#5087,#5088,#5089,#5090,#5091,#5092,#5093,#5094,#5095,#5096,#5097,
#5098,#5099,#5100,#5101,#5102,#5103,#5104,#5105,#5106,#5107,#5108));
#11403=EDGE_LOOP('',(#5109));
#11404=EDGE_LOOP('',(#5110,#5111,#5112,#5113));
#11405=EDGE_LOOP('',(#5114));
#11406=EDGE_LOOP('',(#5115));
#11407=EDGE_LOOP('',(#5116,#5117,#5118,#5119));
#11408=EDGE_LOOP('',(#5120,#5121,#5122,#5123));
#11409=EDGE_LOOP('',(#5124,#5125,#5126,#5127));
#11410=EDGE_LOOP('',(#5128,#5129,#5130,#5131));
#11411=EDGE_LOOP('',(#5132,#5133,#5134,#5135));
#11412=EDGE_LOOP('',(#5136,#5137,#5138,#5139));
#11413=EDGE_LOOP('',(#5140,#5141,#5142,#5143));
#11414=EDGE_LOOP('',(#5144,#5145,#5146,#5147));
#11415=EDGE_LOOP('',(#5148,#5149,#5150,#5151));
#11416=EDGE_LOOP('',(#5152,#5153,#5154,#5155));
#11417=EDGE_LOOP('',(#5156,#5157,#5158,#5159,#5160,#5161,#5162,#5163,#5164,
#5165,#5166,#5167,#5168,#5169,#5170,#5171,#5172,#5173,#5174,#5175,#5176));
#11418=EDGE_LOOP('',(#5177));
#11419=EDGE_LOOP('',(#5178));
#11420=EDGE_LOOP('',(#5179));
#11421=EDGE_LOOP('',(#5180,#5181,#5182,#5183));
#11422=EDGE_LOOP('',(#5184,#5185,#5186,#5187));
#11423=EDGE_LOOP('',(#5188,#5189,#5190,#5191));
#11424=EDGE_LOOP('',(#5192,#5193,#5194,#5195));
#11425=EDGE_LOOP('',(#5196,#5197,#5198,#5199));
#11426=EDGE_LOOP('',(#5200,#5201,#5202,#5203));
#11427=EDGE_LOOP('',(#5204,#5205,#5206,#5207,#5208,#5209));
#11428=EDGE_LOOP('',(#5210,#5211,#5212,#5213,#5214,#5215,#5216,#5217,#5218,
#5219,#5220));
#11429=EDGE_LOOP('',(#5221,#5222,#5223,#5224,#5225,#5226,#5227,#5228,#5229,
#5230,#5231));
#11430=EDGE_LOOP('',(#5232,#5233,#5234,#5235));
#11431=EDGE_LOOP('',(#5236,#5237,#5238,#5239));
#11432=EDGE_LOOP('',(#5240,#5241,#5242,#5243));
#11433=EDGE_LOOP('',(#5244,#5245,#5246,#5247));
#11434=EDGE_LOOP('',(#5248));
#11435=EDGE_LOOP('',(#5249));
#11436=EDGE_LOOP('',(#5250,#5251,#5252,#5253,#5254,#5255,#5256,#5257));
#11437=EDGE_LOOP('',(#5258));
#11438=EDGE_LOOP('',(#5259));
#11439=EDGE_LOOP('',(#5260,#5261,#5262,#5263));
#11440=EDGE_LOOP('',(#5264,#5265,#5266,#5267));
#11441=EDGE_LOOP('',(#5268,#5269,#5270,#5271));
#11442=EDGE_LOOP('',(#5272,#5273,#5274,#5275));
#11443=EDGE_LOOP('',(#5276,#5277,#5278,#5279));
#11444=EDGE_LOOP('',(#5280,#5281));
#11445=EDGE_LOOP('',(#5282));
#11446=EDGE_LOOP('',(#5283,#5284));
#11447=EDGE_LOOP('',(#5285,#5286,#5287,#5288));
#11448=EDGE_LOOP('',(#5289,#5290,#5291,#5292,#5293,#5294,#5295,#5296,#5297,
#5298,#5299,#5300,#5301,#5302,#5303,#5304,#5305,#5306,#5307));
#11449=EDGE_LOOP('',(#5308));
#11450=EDGE_LOOP('',(#5309,#5310,#5311,#5312));
#11451=EDGE_LOOP('',(#5313));
#11452=EDGE_LOOP('',(#5314));
#11453=EDGE_LOOP('',(#5315));
#11454=EDGE_LOOP('',(#5316));
#11455=EDGE_LOOP('',(#5317,#5318));
#11456=EDGE_LOOP('',(#5319));
#11457=EDGE_LOOP('',(#5320,#5321,#5322,#5323));
#11458=EDGE_LOOP('',(#5324,#5325,#5326,#5327));
#11459=EDGE_LOOP('',(#5328,#5329,#5330,#5331));
#11460=EDGE_LOOP('',(#5332,#5333,#5334,#5335));
#11461=EDGE_LOOP('',(#5336,#5337,#5338,#5339));
#11462=EDGE_LOOP('',(#5340,#5341,#5342,#5343,#5344));
#11463=EDGE_LOOP('',(#5345,#5346,#5347,#5348));
#11464=EDGE_LOOP('',(#5349,#5350,#5351,#5352,#5353));
#11465=EDGE_LOOP('',(#5354,#5355,#5356,#5357));
#11466=EDGE_LOOP('',(#5358,#5359,#5360,#5361,#5362));
#11467=EDGE_LOOP('',(#5363,#5364,#5365,#5366));
#11468=EDGE_LOOP('',(#5367,#5368,#5369,#5370,#5371));
#11469=EDGE_LOOP('',(#5372,#5373,#5374,#5375));
#11470=EDGE_LOOP('',(#5376,#5377,#5378,#5379,#5380));
#11471=EDGE_LOOP('',(#5381,#5382,#5383,#5384));
#11472=EDGE_LOOP('',(#5385,#5386,#5387,#5388,#5389));
#11473=EDGE_LOOP('',(#5390,#5391,#5392,#5393));
#11474=EDGE_LOOP('',(#5394,#5395,#5396,#5397,#5398));
#11475=EDGE_LOOP('',(#5399,#5400,#5401,#5402));
#11476=EDGE_LOOP('',(#5403,#5404,#5405,#5406,#5407));
#11477=EDGE_LOOP('',(#5408,#5409,#5410,#5411));
#11478=EDGE_LOOP('',(#5412));
#11479=EDGE_LOOP('',(#5413,#5414,#5415,#5416,#5417,#5418,#5419,#5420));
#11480=EDGE_LOOP('',(#5421));
#11481=EDGE_LOOP('',(#5422,#5423,#5424,#5425,#5426,#5427,#5428,#5429,#5430,
#5431,#5432,#5433,#5434,#5435,#5436,#5437));
#11482=EDGE_LOOP('',(#5438));
#11483=EDGE_LOOP('',(#5439,#5440,#5441,#5442,#5443,#5444,#5445,#5446));
#11484=EDGE_LOOP('',(#5447,#5448,#5449,#5450,#5451,#5452,#5453,#5454));
#11485=EDGE_LOOP('',(#5455));
#11486=EDGE_LOOP('',(#5456,#5457,#5458,#5459));
#11487=EDGE_LOOP('',(#5460,#5461,#5462,#5463));
#11488=EDGE_LOOP('',(#5464,#5465,#5466,#5467));
#11489=EDGE_LOOP('',(#5468,#5469,#5470,#5471));
#11490=EDGE_LOOP('',(#5472,#5473,#5474,#5475));
#11491=EDGE_LOOP('',(#5476,#5477,#5478,#5479));
#11492=EDGE_LOOP('',(#5480));
#11493=EDGE_LOOP('',(#5481));
#11494=EDGE_LOOP('',(#5482,#5483,#5484,#5485));
#11495=EDGE_LOOP('',(#5486));
#11496=EDGE_LOOP('',(#5487));
#11497=EDGE_LOOP('',(#5488));
#11498=EDGE_LOOP('',(#5489));
#11499=EDGE_LOOP('',(#5490,#5491,#5492,#5493));
#11500=EDGE_LOOP('',(#5494,#5495,#5496,#5497));
#11501=EDGE_LOOP('',(#5498,#5499,#5500));
#11502=EDGE_LOOP('',(#5501,#5502,#5503,#5504,#5505));
#11503=EDGE_LOOP('',(#5506,#5507,#5508));
#11504=EDGE_LOOP('',(#5509,#5510,#5511,#5512));
#11505=EDGE_LOOP('',(#5513,#5514,#5515,#5516));
#11506=EDGE_LOOP('',(#5517,#5518,#5519));
#11507=EDGE_LOOP('',(#5520,#5521,#5522,#5523,#5524));
#11508=EDGE_LOOP('',(#5525,#5526,#5527));
#11509=EDGE_LOOP('',(#5528,#5529,#5530,#5531));
#11510=EDGE_LOOP('',(#5532,#5533,#5534,#5535,#5536,#5537,#5538,#5539,#5540,
#5541,#5542,#5543));
#11511=EDGE_LOOP('',(#5544,#5545,#5546,#5547,#5548,#5549));
#11512=EDGE_LOOP('',(#5550,#5551,#5552,#5553,#5554,#5555));
#11513=EDGE_LOOP('',(#5556,#5557,#5558,#5559,#5560,#5561,#5562,#5563,#5564,
#5565,#5566,#5567));
#11514=EDGE_LOOP('',(#5568));
#11515=EDGE_LOOP('',(#5569));
#11516=EDGE_LOOP('',(#5570));
#11517=EDGE_LOOP('',(#5571));
#11518=EDGE_LOOP('',(#5572));
#11519=EDGE_LOOP('',(#5573));
#11520=EDGE_LOOP('',(#5574,#5575,#5576));
#11521=EDGE_LOOP('',(#5577,#5578,#5579));
#11522=EDGE_LOOP('',(#5580,#5581,#5582));
#11523=EDGE_LOOP('',(#5583,#5584,#5585));
#11524=EDGE_LOOP('',(#5586,#5587,#5588,#5589,#5590,#5591,#5592,#5593,#5594,
#5595,#5596,#5597,#5598,#5599,#5600,#5601));
#11525=EDGE_LOOP('',(#5602));
#11526=EDGE_LOOP('',(#5603));
#11527=EDGE_LOOP('',(#5604));
#11528=EDGE_LOOP('',(#5605));
#11529=EDGE_LOOP('',(#5606));
#11530=EDGE_LOOP('',(#5607));
#11531=EDGE_LOOP('',(#5608,#5609,#5610,#5611,#5612,#5613,#5614,#5615,#5616,
#5617));
#11532=EDGE_LOOP('',(#5618));
#11533=EDGE_LOOP('',(#5619));
#11534=EDGE_LOOP('',(#5620));
#11535=EDGE_LOOP('',(#5621));
#11536=EDGE_LOOP('',(#5622));
#11537=EDGE_LOOP('',(#5623));
#11538=EDGE_LOOP('',(#5624));
#11539=EDGE_LOOP('',(#5625));
#11540=EDGE_LOOP('',(#5626));
#11541=EDGE_LOOP('',(#5627));
#11542=EDGE_LOOP('',(#5628));
#11543=EDGE_LOOP('',(#5629));
#11544=FACE_BOUND('',#10429,.T.);
#11545=FACE_BOUND('',#10430,.T.);
#11546=FACE_BOUND('',#10431,.T.);
#11547=FACE_BOUND('',#10432,.T.);
#11548=FACE_BOUND('',#10433,.T.);
#11549=FACE_BOUND('',#10434,.T.);
#11550=FACE_BOUND('',#10435,.T.);
#11551=FACE_BOUND('',#10436,.T.);
#11552=FACE_BOUND('',#10437,.T.);
#11553=FACE_BOUND('',#10438,.T.);
#11554=FACE_BOUND('',#10439,.T.);
#11555=FACE_BOUND('',#10440,.T.);
#11556=FACE_BOUND('',#10441,.T.);
#11557=FACE_BOUND('',#10442,.T.);
#11558=FACE_BOUND('',#10443,.T.);
#11559=FACE_BOUND('',#10444,.T.);
#11560=FACE_BOUND('',#10445,.T.);
#11561=FACE_BOUND('',#10446,.T.);
#11562=FACE_BOUND('',#10447,.T.);
#11563=FACE_BOUND('',#10448,.T.);
#11564=FACE_BOUND('',#10449,.T.);
#11565=FACE_BOUND('',#10450,.T.);
#11566=FACE_BOUND('',#10451,.T.);
#11567=FACE_BOUND('',#10452,.T.);
#11568=FACE_BOUND('',#10453,.T.);
#11569=FACE_BOUND('',#10454,.T.);
#11570=FACE_BOUND('',#10455,.T.);
#11571=FACE_BOUND('',#10456,.T.);
#11572=FACE_BOUND('',#10457,.T.);
#11573=FACE_BOUND('',#10458,.T.);
#11574=FACE_BOUND('',#10459,.T.);
#11575=FACE_BOUND('',#10460,.T.);
#11576=FACE_BOUND('',#10461,.T.);
#11577=FACE_BOUND('',#10462,.T.);
#11578=FACE_BOUND('',#10463,.T.);
#11579=FACE_BOUND('',#10464,.T.);
#11580=FACE_BOUND('',#10465,.T.);
#11581=FACE_BOUND('',#10466,.T.);
#11582=FACE_BOUND('',#10467,.T.);
#11583=FACE_BOUND('',#10468,.T.);
#11584=FACE_BOUND('',#10469,.T.);
#11585=FACE_BOUND('',#10470,.T.);
#11586=FACE_BOUND('',#10471,.T.);
#11587=FACE_BOUND('',#10472,.T.);
#11588=FACE_BOUND('',#10473,.T.);
#11589=FACE_BOUND('',#10474,.T.);
#11590=FACE_BOUND('',#10475,.T.);
#11591=FACE_BOUND('',#10476,.T.);
#11592=FACE_BOUND('',#10477,.T.);
#11593=FACE_BOUND('',#10478,.T.);
#11594=FACE_BOUND('',#10479,.T.);
#11595=FACE_BOUND('',#10480,.T.);
#11596=FACE_BOUND('',#10481,.T.);
#11597=FACE_BOUND('',#10482,.T.);
#11598=FACE_BOUND('',#10483,.T.);
#11599=FACE_BOUND('',#10484,.T.);
#11600=FACE_BOUND('',#10485,.T.);
#11601=FACE_BOUND('',#10486,.T.);
#11602=FACE_BOUND('',#10487,.T.);
#11603=FACE_BOUND('',#10488,.T.);
#11604=FACE_BOUND('',#10489,.T.);
#11605=FACE_BOUND('',#10490,.T.);
#11606=FACE_BOUND('',#10491,.T.);
#11607=FACE_BOUND('',#10492,.T.);
#11608=FACE_BOUND('',#10493,.T.);
#11609=FACE_BOUND('',#10494,.T.);
#11610=FACE_BOUND('',#10495,.T.);
#11611=FACE_BOUND('',#10496,.T.);
#11612=FACE_BOUND('',#10497,.T.);
#11613=FACE_BOUND('',#10498,.T.);
#11614=FACE_BOUND('',#10499,.T.);
#11615=FACE_BOUND('',#10500,.T.);
#11616=FACE_BOUND('',#10501,.T.);
#11617=FACE_BOUND('',#10502,.T.);
#11618=FACE_BOUND('',#10503,.T.);
#11619=FACE_BOUND('',#10504,.T.);
#11620=FACE_BOUND('',#10505,.T.);
#11621=FACE_BOUND('',#10506,.T.);
#11622=FACE_BOUND('',#10507,.T.);
#11623=FACE_BOUND('',#10508,.T.);
#11624=FACE_BOUND('',#10509,.T.);
#11625=FACE_BOUND('',#10510,.T.);
#11626=FACE_BOUND('',#10511,.T.);
#11627=FACE_BOUND('',#10512,.T.);
#11628=FACE_BOUND('',#10513,.T.);
#11629=FACE_BOUND('',#10514,.T.);
#11630=FACE_BOUND('',#10515,.T.);
#11631=FACE_BOUND('',#10516,.T.);
#11632=FACE_BOUND('',#10517,.T.);
#11633=FACE_BOUND('',#10518,.T.);
#11634=FACE_BOUND('',#10519,.T.);
#11635=FACE_BOUND('',#10520,.T.);
#11636=FACE_BOUND('',#10521,.T.);
#11637=FACE_BOUND('',#10522,.T.);
#11638=FACE_BOUND('',#10523,.T.);
#11639=FACE_BOUND('',#10524,.T.);
#11640=FACE_BOUND('',#10525,.T.);
#11641=FACE_BOUND('',#10526,.T.);
#11642=FACE_BOUND('',#10527,.T.);
#11643=FACE_BOUND('',#10528,.T.);
#11644=FACE_BOUND('',#10529,.T.);
#11645=FACE_BOUND('',#10530,.T.);
#11646=FACE_BOUND('',#10531,.T.);
#11647=FACE_BOUND('',#10532,.T.);
#11648=FACE_BOUND('',#10533,.T.);
#11649=FACE_BOUND('',#10534,.T.);
#11650=FACE_BOUND('',#10535,.T.);
#11651=FACE_BOUND('',#10536,.T.);
#11652=FACE_BOUND('',#10537,.T.);
#11653=FACE_BOUND('',#10538,.T.);
#11654=FACE_BOUND('',#10539,.T.);
#11655=FACE_BOUND('',#10540,.T.);
#11656=FACE_BOUND('',#10541,.T.);
#11657=FACE_BOUND('',#10542,.T.);
#11658=FACE_BOUND('',#10543,.T.);
#11659=FACE_BOUND('',#10544,.T.);
#11660=FACE_BOUND('',#10545,.T.);
#11661=FACE_BOUND('',#10546,.T.);
#11662=FACE_BOUND('',#10547,.T.);
#11663=FACE_BOUND('',#10548,.T.);
#11664=FACE_BOUND('',#10549,.T.);
#11665=FACE_BOUND('',#10550,.T.);
#11666=FACE_BOUND('',#10551,.T.);
#11667=FACE_BOUND('',#10552,.T.);
#11668=FACE_BOUND('',#10553,.T.);
#11669=FACE_BOUND('',#10554,.T.);
#11670=FACE_BOUND('',#10555,.T.);
#11671=FACE_BOUND('',#10556,.T.);
#11672=FACE_BOUND('',#10557,.T.);
#11673=FACE_BOUND('',#10558,.T.);
#11674=FACE_BOUND('',#10559,.T.);
#11675=FACE_BOUND('',#10560,.T.);
#11676=FACE_BOUND('',#10561,.T.);
#11677=FACE_BOUND('',#10562,.T.);
#11678=FACE_BOUND('',#10563,.T.);
#11679=FACE_BOUND('',#10564,.T.);
#11680=FACE_BOUND('',#10565,.T.);
#11681=FACE_BOUND('',#10566,.T.);
#11682=FACE_BOUND('',#10567,.T.);
#11683=FACE_BOUND('',#10568,.T.);
#11684=FACE_BOUND('',#10569,.T.);
#11685=FACE_BOUND('',#10570,.T.);
#11686=FACE_BOUND('',#10571,.T.);
#11687=FACE_BOUND('',#10572,.T.);
#11688=FACE_BOUND('',#10573,.T.);
#11689=FACE_BOUND('',#10574,.T.);
#11690=FACE_BOUND('',#10575,.T.);
#11691=FACE_BOUND('',#10576,.T.);
#11692=FACE_BOUND('',#10577,.T.);
#11693=FACE_BOUND('',#10578,.T.);
#11694=FACE_BOUND('',#10579,.T.);
#11695=FACE_BOUND('',#10580,.T.);
#11696=FACE_BOUND('',#10581,.T.);
#11697=FACE_BOUND('',#10582,.T.);
#11698=FACE_BOUND('',#10583,.T.);
#11699=FACE_BOUND('',#10584,.T.);
#11700=FACE_BOUND('',#10585,.T.);
#11701=FACE_BOUND('',#10586,.T.);
#11702=FACE_BOUND('',#10587,.T.);
#11703=FACE_BOUND('',#10588,.T.);
#11704=FACE_BOUND('',#10589,.T.);
#11705=FACE_BOUND('',#10590,.T.);
#11706=FACE_BOUND('',#10591,.T.);
#11707=FACE_BOUND('',#10592,.T.);
#11708=FACE_BOUND('',#10593,.T.);
#11709=FACE_BOUND('',#10594,.T.);
#11710=FACE_BOUND('',#10595,.T.);
#11711=FACE_BOUND('',#10596,.T.);
#11712=FACE_BOUND('',#10597,.T.);
#11713=FACE_BOUND('',#10598,.T.);
#11714=FACE_BOUND('',#10599,.T.);
#11715=FACE_BOUND('',#10600,.T.);
#11716=FACE_BOUND('',#10601,.T.);
#11717=FACE_BOUND('',#10602,.T.);
#11718=FACE_BOUND('',#10603,.T.);
#11719=FACE_BOUND('',#10604,.T.);
#11720=FACE_BOUND('',#10605,.T.);
#11721=FACE_BOUND('',#10606,.T.);
#11722=FACE_BOUND('',#10607,.T.);
#11723=FACE_BOUND('',#10608,.T.);
#11724=FACE_BOUND('',#10609,.T.);
#11725=FACE_BOUND('',#10610,.T.);
#11726=FACE_BOUND('',#10611,.T.);
#11727=FACE_BOUND('',#10612,.T.);
#11728=FACE_BOUND('',#10613,.T.);
#11729=FACE_BOUND('',#10614,.T.);
#11730=FACE_BOUND('',#10615,.T.);
#11731=FACE_BOUND('',#10616,.T.);
#11732=FACE_BOUND('',#10617,.T.);
#11733=FACE_BOUND('',#10618,.T.);
#11734=FACE_BOUND('',#10619,.T.);
#11735=FACE_BOUND('',#10620,.T.);
#11736=FACE_BOUND('',#10621,.T.);
#11737=FACE_BOUND('',#10622,.T.);
#11738=FACE_BOUND('',#10623,.T.);
#11739=FACE_BOUND('',#10624,.T.);
#11740=FACE_BOUND('',#10625,.T.);
#11741=FACE_BOUND('',#10626,.T.);
#11742=FACE_BOUND('',#10627,.T.);
#11743=FACE_BOUND('',#10628,.T.);
#11744=FACE_BOUND('',#10629,.T.);
#11745=FACE_BOUND('',#10630,.T.);
#11746=FACE_BOUND('',#10631,.T.);
#11747=FACE_BOUND('',#10632,.T.);
#11748=FACE_BOUND('',#10633,.T.);
#11749=FACE_BOUND('',#10634,.T.);
#11750=FACE_BOUND('',#10635,.T.);
#11751=FACE_BOUND('',#10636,.T.);
#11752=FACE_BOUND('',#10637,.T.);
#11753=FACE_BOUND('',#10638,.T.);
#11754=FACE_BOUND('',#10639,.T.);
#11755=FACE_BOUND('',#10640,.T.);
#11756=FACE_BOUND('',#10641,.T.);
#11757=FACE_BOUND('',#10642,.T.);
#11758=FACE_BOUND('',#10643,.T.);
#11759=FACE_BOUND('',#10644,.T.);
#11760=FACE_BOUND('',#10645,.T.);
#11761=FACE_BOUND('',#10646,.T.);
#11762=FACE_BOUND('',#10647,.T.);
#11763=FACE_BOUND('',#10648,.T.);
#11764=FACE_BOUND('',#10649,.T.);
#11765=FACE_BOUND('',#10650,.T.);
#11766=FACE_BOUND('',#10651,.T.);
#11767=FACE_BOUND('',#10652,.T.);
#11768=FACE_BOUND('',#10653,.T.);
#11769=FACE_BOUND('',#10654,.T.);
#11770=FACE_BOUND('',#10655,.T.);
#11771=FACE_BOUND('',#10656,.T.);
#11772=FACE_BOUND('',#10657,.T.);
#11773=FACE_BOUND('',#10658,.T.);
#11774=FACE_BOUND('',#10659,.T.);
#11775=FACE_BOUND('',#10660,.T.);
#11776=FACE_BOUND('',#10661,.T.);
#11777=FACE_BOUND('',#10662,.T.);
#11778=FACE_BOUND('',#10663,.T.);
#11779=FACE_BOUND('',#10664,.T.);
#11780=FACE_BOUND('',#10665,.T.);
#11781=FACE_BOUND('',#10666,.T.);
#11782=FACE_BOUND('',#10667,.T.);
#11783=FACE_BOUND('',#10668,.T.);
#11784=FACE_BOUND('',#10669,.T.);
#11785=FACE_BOUND('',#10670,.T.);
#11786=FACE_BOUND('',#10671,.T.);
#11787=FACE_BOUND('',#10672,.T.);
#11788=FACE_BOUND('',#10673,.T.);
#11789=FACE_BOUND('',#10674,.T.);
#11790=FACE_BOUND('',#10675,.T.);
#11791=FACE_BOUND('',#10676,.T.);
#11792=FACE_BOUND('',#10677,.T.);
#11793=FACE_BOUND('',#10678,.T.);
#11794=FACE_BOUND('',#10679,.T.);
#11795=FACE_BOUND('',#10680,.T.);
#11796=FACE_BOUND('',#10681,.T.);
#11797=FACE_BOUND('',#10682,.T.);
#11798=FACE_BOUND('',#10683,.T.);
#11799=FACE_BOUND('',#10684,.T.);
#11800=FACE_BOUND('',#10685,.T.);
#11801=FACE_BOUND('',#10686,.T.);
#11802=FACE_BOUND('',#10687,.T.);
#11803=FACE_BOUND('',#10688,.T.);
#11804=FACE_BOUND('',#10689,.T.);
#11805=FACE_BOUND('',#10690,.T.);
#11806=FACE_BOUND('',#10691,.T.);
#11807=FACE_BOUND('',#10692,.T.);
#11808=FACE_BOUND('',#10693,.T.);
#11809=FACE_BOUND('',#10694,.T.);
#11810=FACE_BOUND('',#10695,.T.);
#11811=FACE_BOUND('',#10696,.T.);
#11812=FACE_BOUND('',#10697,.T.);
#11813=FACE_BOUND('',#10698,.T.);
#11814=FACE_BOUND('',#10699,.T.);
#11815=FACE_BOUND('',#10700,.T.);
#11816=FACE_BOUND('',#10701,.T.);
#11817=FACE_BOUND('',#10702,.T.);
#11818=FACE_BOUND('',#10703,.T.);
#11819=FACE_BOUND('',#10704,.T.);
#11820=FACE_BOUND('',#10705,.T.);
#11821=FACE_BOUND('',#10706,.T.);
#11822=FACE_BOUND('',#10707,.T.);
#11823=FACE_BOUND('',#10708,.T.);
#11824=FACE_BOUND('',#10709,.T.);
#11825=FACE_BOUND('',#10710,.T.);
#11826=FACE_BOUND('',#10711,.T.);
#11827=FACE_BOUND('',#10712,.T.);
#11828=FACE_BOUND('',#10713,.T.);
#11829=FACE_BOUND('',#10714,.T.);
#11830=FACE_BOUND('',#10715,.T.);
#11831=FACE_BOUND('',#10716,.T.);
#11832=FACE_BOUND('',#10717,.T.);
#11833=FACE_BOUND('',#10718,.T.);
#11834=FACE_BOUND('',#10719,.T.);
#11835=FACE_BOUND('',#10720,.T.);
#11836=FACE_BOUND('',#10721,.T.);
#11837=FACE_BOUND('',#10722,.T.);
#11838=FACE_BOUND('',#10723,.T.);
#11839=FACE_BOUND('',#10724,.T.);
#11840=FACE_BOUND('',#10725,.T.);
#11841=FACE_BOUND('',#10726,.T.);
#11842=FACE_BOUND('',#10727,.T.);
#11843=FACE_BOUND('',#10728,.T.);
#11844=FACE_BOUND('',#10729,.T.);
#11845=FACE_BOUND('',#10730,.T.);
#11846=FACE_BOUND('',#10731,.T.);
#11847=FACE_BOUND('',#10732,.T.);
#11848=FACE_BOUND('',#10733,.T.);
#11849=FACE_BOUND('',#10734,.T.);
#11850=FACE_BOUND('',#10735,.T.);
#11851=FACE_BOUND('',#10736,.T.);
#11852=FACE_BOUND('',#10737,.T.);
#11853=FACE_BOUND('',#10738,.T.);
#11854=FACE_BOUND('',#10739,.T.);
#11855=FACE_BOUND('',#10740,.T.);
#11856=FACE_BOUND('',#10741,.T.);
#11857=FACE_BOUND('',#10742,.T.);
#11858=FACE_BOUND('',#10743,.T.);
#11859=FACE_BOUND('',#10744,.T.);
#11860=FACE_BOUND('',#10745,.T.);
#11861=FACE_BOUND('',#10746,.T.);
#11862=FACE_BOUND('',#10747,.T.);
#11863=FACE_BOUND('',#10748,.T.);
#11864=FACE_BOUND('',#10749,.T.);
#11865=FACE_BOUND('',#10750,.T.);
#11866=FACE_BOUND('',#10751,.T.);
#11867=FACE_BOUND('',#10752,.T.);
#11868=FACE_BOUND('',#10753,.T.);
#11869=FACE_BOUND('',#10754,.T.);
#11870=FACE_BOUND('',#10755,.T.);
#11871=FACE_BOUND('',#10756,.T.);
#11872=FACE_BOUND('',#10757,.T.);
#11873=FACE_BOUND('',#10758,.T.);
#11874=FACE_BOUND('',#10759,.T.);
#11875=FACE_BOUND('',#10760,.T.);
#11876=FACE_BOUND('',#10761,.T.);
#11877=FACE_BOUND('',#10762,.T.);
#11878=FACE_BOUND('',#10763,.T.);
#11879=FACE_BOUND('',#10764,.T.);
#11880=FACE_BOUND('',#10765,.T.);
#11881=FACE_BOUND('',#10766,.T.);
#11882=FACE_BOUND('',#10767,.T.);
#11883=FACE_BOUND('',#10768,.T.);
#11884=FACE_BOUND('',#10769,.T.);
#11885=FACE_BOUND('',#10770,.T.);
#11886=FACE_BOUND('',#10771,.T.);
#11887=FACE_BOUND('',#10772,.T.);
#11888=FACE_BOUND('',#10773,.T.);
#11889=FACE_BOUND('',#10774,.T.);
#11890=FACE_BOUND('',#10775,.T.);
#11891=FACE_BOUND('',#10776,.T.);
#11892=FACE_BOUND('',#10777,.T.);
#11893=FACE_BOUND('',#10778,.T.);
#11894=FACE_BOUND('',#10779,.T.);
#11895=FACE_BOUND('',#10780,.T.);
#11896=FACE_BOUND('',#10781,.T.);
#11897=FACE_BOUND('',#10782,.T.);
#11898=FACE_BOUND('',#10783,.T.);
#11899=FACE_BOUND('',#10784,.T.);
#11900=FACE_BOUND('',#10785,.T.);
#11901=FACE_BOUND('',#10,.T.);
#11902=FACE_BOUND('',#10786,.T.);
#11903=FACE_BOUND('',#11,.T.);
#11904=FACE_BOUND('',#10787,.T.);
#11905=FACE_BOUND('',#10788,.T.);
#11906=FACE_BOUND('',#10789,.T.);
#11907=FACE_BOUND('',#10790,.T.);
#11908=FACE_BOUND('',#10791,.T.);
#11909=FACE_BOUND('',#10792,.T.);
#11910=FACE_BOUND('',#10793,.T.);
#11911=FACE_BOUND('',#10794,.T.);
#11912=FACE_BOUND('',#10795,.T.);
#11913=FACE_BOUND('',#10796,.T.);
#11914=FACE_BOUND('',#10797,.T.);
#11915=FACE_BOUND('',#10798,.T.);
#11916=FACE_BOUND('',#10799,.T.);
#11917=FACE_BOUND('',#10800,.T.);
#11918=FACE_BOUND('',#10801,.T.);
#11919=FACE_BOUND('',#10802,.T.);
#11920=FACE_BOUND('',#10803,.T.);
#11921=FACE_BOUND('',#10804,.T.);
#11922=FACE_BOUND('',#10805,.T.);
#11923=FACE_BOUND('',#10806,.T.);
#11924=FACE_BOUND('',#10807,.T.);
#11925=FACE_BOUND('',#10808,.T.);
#11926=FACE_BOUND('',#10809,.T.);
#11927=FACE_BOUND('',#10810,.T.);
#11928=FACE_BOUND('',#10811,.T.);
#11929=FACE_BOUND('',#10812,.T.);
#11930=FACE_BOUND('',#10813,.T.);
#11931=FACE_BOUND('',#10814,.T.);
#11932=FACE_BOUND('',#10815,.T.);
#11933=FACE_BOUND('',#10816,.T.);
#11934=FACE_BOUND('',#10817,.T.);
#11935=FACE_BOUND('',#10818,.T.);
#11936=FACE_BOUND('',#10819,.T.);
#11937=FACE_BOUND('',#10820,.T.);
#11938=FACE_BOUND('',#10821,.T.);
#11939=FACE_BOUND('',#10822,.T.);
#11940=FACE_BOUND('',#10823,.T.);
#11941=FACE_BOUND('',#10824,.T.);
#11942=FACE_BOUND('',#10825,.T.);
#11943=FACE_BOUND('',#10826,.T.);
#11944=FACE_BOUND('',#10827,.T.);
#11945=FACE_BOUND('',#10828,.T.);
#11946=FACE_BOUND('',#10829,.T.);
#11947=FACE_BOUND('',#10830,.T.);
#11948=FACE_BOUND('',#10831,.T.);
#11949=FACE_BOUND('',#10832,.T.);
#11950=FACE_BOUND('',#10833,.T.);
#11951=FACE_BOUND('',#10834,.T.);
#11952=FACE_BOUND('',#10835,.T.);
#11953=FACE_BOUND('',#10836,.T.);
#11954=FACE_BOUND('',#10837,.T.);
#11955=FACE_BOUND('',#10838,.T.);
#11956=FACE_BOUND('',#10839,.T.);
#11957=FACE_BOUND('',#10840,.T.);
#11958=FACE_BOUND('',#10841,.T.);
#11959=FACE_BOUND('',#10842,.T.);
#11960=FACE_BOUND('',#10843,.T.);
#11961=FACE_BOUND('',#10844,.T.);
#11962=FACE_BOUND('',#10845,.T.);
#11963=FACE_BOUND('',#10846,.T.);
#11964=FACE_BOUND('',#10847,.T.);
#11965=FACE_BOUND('',#10848,.T.);
#11966=FACE_BOUND('',#10849,.T.);
#11967=FACE_BOUND('',#10850,.T.);
#11968=FACE_BOUND('',#10851,.T.);
#11969=FACE_BOUND('',#10852,.T.);
#11970=FACE_BOUND('',#10853,.T.);
#11971=FACE_BOUND('',#10854,.T.);
#11972=FACE_BOUND('',#10855,.T.);
#11973=FACE_BOUND('',#10856,.T.);
#11974=FACE_BOUND('',#10857,.T.);
#11975=FACE_BOUND('',#10858,.T.);
#11976=FACE_BOUND('',#10859,.T.);
#11977=FACE_BOUND('',#10860,.T.);
#11978=FACE_BOUND('',#10861,.T.);
#11979=FACE_BOUND('',#10862,.T.);
#11980=FACE_BOUND('',#10863,.T.);
#11981=FACE_BOUND('',#10864,.T.);
#11982=FACE_BOUND('',#10865,.T.);
#11983=FACE_BOUND('',#10866,.T.);
#11984=FACE_BOUND('',#10867,.T.);
#11985=FACE_BOUND('',#10868,.T.);
#11986=FACE_BOUND('',#10869,.T.);
#11987=FACE_BOUND('',#10870,.T.);
#11988=FACE_BOUND('',#10871,.T.);
#11989=FACE_BOUND('',#10872,.T.);
#11990=FACE_BOUND('',#10873,.T.);
#11991=FACE_BOUND('',#10874,.T.);
#11992=FACE_BOUND('',#10875,.T.);
#11993=FACE_BOUND('',#10876,.T.);
#11994=FACE_BOUND('',#10877,.T.);
#11995=FACE_BOUND('',#10878,.T.);
#11996=FACE_BOUND('',#10879,.T.);
#11997=FACE_BOUND('',#10880,.T.);
#11998=FACE_BOUND('',#10881,.T.);
#11999=FACE_BOUND('',#10882,.T.);
#12000=FACE_BOUND('',#10883,.T.);
#12001=FACE_BOUND('',#10884,.T.);
#12002=FACE_BOUND('',#10885,.T.);
#12003=FACE_BOUND('',#10886,.T.);
#12004=FACE_BOUND('',#10887,.T.);
#12005=FACE_BOUND('',#10888,.T.);
#12006=FACE_BOUND('',#10889,.T.);
#12007=FACE_BOUND('',#10890,.T.);
#12008=FACE_BOUND('',#10891,.T.);
#12009=FACE_BOUND('',#10892,.T.);
#12010=FACE_BOUND('',#10893,.T.);
#12011=FACE_BOUND('',#10894,.T.);
#12012=FACE_BOUND('',#10895,.T.);
#12013=FACE_BOUND('',#10896,.T.);
#12014=FACE_BOUND('',#10897,.T.);
#12015=FACE_BOUND('',#10898,.T.);
#12016=FACE_BOUND('',#10899,.T.);
#12017=FACE_BOUND('',#10900,.T.);
#12018=FACE_BOUND('',#10901,.T.);
#12019=FACE_BOUND('',#10902,.T.);
#12020=FACE_BOUND('',#10903,.T.);
#12021=FACE_BOUND('',#10904,.T.);
#12022=FACE_BOUND('',#10905,.T.);
#12023=FACE_BOUND('',#10906,.T.);
#12024=FACE_BOUND('',#10907,.T.);
#12025=FACE_BOUND('',#10908,.T.);
#12026=FACE_BOUND('',#10909,.T.);
#12027=FACE_BOUND('',#10910,.T.);
#12028=FACE_BOUND('',#10911,.T.);
#12029=FACE_BOUND('',#10912,.T.);
#12030=FACE_BOUND('',#10913,.T.);
#12031=FACE_BOUND('',#10914,.T.);
#12032=FACE_BOUND('',#10915,.T.);
#12033=FACE_BOUND('',#10916,.T.);
#12034=FACE_BOUND('',#10917,.T.);
#12035=FACE_BOUND('',#10918,.T.);
#12036=FACE_BOUND('',#10919,.T.);
#12037=FACE_BOUND('',#10920,.T.);
#12038=FACE_BOUND('',#10921,.T.);
#12039=FACE_BOUND('',#10922,.T.);
#12040=FACE_BOUND('',#10923,.T.);
#12041=FACE_BOUND('',#10924,.T.);
#12042=FACE_BOUND('',#10925,.T.);
#12043=FACE_BOUND('',#10926,.T.);
#12044=FACE_BOUND('',#10927,.T.);
#12045=FACE_BOUND('',#10928,.T.);
#12046=FACE_BOUND('',#10929,.T.);
#12047=FACE_BOUND('',#10930,.T.);
#12048=FACE_BOUND('',#10931,.T.);
#12049=FACE_BOUND('',#10932,.T.);
#12050=FACE_BOUND('',#10933,.T.);
#12051=FACE_BOUND('',#10934,.T.);
#12052=FACE_BOUND('',#10935,.T.);
#12053=FACE_BOUND('',#10936,.T.);
#12054=FACE_BOUND('',#10937,.T.);
#12055=FACE_BOUND('',#10938,.T.);
#12056=FACE_BOUND('',#10939,.T.);
#12057=FACE_BOUND('',#10940,.T.);
#12058=FACE_BOUND('',#10941,.T.);
#12059=FACE_BOUND('',#10942,.T.);
#12060=FACE_BOUND('',#10943,.T.);
#12061=FACE_BOUND('',#10944,.T.);
#12062=FACE_BOUND('',#10945,.T.);
#12063=FACE_BOUND('',#10946,.T.);
#12064=FACE_BOUND('',#10947,.T.);
#12065=FACE_BOUND('',#10948,.T.);
#12066=FACE_BOUND('',#10949,.T.);
#12067=FACE_BOUND('',#10950,.T.);
#12068=FACE_BOUND('',#10951,.T.);
#12069=FACE_BOUND('',#10952,.T.);
#12070=FACE_BOUND('',#10953,.T.);
#12071=FACE_BOUND('',#10954,.T.);
#12072=FACE_BOUND('',#10955,.T.);
#12073=FACE_BOUND('',#10956,.T.);
#12074=FACE_BOUND('',#10957,.T.);
#12075=FACE_BOUND('',#10958,.T.);
#12076=FACE_BOUND('',#10959,.T.);
#12077=FACE_BOUND('',#10960,.T.);
#12078=FACE_BOUND('',#10961,.T.);
#12079=FACE_BOUND('',#10962,.T.);
#12080=FACE_BOUND('',#10963,.T.);
#12081=FACE_BOUND('',#10964,.T.);
#12082=FACE_BOUND('',#10965,.T.);
#12083=FACE_BOUND('',#10966,.T.);
#12084=FACE_BOUND('',#10967,.T.);
#12085=FACE_BOUND('',#10968,.T.);
#12086=FACE_BOUND('',#10969,.T.);
#12087=FACE_BOUND('',#10970,.T.);
#12088=FACE_BOUND('',#10971,.T.);
#12089=FACE_BOUND('',#10972,.T.);
#12090=FACE_BOUND('',#10973,.T.);
#12091=FACE_BOUND('',#10974,.T.);
#12092=FACE_BOUND('',#10975,.T.);
#12093=FACE_BOUND('',#10976,.T.);
#12094=FACE_BOUND('',#10977,.T.);
#12095=FACE_BOUND('',#10978,.T.);
#12096=FACE_BOUND('',#10979,.T.);
#12097=FACE_BOUND('',#10980,.T.);
#12098=FACE_BOUND('',#10981,.T.);
#12099=FACE_BOUND('',#10982,.T.);
#12100=FACE_BOUND('',#10983,.T.);
#12101=FACE_BOUND('',#10984,.T.);
#12102=FACE_BOUND('',#10985,.T.);
#12103=FACE_BOUND('',#10986,.T.);
#12104=FACE_BOUND('',#10987,.T.);
#12105=FACE_BOUND('',#10988,.T.);
#12106=FACE_BOUND('',#10989,.T.);
#12107=FACE_BOUND('',#10990,.T.);
#12108=FACE_BOUND('',#10991,.T.);
#12109=FACE_BOUND('',#10992,.T.);
#12110=FACE_BOUND('',#10993,.T.);
#12111=FACE_BOUND('',#10994,.T.);
#12112=FACE_BOUND('',#10995,.T.);
#12113=FACE_BOUND('',#10996,.T.);
#12114=FACE_BOUND('',#10997,.T.);
#12115=FACE_BOUND('',#10998,.T.);
#12116=FACE_BOUND('',#10999,.T.);
#12117=FACE_BOUND('',#11000,.T.);
#12118=FACE_BOUND('',#11001,.T.);
#12119=FACE_BOUND('',#11002,.T.);
#12120=FACE_BOUND('',#11003,.T.);
#12121=FACE_BOUND('',#11004,.T.);
#12122=FACE_BOUND('',#11005,.T.);
#12123=FACE_BOUND('',#11006,.T.);
#12124=FACE_BOUND('',#11007,.T.);
#12125=FACE_BOUND('',#11008,.T.);
#12126=FACE_BOUND('',#11009,.T.);
#12127=FACE_BOUND('',#11010,.T.);
#12128=FACE_BOUND('',#11011,.T.);
#12129=FACE_BOUND('',#11012,.T.);
#12130=FACE_BOUND('',#11013,.T.);
#12131=FACE_BOUND('',#11014,.T.);
#12132=FACE_BOUND('',#11015,.T.);
#12133=FACE_BOUND('',#11016,.T.);
#12134=FACE_BOUND('',#11017,.T.);
#12135=FACE_BOUND('',#11018,.T.);
#12136=FACE_BOUND('',#11019,.T.);
#12137=FACE_BOUND('',#11020,.T.);
#12138=FACE_BOUND('',#11021,.T.);
#12139=FACE_BOUND('',#11022,.T.);
#12140=FACE_BOUND('',#11023,.T.);
#12141=FACE_BOUND('',#11024,.T.);
#12142=FACE_BOUND('',#11025,.T.);
#12143=FACE_BOUND('',#11026,.T.);
#12144=FACE_BOUND('',#11027,.T.);
#12145=FACE_BOUND('',#11028,.T.);
#12146=FACE_BOUND('',#11029,.T.);
#12147=FACE_BOUND('',#11030,.T.);
#12148=FACE_BOUND('',#11031,.T.);
#12149=FACE_BOUND('',#11032,.T.);
#12150=FACE_BOUND('',#11033,.T.);
#12151=FACE_BOUND('',#11034,.T.);
#12152=FACE_BOUND('',#11035,.T.);
#12153=FACE_BOUND('',#11036,.T.);
#12154=FACE_BOUND('',#11037,.T.);
#12155=FACE_BOUND('',#11038,.T.);
#12156=FACE_BOUND('',#11039,.T.);
#12157=FACE_BOUND('',#11040,.T.);
#12158=FACE_BOUND('',#11041,.T.);
#12159=FACE_BOUND('',#11042,.T.);
#12160=FACE_BOUND('',#11043,.T.);
#12161=FACE_BOUND('',#11044,.T.);
#12162=FACE_BOUND('',#11045,.T.);
#12163=FACE_BOUND('',#11046,.T.);
#12164=FACE_BOUND('',#11047,.T.);
#12165=FACE_BOUND('',#11048,.T.);
#12166=FACE_BOUND('',#11049,.T.);
#12167=FACE_BOUND('',#11050,.T.);
#12168=FACE_BOUND('',#11051,.T.);
#12169=FACE_BOUND('',#11052,.T.);
#12170=FACE_BOUND('',#11053,.T.);
#12171=FACE_BOUND('',#11054,.T.);
#12172=FACE_BOUND('',#11055,.T.);
#12173=FACE_BOUND('',#11056,.T.);
#12174=FACE_BOUND('',#11057,.T.);
#12175=FACE_BOUND('',#11058,.T.);
#12176=FACE_BOUND('',#11059,.T.);
#12177=FACE_BOUND('',#11060,.T.);
#12178=FACE_BOUND('',#11061,.T.);
#12179=FACE_BOUND('',#11062,.T.);
#12180=FACE_BOUND('',#11063,.T.);
#12181=FACE_BOUND('',#11064,.T.);
#12182=FACE_BOUND('',#11065,.T.);
#12183=FACE_BOUND('',#11066,.T.);
#12184=FACE_BOUND('',#11067,.T.);
#12185=FACE_BOUND('',#11068,.T.);
#12186=FACE_BOUND('',#11069,.T.);
#12187=FACE_BOUND('',#11070,.T.);
#12188=FACE_BOUND('',#11071,.T.);
#12189=FACE_BOUND('',#11072,.T.);
#12190=FACE_BOUND('',#11073,.T.);
#12191=FACE_BOUND('',#11074,.T.);
#12192=FACE_BOUND('',#11075,.T.);
#12193=FACE_BOUND('',#11076,.T.);
#12194=FACE_BOUND('',#11077,.T.);
#12195=FACE_BOUND('',#11078,.T.);
#12196=FACE_BOUND('',#11079,.T.);
#12197=FACE_BOUND('',#11080,.T.);
#12198=FACE_BOUND('',#11081,.T.);
#12199=FACE_BOUND('',#11082,.T.);
#12200=FACE_BOUND('',#11083,.T.);
#12201=FACE_BOUND('',#11084,.T.);
#12202=FACE_BOUND('',#11085,.T.);
#12203=FACE_BOUND('',#11086,.T.);
#12204=FACE_BOUND('',#11087,.T.);
#12205=FACE_BOUND('',#11088,.T.);
#12206=FACE_BOUND('',#11089,.T.);
#12207=FACE_BOUND('',#11090,.T.);
#12208=FACE_BOUND('',#11091,.T.);
#12209=FACE_BOUND('',#12,.T.);
#12210=FACE_BOUND('',#11092,.T.);
#12211=FACE_BOUND('',#11093,.T.);
#12212=FACE_BOUND('',#11094,.T.);
#12213=FACE_BOUND('',#11095,.T.);
#12214=FACE_BOUND('',#11096,.T.);
#12215=FACE_BOUND('',#11097,.T.);
#12216=FACE_BOUND('',#11098,.T.);
#12217=FACE_BOUND('',#11099,.T.);
#12218=FACE_BOUND('',#11100,.T.);
#12219=FACE_BOUND('',#11101,.T.);
#12220=FACE_BOUND('',#11102,.T.);
#12221=FACE_BOUND('',#11103,.T.);
#12222=FACE_BOUND('',#11104,.T.);
#12223=FACE_BOUND('',#11105,.T.);
#12224=FACE_BOUND('',#11106,.T.);
#12225=FACE_BOUND('',#11107,.T.);
#12226=FACE_BOUND('',#11108,.T.);
#12227=FACE_BOUND('',#11109,.T.);
#12228=FACE_BOUND('',#11110,.T.);
#12229=FACE_BOUND('',#11111,.T.);
#12230=FACE_BOUND('',#11112,.T.);
#12231=FACE_BOUND('',#11113,.T.);
#12232=FACE_BOUND('',#11114,.T.);
#12233=FACE_BOUND('',#11115,.T.);
#12234=FACE_BOUND('',#11116,.T.);
#12235=FACE_BOUND('',#11117,.T.);
#12236=FACE_BOUND('',#11118,.T.);
#12237=FACE_BOUND('',#11119,.T.);
#12238=FACE_BOUND('',#11120,.T.);
#12239=FACE_BOUND('',#11121,.T.);
#12240=FACE_BOUND('',#11122,.T.);
#12241=FACE_BOUND('',#11123,.T.);
#12242=FACE_BOUND('',#11124,.T.);
#12243=FACE_BOUND('',#11125,.T.);
#12244=FACE_BOUND('',#11126,.T.);
#12245=FACE_BOUND('',#11127,.T.);
#12246=FACE_BOUND('',#11128,.T.);
#12247=FACE_BOUND('',#11129,.T.);
#12248=FACE_BOUND('',#11130,.T.);
#12249=FACE_BOUND('',#11131,.T.);
#12250=FACE_BOUND('',#11132,.T.);
#12251=FACE_BOUND('',#11133,.T.);
#12252=FACE_BOUND('',#11134,.T.);
#12253=FACE_BOUND('',#11135,.T.);
#12254=FACE_BOUND('',#11136,.T.);
#12255=FACE_BOUND('',#11137,.T.);
#12256=FACE_BOUND('',#11138,.T.);
#12257=FACE_BOUND('',#11139,.T.);
#12258=FACE_BOUND('',#11140,.T.);
#12259=FACE_BOUND('',#11141,.T.);
#12260=FACE_BOUND('',#11142,.T.);
#12261=FACE_BOUND('',#11143,.T.);
#12262=FACE_BOUND('',#11144,.T.);
#12263=FACE_BOUND('',#11145,.T.);
#12264=FACE_BOUND('',#11146,.T.);
#12265=FACE_BOUND('',#11147,.T.);
#12266=FACE_BOUND('',#11148,.T.);
#12267=FACE_BOUND('',#11149,.T.);
#12268=FACE_BOUND('',#13,.T.);
#12269=FACE_BOUND('',#11150,.T.);
#12270=FACE_BOUND('',#11151,.T.);
#12271=FACE_BOUND('',#11152,.T.);
#12272=FACE_BOUND('',#11153,.T.);
#12273=FACE_BOUND('',#11154,.T.);
#12274=FACE_BOUND('',#11155,.T.);
#12275=FACE_BOUND('',#11156,.T.);
#12276=FACE_BOUND('',#11157,.T.);
#12277=FACE_BOUND('',#11158,.T.);
#12278=FACE_BOUND('',#11159,.T.);
#12279=FACE_BOUND('',#11160,.T.);
#12280=FACE_BOUND('',#11161,.T.);
#12281=FACE_BOUND('',#11162,.T.);
#12282=FACE_BOUND('',#11163,.T.);
#12283=FACE_BOUND('',#11164,.T.);
#12284=FACE_BOUND('',#11165,.T.);
#12285=FACE_BOUND('',#11166,.T.);
#12286=FACE_BOUND('',#11167,.T.);
#12287=FACE_BOUND('',#11168,.T.);
#12288=FACE_BOUND('',#11169,.T.);
#12289=FACE_BOUND('',#11170,.T.);
#12290=FACE_BOUND('',#11171,.T.);
#12291=FACE_BOUND('',#11172,.T.);
#12292=FACE_BOUND('',#11173,.T.);
#12293=FACE_BOUND('',#11174,.T.);
#12294=FACE_BOUND('',#11175,.T.);
#12295=FACE_BOUND('',#11176,.T.);
#12296=FACE_BOUND('',#11177,.T.);
#12297=FACE_BOUND('',#11178,.T.);
#12298=FACE_BOUND('',#11179,.T.);
#12299=FACE_BOUND('',#11180,.T.);
#12300=FACE_BOUND('',#11181,.T.);
#12301=FACE_BOUND('',#11182,.T.);
#12302=FACE_BOUND('',#11183,.T.);
#12303=FACE_BOUND('',#11184,.T.);
#12304=FACE_BOUND('',#11185,.T.);
#12305=FACE_BOUND('',#11186,.T.);
#12306=FACE_BOUND('',#11187,.T.);
#12307=FACE_BOUND('',#11188,.T.);
#12308=FACE_BOUND('',#11189,.T.);
#12309=FACE_BOUND('',#11190,.T.);
#12310=FACE_BOUND('',#11191,.T.);
#12311=FACE_BOUND('',#11192,.T.);
#12312=FACE_BOUND('',#11193,.T.);
#12313=FACE_BOUND('',#11194,.T.);
#12314=FACE_BOUND('',#11195,.T.);
#12315=FACE_BOUND('',#11196,.T.);
#12316=FACE_BOUND('',#11197,.T.);
#12317=FACE_BOUND('',#11198,.T.);
#12318=FACE_BOUND('',#11199,.T.);
#12319=FACE_BOUND('',#11200,.T.);
#12320=FACE_BOUND('',#11201,.T.);
#12321=FACE_BOUND('',#11202,.T.);
#12322=FACE_BOUND('',#11203,.T.);
#12323=FACE_BOUND('',#11204,.T.);
#12324=FACE_BOUND('',#11205,.T.);
#12325=FACE_BOUND('',#11206,.T.);
#12326=FACE_BOUND('',#11207,.T.);
#12327=FACE_BOUND('',#11208,.T.);
#12328=FACE_BOUND('',#11209,.T.);
#12329=FACE_BOUND('',#11210,.T.);
#12330=FACE_BOUND('',#11211,.T.);
#12331=FACE_BOUND('',#11212,.T.);
#12332=FACE_BOUND('',#11213,.T.);
#12333=FACE_BOUND('',#11214,.T.);
#12334=FACE_BOUND('',#11215,.T.);
#12335=FACE_BOUND('',#11216,.T.);
#12336=FACE_BOUND('',#11217,.T.);
#12337=FACE_BOUND('',#11218,.T.);
#12338=FACE_BOUND('',#11219,.T.);
#12339=FACE_BOUND('',#11220,.T.);
#12340=FACE_BOUND('',#11221,.T.);
#12341=FACE_BOUND('',#11222,.T.);
#12342=FACE_BOUND('',#11223,.T.);
#12343=FACE_BOUND('',#11224,.T.);
#12344=FACE_BOUND('',#11225,.T.);
#12345=FACE_BOUND('',#11226,.T.);
#12346=FACE_BOUND('',#11227,.T.);
#12347=FACE_BOUND('',#11228,.T.);
#12348=FACE_BOUND('',#11229,.T.);
#12349=FACE_BOUND('',#11230,.T.);
#12350=FACE_BOUND('',#11231,.T.);
#12351=FACE_BOUND('',#11232,.T.);
#12352=FACE_BOUND('',#11233,.T.);
#12353=FACE_BOUND('',#11234,.T.);
#12354=FACE_BOUND('',#11235,.T.);
#12355=FACE_BOUND('',#11236,.T.);
#12356=FACE_BOUND('',#11237,.T.);
#12357=FACE_BOUND('',#11238,.T.);
#12358=FACE_BOUND('',#11239,.T.);
#12359=FACE_BOUND('',#11240,.T.);
#12360=FACE_BOUND('',#11241,.T.);
#12361=FACE_BOUND('',#11242,.T.);
#12362=FACE_BOUND('',#11243,.T.);
#12363=FACE_BOUND('',#11244,.T.);
#12364=FACE_BOUND('',#11245,.T.);
#12365=FACE_BOUND('',#11246,.T.);
#12366=FACE_BOUND('',#11247,.T.);
#12367=FACE_BOUND('',#11248,.T.);
#12368=FACE_BOUND('',#11249,.T.);
#12369=FACE_BOUND('',#11250,.T.);
#12370=FACE_BOUND('',#11251,.T.);
#12371=FACE_BOUND('',#11252,.T.);
#12372=FACE_BOUND('',#11253,.T.);
#12373=FACE_BOUND('',#11254,.T.);
#12374=FACE_BOUND('',#11255,.T.);
#12375=FACE_BOUND('',#11256,.T.);
#12376=FACE_BOUND('',#11257,.T.);
#12377=FACE_BOUND('',#11258,.T.);
#12378=FACE_BOUND('',#11259,.T.);
#12379=FACE_BOUND('',#11260,.T.);
#12380=FACE_BOUND('',#11261,.T.);
#12381=FACE_BOUND('',#11262,.T.);
#12382=FACE_BOUND('',#11263,.T.);
#12383=FACE_BOUND('',#11264,.T.);
#12384=FACE_BOUND('',#11265,.T.);
#12385=FACE_BOUND('',#11266,.T.);
#12386=FACE_BOUND('',#11267,.T.);
#12387=FACE_BOUND('',#11268,.T.);
#12388=FACE_BOUND('',#11269,.T.);
#12389=FACE_BOUND('',#11270,.T.);
#12390=FACE_BOUND('',#11271,.T.);
#12391=FACE_BOUND('',#11272,.T.);
#12392=FACE_BOUND('',#11273,.T.);
#12393=FACE_BOUND('',#11274,.T.);
#12394=FACE_BOUND('',#11275,.T.);
#12395=FACE_BOUND('',#11276,.T.);
#12396=FACE_BOUND('',#11277,.T.);
#12397=FACE_BOUND('',#11278,.T.);
#12398=FACE_BOUND('',#11279,.T.);
#12399=FACE_BOUND('',#11280,.T.);
#12400=FACE_BOUND('',#11281,.T.);
#12401=FACE_BOUND('',#11282,.T.);
#12402=FACE_BOUND('',#11283,.T.);
#12403=FACE_BOUND('',#11284,.T.);
#12404=FACE_BOUND('',#11285,.T.);
#12405=FACE_BOUND('',#11286,.T.);
#12406=FACE_BOUND('',#11287,.T.);
#12407=FACE_BOUND('',#11288,.T.);
#12408=FACE_BOUND('',#11289,.T.);
#12409=FACE_BOUND('',#11290,.T.);
#12410=FACE_BOUND('',#11291,.T.);
#12411=FACE_BOUND('',#11292,.T.);
#12412=FACE_BOUND('',#11293,.T.);
#12413=FACE_BOUND('',#11294,.T.);
#12414=FACE_BOUND('',#11295,.T.);
#12415=FACE_BOUND('',#11296,.T.);
#12416=FACE_BOUND('',#11297,.T.);
#12417=FACE_BOUND('',#11298,.T.);
#12418=FACE_BOUND('',#11299,.T.);
#12419=FACE_BOUND('',#11300,.T.);
#12420=FACE_BOUND('',#11301,.T.);
#12421=FACE_BOUND('',#11302,.T.);
#12422=FACE_BOUND('',#11303,.T.);
#12423=FACE_BOUND('',#11304,.T.);
#12424=FACE_BOUND('',#11305,.T.);
#12425=FACE_BOUND('',#11306,.T.);
#12426=FACE_BOUND('',#11307,.T.);
#12427=FACE_BOUND('',#11308,.T.);
#12428=FACE_BOUND('',#11309,.T.);
#12429=FACE_BOUND('',#11310,.T.);
#12430=FACE_BOUND('',#11311,.T.);
#12431=FACE_BOUND('',#11312,.T.);
#12432=FACE_BOUND('',#11313,.T.);
#12433=FACE_BOUND('',#11314,.T.);
#12434=FACE_BOUND('',#11315,.T.);
#12435=FACE_BOUND('',#11316,.T.);
#12436=FACE_BOUND('',#11317,.T.);
#12437=FACE_BOUND('',#11318,.T.);
#12438=FACE_BOUND('',#11319,.T.);
#12439=FACE_BOUND('',#11320,.T.);
#12440=FACE_BOUND('',#11321,.T.);
#12441=FACE_BOUND('',#11322,.T.);
#12442=FACE_BOUND('',#11323,.T.);
#12443=FACE_BOUND('',#11324,.T.);
#12444=FACE_BOUND('',#11325,.T.);
#12445=FACE_BOUND('',#11326,.T.);
#12446=FACE_BOUND('',#11327,.T.);
#12447=FACE_BOUND('',#11328,.T.);
#12448=FACE_BOUND('',#11329,.T.);
#12449=FACE_BOUND('',#11330,.T.);
#12450=FACE_BOUND('',#11331,.T.);
#12451=FACE_BOUND('',#11332,.T.);
#12452=FACE_BOUND('',#11333,.T.);
#12453=FACE_BOUND('',#11334,.T.);
#12454=FACE_BOUND('',#11335,.T.);
#12455=FACE_BOUND('',#11336,.T.);
#12456=FACE_BOUND('',#11337,.T.);
#12457=FACE_BOUND('',#11338,.T.);
#12458=FACE_BOUND('',#11339,.T.);
#12459=FACE_BOUND('',#11340,.T.);
#12460=FACE_BOUND('',#11341,.T.);
#12461=FACE_BOUND('',#11342,.T.);
#12462=FACE_BOUND('',#11343,.T.);
#12463=FACE_BOUND('',#11344,.T.);
#12464=FACE_BOUND('',#11345,.T.);
#12465=FACE_BOUND('',#11346,.T.);
#12466=FACE_BOUND('',#11347,.T.);
#12467=FACE_BOUND('',#11348,.T.);
#12468=FACE_BOUND('',#11349,.T.);
#12469=FACE_BOUND('',#11350,.T.);
#12470=FACE_BOUND('',#11351,.T.);
#12471=FACE_BOUND('',#11352,.T.);
#12472=FACE_BOUND('',#11353,.T.);
#12473=FACE_BOUND('',#11354,.T.);
#12474=FACE_BOUND('',#11355,.T.);
#12475=FACE_BOUND('',#11356,.T.);
#12476=FACE_BOUND('',#11357,.T.);
#12477=FACE_BOUND('',#11358,.T.);
#12478=FACE_BOUND('',#11359,.T.);
#12479=FACE_BOUND('',#11360,.T.);
#12480=FACE_BOUND('',#11361,.T.);
#12481=FACE_BOUND('',#11362,.T.);
#12482=FACE_BOUND('',#11363,.T.);
#12483=FACE_BOUND('',#11364,.T.);
#12484=FACE_BOUND('',#11365,.T.);
#12485=FACE_BOUND('',#11366,.T.);
#12486=FACE_BOUND('',#11367,.T.);
#12487=FACE_BOUND('',#11368,.T.);
#12488=FACE_BOUND('',#11369,.T.);
#12489=FACE_BOUND('',#11370,.T.);
#12490=FACE_BOUND('',#11371,.T.);
#12491=FACE_BOUND('',#11372,.T.);
#12492=FACE_BOUND('',#11373,.T.);
#12493=FACE_BOUND('',#11374,.T.);
#12494=FACE_BOUND('',#11375,.T.);
#12495=FACE_BOUND('',#11376,.T.);
#12496=FACE_BOUND('',#11377,.T.);
#12497=FACE_BOUND('',#11378,.T.);
#12498=FACE_BOUND('',#11379,.T.);
#12499=FACE_BOUND('',#11380,.T.);
#12500=FACE_BOUND('',#11381,.T.);
#12501=FACE_BOUND('',#11382,.T.);
#12502=FACE_BOUND('',#11383,.T.);
#12503=FACE_BOUND('',#11384,.T.);
#12504=FACE_BOUND('',#11385,.T.);
#12505=FACE_BOUND('',#11386,.T.);
#12506=FACE_BOUND('',#11387,.T.);
#12507=FACE_BOUND('',#11388,.T.);
#12508=FACE_BOUND('',#11389,.T.);
#12509=FACE_BOUND('',#11390,.T.);
#12510=FACE_BOUND('',#11391,.T.);
#12511=FACE_BOUND('',#11392,.T.);
#12512=FACE_BOUND('',#11393,.T.);
#12513=FACE_BOUND('',#11394,.T.);
#12514=FACE_BOUND('',#11395,.T.);
#12515=FACE_BOUND('',#11396,.T.);
#12516=FACE_BOUND('',#11397,.T.);
#12517=FACE_BOUND('',#11398,.T.);
#12518=FACE_BOUND('',#11399,.T.);
#12519=FACE_BOUND('',#11400,.T.);
#12520=FACE_BOUND('',#11401,.T.);
#12521=FACE_BOUND('',#11402,.T.);
#12522=FACE_BOUND('',#11403,.T.);
#12523=FACE_BOUND('',#11404,.T.);
#12524=FACE_BOUND('',#11405,.T.);
#12525=FACE_BOUND('',#11406,.T.);
#12526=FACE_BOUND('',#11407,.T.);
#12527=FACE_BOUND('',#11408,.T.);
#12528=FACE_BOUND('',#11409,.T.);
#12529=FACE_BOUND('',#11410,.T.);
#12530=FACE_BOUND('',#11411,.T.);
#12531=FACE_BOUND('',#11412,.T.);
#12532=FACE_BOUND('',#11413,.T.);
#12533=FACE_BOUND('',#11414,.T.);
#12534=FACE_BOUND('',#11415,.T.);
#12535=FACE_BOUND('',#11416,.T.);
#12536=FACE_BOUND('',#11417,.T.);
#12537=FACE_BOUND('',#11418,.T.);
#12538=FACE_BOUND('',#11419,.T.);
#12539=FACE_BOUND('',#11420,.T.);
#12540=FACE_BOUND('',#11421,.T.);
#12541=FACE_BOUND('',#11422,.T.);
#12542=FACE_BOUND('',#11423,.T.);
#12543=FACE_BOUND('',#11424,.T.);
#12544=FACE_BOUND('',#11425,.T.);
#12545=FACE_BOUND('',#11426,.T.);
#12546=FACE_BOUND('',#11427,.T.);
#12547=FACE_BOUND('',#11428,.T.);
#12548=FACE_BOUND('',#11429,.T.);
#12549=FACE_BOUND('',#11430,.T.);
#12550=FACE_BOUND('',#11431,.T.);
#12551=FACE_BOUND('',#11432,.T.);
#12552=FACE_BOUND('',#11433,.T.);
#12553=FACE_BOUND('',#11434,.T.);
#12554=FACE_BOUND('',#11435,.T.);
#12555=FACE_BOUND('',#11436,.T.);
#12556=FACE_BOUND('',#11437,.T.);
#12557=FACE_BOUND('',#11438,.T.);
#12558=FACE_BOUND('',#11439,.T.);
#12559=FACE_BOUND('',#11440,.T.);
#12560=FACE_BOUND('',#11441,.T.);
#12561=FACE_BOUND('',#11442,.T.);
#12562=FACE_BOUND('',#11443,.T.);
#12563=FACE_BOUND('',#11444,.T.);
#12564=FACE_BOUND('',#11445,.T.);
#12565=FACE_BOUND('',#11446,.T.);
#12566=FACE_BOUND('',#11447,.T.);
#12567=FACE_BOUND('',#11448,.T.);
#12568=FACE_BOUND('',#11449,.T.);
#12569=FACE_BOUND('',#11450,.T.);
#12570=FACE_BOUND('',#11451,.T.);
#12571=FACE_BOUND('',#11452,.T.);
#12572=FACE_BOUND('',#11453,.T.);
#12573=FACE_BOUND('',#11454,.T.);
#12574=FACE_BOUND('',#11455,.T.);
#12575=FACE_BOUND('',#11456,.T.);
#12576=FACE_BOUND('',#11457,.T.);
#12577=FACE_BOUND('',#11458,.T.);
#12578=FACE_BOUND('',#11459,.T.);
#12579=FACE_BOUND('',#11460,.T.);
#12580=FACE_BOUND('',#11461,.T.);
#12581=FACE_BOUND('',#11462,.T.);
#12582=FACE_BOUND('',#11463,.T.);
#12583=FACE_BOUND('',#11464,.T.);
#12584=FACE_BOUND('',#11465,.T.);
#12585=FACE_BOUND('',#11466,.T.);
#12586=FACE_BOUND('',#11467,.T.);
#12587=FACE_BOUND('',#11468,.T.);
#12588=FACE_BOUND('',#11469,.T.);
#12589=FACE_BOUND('',#11470,.T.);
#12590=FACE_BOUND('',#11471,.T.);
#12591=FACE_BOUND('',#11472,.T.);
#12592=FACE_BOUND('',#11473,.T.);
#12593=FACE_BOUND('',#11474,.T.);
#12594=FACE_BOUND('',#11475,.T.);
#12595=FACE_BOUND('',#11476,.T.);
#12596=FACE_BOUND('',#11477,.T.);
#12597=FACE_BOUND('',#11478,.T.);
#12598=FACE_BOUND('',#11479,.T.);
#12599=FACE_BOUND('',#11480,.T.);
#12600=FACE_BOUND('',#11481,.T.);
#12601=FACE_BOUND('',#11482,.T.);
#12602=FACE_BOUND('',#11483,.T.);
#12603=FACE_BOUND('',#11484,.T.);
#12604=FACE_BOUND('',#11485,.T.);
#12605=FACE_BOUND('',#11486,.T.);
#12606=FACE_BOUND('',#11487,.T.);
#12607=FACE_BOUND('',#11488,.T.);
#12608=FACE_BOUND('',#11489,.T.);
#12609=FACE_BOUND('',#11490,.T.);
#12610=FACE_BOUND('',#11491,.T.);
#12611=FACE_BOUND('',#11492,.T.);
#12612=FACE_BOUND('',#11493,.T.);
#12613=FACE_BOUND('',#11494,.T.);
#12614=FACE_BOUND('',#11495,.T.);
#12615=FACE_BOUND('',#11496,.T.);
#12616=FACE_BOUND('',#11497,.T.);
#12617=FACE_BOUND('',#11498,.T.);
#12618=FACE_BOUND('',#11499,.T.);
#12619=FACE_BOUND('',#11500,.T.);
#12620=FACE_BOUND('',#11501,.T.);
#12621=FACE_BOUND('',#11502,.T.);
#12622=FACE_BOUND('',#11503,.T.);
#12623=FACE_BOUND('',#11504,.T.);
#12624=FACE_BOUND('',#11505,.T.);
#12625=FACE_BOUND('',#11506,.T.);
#12626=FACE_BOUND('',#11507,.T.);
#12627=FACE_BOUND('',#11508,.T.);
#12628=FACE_BOUND('',#11509,.T.);
#12629=FACE_BOUND('',#11510,.T.);
#12630=FACE_BOUND('',#11511,.T.);
#12631=FACE_BOUND('',#11512,.T.);
#12632=FACE_BOUND('',#11513,.T.);
#12633=FACE_BOUND('',#11514,.T.);
#12634=FACE_BOUND('',#11515,.T.);
#12635=FACE_BOUND('',#11516,.T.);
#12636=FACE_BOUND('',#11517,.T.);
#12637=FACE_BOUND('',#11518,.T.);
#12638=FACE_BOUND('',#11519,.T.);
#12639=FACE_BOUND('',#11520,.T.);
#12640=FACE_BOUND('',#11521,.T.);
#12641=FACE_BOUND('',#11522,.T.);
#12642=FACE_BOUND('',#11523,.T.);
#12643=FACE_BOUND('',#11524,.T.);
#12644=FACE_BOUND('',#11525,.T.);
#12645=FACE_BOUND('',#11526,.T.);
#12646=FACE_BOUND('',#11527,.T.);
#12647=FACE_BOUND('',#11528,.T.);
#12648=FACE_BOUND('',#11529,.T.);
#12649=FACE_BOUND('',#11530,.T.);
#12650=FACE_BOUND('',#11531,.T.);
#12651=FACE_BOUND('',#11532,.T.);
#12652=FACE_BOUND('',#11533,.T.);
#12653=FACE_BOUND('',#11534,.T.);
#12654=FACE_BOUND('',#11535,.T.);
#12655=FACE_BOUND('',#11536,.T.);
#12656=FACE_BOUND('',#11537,.T.);
#12657=FACE_BOUND('',#11538,.T.);
#12658=FACE_BOUND('',#11539,.T.);
#12659=FACE_BOUND('',#11540,.T.);
#12660=FACE_BOUND('',#11541,.T.);
#12661=FACE_BOUND('',#11542,.T.);
#12662=FACE_BOUND('',#11543,.T.);
#12663=(
BOUNDED_SURFACE()
B_SPLINE_SURFACE(1,2,((#19110,#19111,#19112,#19113,#19114,#19115,#19116,
#19117,#19118,#19119,#19120,#19121,#19122,#19123,#19124,#19125,#19126,#19127,
#19128,#19129,#19130,#19131,#19132,#19133,#19134,#19135,#19136,#19137,#19138,
#19139,#19140,#19141,#19142,#19143,#19144,#19145,#19146,#19147,#19148,#19149,
#19150,#19151,#19152,#19153,#19154,#19155,#19156,#19157,#19158,#19159,#19160,
#19161,#19162,#19163,#19164,#19165,#19166),(#19167,#19168,#19169,#19170,
#19171,#19172,#19173,#19174,#19175,#19176,#19177,#19178,#19179,#19180,#19181,
#19182,#19183,#19184,#19185,#19186,#19187,#19188,#19189,#19190,#19191,#19192,
#19193,#19194,#19195,#19196,#19197,#19198,#19199,#19200,#19201,#19202,#19203,
#19204,#19205,#19206,#19207,#19208,#19209,#19210,#19211,#19212,#19213,#19214,
#19215,#19216,#19217,#19218,#19219,#19220,#19221,#19222,#19223)),
 .RULED_SURF.,.F.,.F.,.F.)
B_SPLINE_SURFACE_WITH_KNOTS((2,2),(3,2,2,2,2,2,2,2,2,2,2,2,2,2,2,2,2,2,
2,2,2,2,2,2,2,2,2,2,3),(0.,1.),(0.,0.03125,0.0625,0.09375,0.125,0.15625,
0.1875,0.21875,0.25,0.28125,0.3125,0.34375,0.375,0.40625,0.4375,0.46875,
0.5,0.53125,0.5625,0.59375,0.625,0.65625,0.6875,0.71875,0.75,0.78125,0.8125,
0.84375,0.875),.UNSPECIFIED.)
GEOMETRIC_REPRESENTATION_ITEM()
RATIONAL_B_SPLINE_SURFACE(((1.,0.923879532511287,1.,0.923879532511287,1.,
0.923879532511287,1.,0.923879532511287,1.,0.923879532511287,1.,0.923879532511287,
1.,0.923879532511287,1.,0.923879532511287,1.,0.923879532511287,1.,0.923879532511287,
1.,0.923879532511287,1.,0.923879532511287,1.,0.923879532511287,1.,0.923879532511287,
1.,0.923879532511287,1.,0.923879532511287,1.,0.923879532511287,1.,0.923879532511287,
1.,0.923879532511287,1.,0.923879532511287,1.,0.923879532511287,1.,0.923879532511287,
1.,0.923879532511287,1.,0.923879532511287,1.,0.923879532511287,1.,0.923879532511287,
1.,0.923879532511287,1.,0.923879532511287,1.),(1.,0.923879532511287,1.,
0.923879532511287,1.,0.923879532511287,1.,0.923879532511287,1.,0.923879532511287,
1.,0.923879532511287,1.,0.923879532511287,1.,0.923879532511287,1.,0.923879532511287,
1.,0.923879532511287,1.,0.923879532511287,1.,0.923879532511287,1.,0.923879532511287,
1.,0.923879532511287,1.,0.923879532511287,1.,0.923879532511287,1.,0.923879532511287,
1.,0.923879532511287,1.,0.923879532511287,1.,0.923879532511287,1.,0.923879532511287,
1.,0.923879532511287,1.,0.923879532511287,1.,0.923879532511287,1.,0.923879532511287,
1.,0.923879532511287,1.,0.923879532511287,1.,0.923879532511287,1.)))
REPRESENTATION_ITEM('')
SURFACE()
);
#12664=(
BOUNDED_SURFACE()
B_SPLINE_SURFACE(1,2,((#19422,#19423,#19424,#19425,#19426,#19427,#19428,
#19429,#19430,#19431,#19432,#19433,#19434,#19435,#19436,#19437,#19438,#19439,
#19440,#19441,#19442,#19443,#19444,#19445,#19446,#19447,#19448,#19449,#19450,
#19451,#19452,#19453,#19454,#19455,#19456,#19457,#19458,#19459,#19460,#19461,
#19462,#19463,#19464,#19465,#19466,#19467,#19468,#19469,#19470,#19471,#19472,
#19473,#19474,#19475,#19476,#19477,#19478),(#19479,#19480,#19481,#19482,
#19483,#19484,#19485,#19486,#19487,#19488,#19489,#19490,#19491,#19492,#19493,
#19494,#19495,#19496,#19497,#19498,#19499,#19500,#19501,#19502,#19503,#19504,
#19505,#19506,#19507,#19508,#19509,#19510,#19511,#19512,#19513,#19514,#19515,
#19516,#19517,#19518,#19519,#19520,#19521,#19522,#19523,#19524,#19525,#19526,
#19527,#19528,#19529,#19530,#19531,#19532,#19533,#19534,#19535)),
 .RULED_SURF.,.F.,.F.,.F.)
B_SPLINE_SURFACE_WITH_KNOTS((2,2),(3,2,2,2,2,2,2,2,2,2,2,2,2,2,2,2,2,2,
2,2,2,2,2,2,2,2,2,2,3),(0.,1.),(0.,0.03125,0.0625,0.09375,0.125,0.15625,
0.1875,0.21875,0.25,0.28125,0.3125,0.34375,0.375,0.40625,0.4375,0.46875,
0.5,0.53125,0.5625,0.59375,0.625,0.65625,0.6875,0.71875,0.75,0.78125,0.8125,
0.84375,0.875),.UNSPECIFIED.)
GEOMETRIC_REPRESENTATION_ITEM()
RATIONAL_B_SPLINE_SURFACE(((1.,0.923879532511287,1.,0.923879532511287,1.,
0.923879532511287,1.,0.923879532511287,1.,0.923879532511287,1.,0.923879532511287,
1.,0.923879532511287,1.,0.923879532511287,1.,0.923879532511287,1.,0.923879532511287,
1.,0.923879532511287,1.,0.923879532511287,1.,0.923879532511287,1.,0.923879532511287,
1.,0.923879532511287,1.,0.923879532511287,1.,0.923879532511287,1.,0.923879532511287,
1.,0.923879532511287,1.,0.923879532511287,1.,0.923879532511287,1.,0.923879532511287,
1.,0.923879532511287,1.,0.923879532511287,1.,0.923879532511287,1.,0.923879532511287,
1.,0.923879532511287,1.,0.923879532511287,1.),(1.,0.923879532511287,1.,
0.923879532511287,1.,0.923879532511287,1.,0.923879532511287,1.,0.923879532511287,
1.,0.923879532511287,1.,0.923879532511287,1.,0.923879532511287,1.,0.923879532511287,
1.,0.923879532511287,1.,0.923879532511287,1.,0.923879532511287,1.,0.923879532511287,
1.,0.923879532511287,1.,0.923879532511287,1.,0.923879532511287,1.,0.923879532511287,
1.,0.923879532511287,1.,0.923879532511287,1.,0.923879532511287,1.,0.923879532511287,
1.,0.923879532511287,1.,0.923879532511287,1.,0.923879532511287,1.,0.923879532511287,
1.,0.923879532511287,1.,0.923879532511287,1.,0.923879532511287,1.)))
REPRESENTATION_ITEM('')
SURFACE()
);
#12665=(
BOUNDED_SURFACE()
B_SPLINE_SURFACE(3,3,((#19618,#19619,#19620,#19621),(#19622,#19623,#19624,
#19625),(#19626,#19627,#19628,#19629),(#19630,#19631,#19632,#19633)),
 .SURF_OF_REVOLUTION.,.F.,.F.,.F.)
B_SPLINE_SURFACE_WITH_KNOTS((4,4),(4,4),(0.,1.),(0.,1.),
 .PIECEWISE_BEZIER_KNOTS.)
GEOMETRIC_REPRESENTATION_ITEM()
RATIONAL_B_SPLINE_SURFACE(((1.,0.333333333333333,0.333333333333333,1.),
(1.,0.333333333333333,0.333333333333333,1.),(1.,0.333333333333333,0.333333333333333,
1.),(1.,0.333333333333333,0.333333333333333,1.)))
REPRESENTATION_ITEM('')
SURFACE()
);
#12666=(
BOUNDED_SURFACE()
B_SPLINE_SURFACE(3,3,((#19822,#19823,#19824,#19825),(#19826,#19827,#19828,
#19829),(#19830,#19831,#19832,#19833),(#19834,#19835,#19836,#19837)),
 .SURF_OF_REVOLUTION.,.F.,.F.,.F.)
B_SPLINE_SURFACE_WITH_KNOTS((4,4),(4,4),(0.,1.),(0.,1.),
 .PIECEWISE_BEZIER_KNOTS.)
GEOMETRIC_REPRESENTATION_ITEM()
RATIONAL_B_SPLINE_SURFACE(((1.,0.333333333333333,0.333333333333333,1.),
(1.,0.333333333333333,0.333333333333333,1.),(1.,0.333333333333333,0.333333333333333,
1.),(1.,0.333333333333333,0.333333333333333,1.)))
REPRESENTATION_ITEM('')
SURFACE()
);
#12667=(
BOUNDED_SURFACE()
B_SPLINE_SURFACE(1,2,((#19849,#19850,#19851,#19852,#19853,#19854,#19855,
#19856,#19857,#19858,#19859,#19860,#19861,#19862,#19863,#19864,#19865,#19866,
#19867,#19868,#19869,#19870,#19871,#19872,#19873,#19874,#19875,#19876,#19877,
#19878,#19879,#19880,#19881,#19882,#19883),(#19884,#19885,#19886,#19887,
#19888,#19889,#19890,#19891,#19892,#19893,#19894,#19895,#19896,#19897,#19898,
#19899,#19900,#19901,#19902,#19903,#19904,#19905,#19906,#19907,#19908,#19909,
#19910,#19911,#19912,#19913,#19914,#19915,#19916,#19917,#19918),(#19919,
#19920,#19921,#19922,#19923,#19924,#19925,#19926,#19927,#19928,#19929,#19930,
#19931,#19932,#19933,#19934,#19935,#19936,#19937,#19938,#19939,#19940,#19941,
#19942,#19943,#19944,#19945,#19946,#19947,#19948,#19949,#19950,#19951,#19952,
#19953)),.RULED_SURF.,.F.,.F.,.F.)
B_SPLINE_SURFACE_WITH_KNOTS((2,1,2),(3,2,2,2,2,2,2,2,2,2,2,2,2,2,2,2,2,
3),(0.,1.,1.08809896316278),(0.,0.05,0.1,0.15,0.2,0.25,0.3,0.35,0.4,0.45,
0.5,0.55,0.6,0.65,0.7,0.75,0.8,0.826757086852854),.UNSPECIFIED.)
GEOMETRIC_REPRESENTATION_ITEM()
RATIONAL_B_SPLINE_SURFACE(((1.,0.951056516295154,1.,0.951056516295154,1.,
0.951056516295154,1.,0.951056516295154,1.,0.951056516295154,1.,0.951056516295154,
1.,0.951056516295154,1.,0.951056516295154,1.,0.951056516295154,1.,0.951056516295154,
1.,0.951056516295154,1.,0.951056516295154,1.,0.951056516295154,1.,0.951056516295154,
1.,0.951056516295154,1.,0.951056516295154,1.,0.973808299112564,0.975649142843891),
(1.,0.951056516295154,1.,0.951056516295154,1.,0.951056516295154,1.,0.951056516295154,
1.,0.951056516295154,1.,0.951056516295154,1.,0.951056516295154,1.,0.951056516295154,
1.,0.951056516295154,1.,0.951056516295154,1.,0.951056516295154,1.,0.951056516295154,
1.,0.951056516295154,1.,0.951056516295154,1.,0.951056516295154,1.,0.951056516295154,
1.,0.973808299112564,0.975649142843891),(1.,0.951056516295154,1.,0.951056516295154,
1.,0.951056516295154,1.,0.951056516295154,1.,0.951056516295154,1.,0.951056516295154,
1.,0.951056516295154,1.,0.951056516295154,1.,0.951056516295154,1.,0.951056516295154,
1.,0.951056516295154,1.,0.951056516295154,1.,0.951056516295154,1.,0.951056516295154,
1.,0.951056516295154,1.,0.951056516295154,1.,0.973808299112564,0.975649142843891)))
REPRESENTATION_ITEM('')
SURFACE()
);
#12668=(
BOUNDED_SURFACE()
B_SPLINE_SURFACE(3,2,((#27051,#27052,#27053,#27054,#27055,#27056,#27057,
#27058,#27059,#27060,#27061,#27062,#27063,#27064,#27065,#27066,#27067,#27068,
#27069,#27070,#27071,#27072,#27073,#27074,#27075,#27076,#27077,#27078,#27079,
#27080,#27081,#27082,#27083,#27084,#27085,#27086,#27087,#27088,#27089,#27090,
#27091,#27092,#27093,#27094,#27095),(#27096,#27097,#27098,#27099,#27100,
#27101,#27102,#27103,#27104,#27105,#27106,#27107,#27108,#27109,#27110,#27111,
#27112,#27113,#27114,#27115,#27116,#27117,#27118,#27119,#27120,#27121,#27122,
#27123,#27124,#27125,#27126,#27127,#27128,#27129,#27130,#27131,#27132,#27133,
#27134,#27135,#27136,#27137,#27138,#27139,#27140),(#27141,#27142,#27143,
#27144,#27145,#27146,#27147,#27148,#27149,#27150,#27151,#27152,#27153,#27154,
#27155,#27156,#27157,#27158,#27159,#27160,#27161,#27162,#27163,#27164,#27165,
#27166,#27167,#27168,#27169,#27170,#27171,#27172,#27173,#27174,#27175,#27176,
#27177,#27178,#27179,#27180,#27181,#27182,#27183,#27184,#27185),(#27186,
#27187,#27188,#27189,#27190,#27191,#27192,#27193,#27194,#27195,#27196,#27197,
#27198,#27199,#27200,#27201,#27202,#27203,#27204,#27205,#27206,#27207,#27208,
#27209,#27210,#27211,#27212,#27213,#27214,#27215,#27216,#27217,#27218,#27219,
#27220,#27221,#27222,#27223,#27224,#27225,#27226,#27227,#27228,#27229,#27230)),
 .UNSPECIFIED.,.F.,.F.,.F.)
B_SPLINE_SURFACE_WITH_KNOTS((4,4),(3,2,2,2,2,2,2,2,2,2,2,2,2,2,2,2,2,2,
2,2,2,2,3),(0.,1.),(0.249847948106021,0.25,0.277777777777778,0.305555555555555,
0.333333333333334,0.361111111111111,0.388888888888889,0.416666666666667,
0.444444444444444,0.472222222222222,0.5,0.527777777777778,0.555555555555556,
0.583333333333333,0.611111111111111,0.638888888888889,0.666666666666667,
0.694444444444444,0.722222222222222,0.75,0.777777777777778,0.805555555555556,
0.833333333333333),.PIECEWISE_BEZIER_KNOTS.)
GEOMETRIC_REPRESENTATION_ITEM()
RATIONAL_B_SPLINE_SURFACE(((0.99962900687411,0.999813482464653,1.,0.965925826289068,
1.,0.965925826289068,1.,0.965925826289068,1.,0.965925826289068,1.,0.965925826289068,
1.,0.965925826289068,1.,0.965925826289068,1.,0.965925826289068,1.,0.965925826289068,
1.,0.965925826289068,1.,0.965925826289068,1.,0.965925826289068,1.,0.965925826289068,
1.,0.965925826289068,1.,0.965925826289068,1.,0.965925826289068,1.,0.965925826289068,
1.,0.965925826289068,1.,0.965925826289068,1.,0.965925826289068,1.,0.965925826289068,
1.),(0.843716499555672,0.84387220241987,0.844029628745984,0.81527001655892,
0.844029628745984,0.81527001655892,0.844029628745984,0.81527001655892,0.844029628745984,
0.81527001655892,0.844029628745984,0.81527001655892,0.844029628745984,0.81527001655892,
0.844029628745984,0.81527001655892,0.844029628745984,0.81527001655892,0.844029628745984,
0.81527001655892,0.844029628745984,0.81527001655892,0.844029628745984,0.81527001655892,
0.844029628745984,0.81527001655892,0.844029628745984,0.81527001655892,0.844029628745984,
0.81527001655892,0.844029628745984,0.81527001655892,0.844029628745984,0.81527001655892,
0.844029628745984,0.81527001655892,0.844029628745984,0.81527001655892,0.844029628745984,
0.81527001655892,0.844029628745984,0.81527001655892,0.844029628745984,0.81527001655892,
0.844029628745984),(0.843716499555672,0.84387220241987,0.844029628745984,
0.81527001655892,0.844029628745984,0.81527001655892,0.844029628745984,0.81527001655892,
0.844029628745984,0.81527001655892,0.844029628745984,0.81527001655892,0.844029628745984,
0.81527001655892,0.844029628745984,0.81527001655892,0.844029628745984,0.81527001655892,
0.844029628745984,0.81527001655892,0.844029628745984,0.81527001655892,0.844029628745984,
0.81527001655892,0.844029628745984,0.81527001655892,0.844029628745984,0.81527001655892,
0.844029628745984,0.81527001655892,0.844029628745984,0.81527001655892,0.844029628745984,
0.81527001655892,0.844029628745984,0.81527001655892,0.844029628745984,0.81527001655892,
0.844029628745984,0.81527001655892,0.844029628745984,0.81527001655892,0.844029628745984,
0.81527001655892,0.844029628745984),(0.99962900687411,0.999813482464653,
1.,0.965925826289068,1.,0.965925826289068,1.,0.965925826289068,1.,0.965925826289068,
1.,0.965925826289068,1.,0.965925826289068,1.,0.965925826289068,1.,0.965925826289068,
1.,0.965925826289068,1.,0.965925826289068,1.,0.965925826289068,1.,0.965925826289068,
1.,0.965925826289068,1.,0.965925826289068,1.,0.965925826289068,1.,0.965925826289068,
1.,0.965925826289068,1.,0.965925826289068,1.,0.965925826289068,1.,0.965925826289068,
1.,0.965925826289068,1.)))
REPRESENTATION_ITEM('')
SURFACE()
);
#12669=(
BOUNDED_SURFACE()
B_SPLINE_SURFACE(1,2,((#27334,#27335,#27336,#27337,#27338,#27339,#27340,
#27341,#27342,#27343,#27344,#27345,#27346,#27347,#27348,#27349,#27350,#27351,
#27352,#27353,#27354,#27355,#27356,#27357,#27358,#27359,#27360,#27361,#27362,
#27363,#27364,#27365,#27366,#27367,#27368,#27369,#27370,#27371,#27372,#27373,
#27374,#27375,#27376,#27377,#27378),(#27379,#27380,#27381,#27382,#27383,
#27384,#27385,#27386,#27387,#27388,#27389,#27390,#27391,#27392,#27393,#27394,
#27395,#27396,#27397,#27398,#27399,#27400,#27401,#27402,#27403,#27404,#27405,
#27406,#27407,#27408,#27409,#27410,#27411,#27412,#27413,#27414,#27415,#27416,
#27417,#27418,#27419,#27420,#27421,#27422,#27423)),.RULED_SURF.,.F.,.F.,
 .F.)
B_SPLINE_SURFACE_WITH_KNOTS((2,2),(3,2,2,2,2,2,2,2,2,2,2,2,2,2,2,2,2,2,
2,2,2,2,3),(0.,1.),(0.23764503803818,0.25,0.277777777777778,0.305555555555555,
0.333333333333334,0.361111111111111,0.388888888888889,0.416666666666667,
0.444444444444444,0.472222222222222,0.5,0.527777777777778,0.555555555555556,
0.583333333333333,0.611111111111111,0.638888888888889,0.666666666666667,
0.694444444444444,0.722222222222222,0.75,0.777777777777778,0.805555555555556,
0.833333333333333),.PIECEWISE_BEZIER_KNOTS.)
GEOMETRIC_REPRESENTATION_ITEM()
RATIONAL_B_SPLINE_SURFACE(((0.983170724690329,0.984844535677156,1.,0.965925826289068,
1.,0.965925826289068,1.,0.965925826289068,1.,0.965925826289068,1.,0.965925826289068,
1.,0.965925826289068,1.,0.965925826289068,1.,0.965925826289068,1.,0.965925826289068,
1.,0.965925826289068,1.,0.965925826289068,1.,0.965925826289068,1.,0.965925826289068,
1.,0.965925826289068,1.,0.965925826289068,1.,0.965925826289068,1.,0.965925826289068,
1.,0.965925826289068,1.,0.965925826289068,1.,0.965925826289068,1.,0.965925826289068,
1.),(0.983170724690329,0.984844535677156,1.,0.965925826289068,1.,0.965925826289068,
1.,0.965925826289068,1.,0.965925826289068,1.,0.965925826289068,1.,0.965925826289068,
1.,0.965925826289068,1.,0.965925826289068,1.,0.965925826289068,1.,0.965925826289068,
1.,0.965925826289068,1.,0.965925826289068,1.,0.965925826289068,1.,0.965925826289068,
1.,0.965925826289068,1.,0.965925826289068,1.,0.965925826289068,1.,0.965925826289068,
1.,0.965925826289068,1.,0.965925826289068,1.,0.965925826289068,1.)))
REPRESENTATION_ITEM('')
SURFACE()
);
#12670=(
BOUNDED_SURFACE()
B_SPLINE_SURFACE(3,2,((#27476,#27477,#27478,#27479,#27480,#27481,#27482,
#27483,#27484,#27485,#27486,#27487,#27488,#27489,#27490,#27491,#27492,#27493,
#27494,#27495,#27496,#27497,#27498,#27499,#27500,#27501,#27502,#27503,#27504,
#27505,#27506,#27507,#27508,#27509,#27510,#27511,#27512,#27513,#27514,#27515,
#27516,#27517,#27518,#27519,#27520,#27521,#27522),(#27523,#27524,#27525,
#27526,#27527,#27528,#27529,#27530,#27531,#27532,#27533,#27534,#27535,#27536,
#27537,#27538,#27539,#27540,#27541,#27542,#27543,#27544,#27545,#27546,#27547,
#27548,#27549,#27550,#27551,#27552,#27553,#27554,#27555,#27556,#27557,#27558,
#27559,#27560,#27561,#27562,#27563,#27564,#27565,#27566,#27567,#27568,#27569),
(#27570,#27571,#27572,#27573,#27574,#27575,#27576,#27577,#27578,#27579,
#27580,#27581,#27582,#27583,#27584,#27585,#27586,#27587,#27588,#27589,#27590,
#27591,#27592,#27593,#27594,#27595,#27596,#27597,#27598,#27599,#27600,#27601,
#27602,#27603,#27604,#27605,#27606,#27607,#27608,#27609,#27610,#27611,#27612,
#27613,#27614,#27615,#27616),(#27617,#27618,#27619,#27620,#27621,#27622,
#27623,#27624,#27625,#27626,#27627,#27628,#27629,#27630,#27631,#27632,#27633,
#27634,#27635,#27636,#27637,#27638,#27639,#27640,#27641,#27642,#27643,#27644,
#27645,#27646,#27647,#27648,#27649,#27650,#27651,#27652,#27653,#27654,#27655,
#27656,#27657,#27658,#27659,#27660,#27661,#27662,#27663)),.UNSPECIFIED.,
 .F.,.F.,.F.)
B_SPLINE_SURFACE_WITH_KNOTS((4,4),(3,2,2,2,2,2,2,2,2,2,2,2,2,2,2,2,2,2,
2,2,2,2,2,3),(0.,1.),(0.211213851681445,0.222222222222222,0.25,0.277777777777778,
0.305555555555555,0.333333333333334,0.361111111111111,0.388888888888889,
0.416666666666667,0.444444444444444,0.472222222222222,0.5,0.527777777777778,
0.555555555555556,0.583333333333333,0.611111111111111,0.638888888888889,
0.666666666666667,0.694444444444444,0.722222222222222,0.75,0.777777777777778,
0.805555555555556,0.833333333333333),.PIECEWISE_BEZIER_KNOTS.)
GEOMETRIC_REPRESENTATION_ITEM()
RATIONAL_B_SPLINE_SURFACE(((0.983695740414847,0.986496359317093,1.,0.965925826289068,
1.,0.965925826289068,1.,0.965925826289068,1.,0.965925826289068,1.,0.965925826289068,
1.,0.965925826289068,1.,0.965925826289068,1.,0.965925826289068,1.,0.965925826289068,
1.,0.965925826289068,1.,0.965925826289068,1.,0.965925826289068,1.,0.965925826289068,
1.,0.965925826289068,1.,0.965925826289068,1.,0.965925826289068,1.,0.965925826289068,
1.,0.965925826289068,1.,0.965925826289068,1.,0.965925826289068,1.,0.965925826289068,
1.,0.965925826289068,1.),(0.830268350581347,0.832632155913669,0.844029628745982,
0.815270016558918,0.844029628745982,0.815270016558918,0.844029628745982,
0.815270016558918,0.844029628745982,0.815270016558918,0.844029628745982,
0.815270016558918,0.844029628745982,0.815270016558918,0.844029628745982,
0.815270016558918,0.844029628745982,0.815270016558918,0.844029628745982,
0.815270016558918,0.844029628745982,0.815270016558918,0.844029628745982,
0.815270016558918,0.844029628745982,0.815270016558918,0.844029628745982,
0.815270016558918,0.844029628745982,0.815270016558918,0.844029628745982,
0.815270016558918,0.844029628745982,0.815270016558918,0.844029628745982,
0.815270016558918,0.844029628745982,0.815270016558918,0.844029628745982,
0.815270016558918,0.844029628745982,0.815270016558918,0.844029628745982,
0.815270016558918,0.844029628745982,0.815270016558918,0.844029628745982),
(0.830268350581347,0.832632155913669,0.844029628745982,0.815270016558918,
0.844029628745982,0.815270016558918,0.844029628745982,0.815270016558918,
0.844029628745982,0.815270016558918,0.844029628745982,0.815270016558918,
0.844029628745982,0.815270016558918,0.844029628745982,0.815270016558918,
0.844029628745982,0.815270016558918,0.844029628745982,0.815270016558918,
0.844029628745982,0.815270016558918,0.844029628745982,0.815270016558918,
0.844029628745982,0.815270016558918,0.844029628745982,0.815270016558918,
0.844029628745982,0.815270016558918,0.844029628745982,0.815270016558918,
0.844029628745982,0.815270016558918,0.844029628745982,0.815270016558918,
0.844029628745982,0.815270016558918,0.844029628745982,0.815270016558918,
0.844029628745982,0.815270016558918,0.844029628745982,0.815270016558918,
0.844029628745982,0.815270016558918,0.844029628745982),(0.983695740414847,
0.986496359317093,1.,0.965925826289068,1.,0.965925826289068,1.,0.965925826289068,
1.,0.965925826289068,1.,0.965925826289068,1.,0.965925826289068,1.,0.965925826289068,
1.,0.965925826289068,1.,0.965925826289068,1.,0.965925826289068,1.,0.965925826289068,
1.,0.965925826289068,1.,0.965925826289068,1.,0.965925826289068,1.,0.965925826289068,
1.,0.965925826289068,1.,0.965925826289068,1.,0.965925826289068,1.,0.965925826289068,
1.,0.965925826289068,1.,0.965925826289068,1.,0.965925826289068,1.)))
REPRESENTATION_ITEM('')
SURFACE()
);
#12671=(
BOUNDED_SURFACE()
B_SPLINE_SURFACE(3,2,((#27776,#27777,#27778,#27779,#27780,#27781,#27782,
#27783,#27784,#27785,#27786,#27787,#27788,#27789,#27790,#27791,#27792,#27793,
#27794,#27795,#27796,#27797,#27798,#27799,#27800,#27801,#27802,#27803,#27804,
#27805,#27806,#27807,#27808,#27809,#27810,#27811,#27812,#27813,#27814,#27815,
#27816,#27817,#27818,#27819,#27820,#27821,#27822,#27823,#27824,#27825,#27826,
#27827,#27828),(#27829,#27830,#27831,#27832,#27833,#27834,#27835,#27836,
#27837,#27838,#27839,#27840,#27841,#27842,#27843,#27844,#27845,#27846,#27847,
#27848,#27849,#27850,#27851,#27852,#27853,#27854,#27855,#27856,#27857,#27858,
#27859,#27860,#27861,#27862,#27863,#27864,#27865,#27866,#27867,#27868,#27869,
#27870,#27871,#27872,#27873,#27874,#27875,#27876,#27877,#27878,#27879,#27880,
#27881),(#27882,#27883,#27884,#27885,#27886,#27887,#27888,#27889,#27890,
#27891,#27892,#27893,#27894,#27895,#27896,#27897,#27898,#27899,#27900,#27901,
#27902,#27903,#27904,#27905,#27906,#27907,#27908,#27909,#27910,#27911,#27912,
#27913,#27914,#27915,#27916,#27917,#27918,#27919,#27920,#27921,#27922,#27923,
#27924,#27925,#27926,#27927,#27928,#27929,#27930,#27931,#27932,#27933,#27934),
(#27935,#27936,#27937,#27938,#27939,#27940,#27941,#27942,#27943,#27944,
#27945,#27946,#27947,#27948,#27949,#27950,#27951,#27952,#27953,#27954,#27955,
#27956,#27957,#27958,#27959,#27960,#27961,#27962,#27963,#27964,#27965,#27966,
#27967,#27968,#27969,#27970,#27971,#27972,#27973,#27974,#27975,#27976,#27977,
#27978,#27979,#27980,#27981,#27982,#27983,#27984,#27985,#27986,#27987)),
 .UNSPECIFIED.,.F.,.F.,.F.)
B_SPLINE_SURFACE_WITH_KNOTS((4,4),(3,2,2,2,2,2,2,2,2,2,2,2,2,2,2,2,2,2,
2,2,2,2,2,2,2,2,3),(0.,1.),(0.117489249341577,0.138888888888889,0.166666666666667,
0.194444444444445,0.222222222222222,0.25,0.277777777777778,0.305555555555555,
0.333333333333334,0.361111111111111,0.388888888888889,0.416666666666667,
0.444444444444444,0.472222222222222,0.5,0.527777777777778,0.555555555555556,
0.583333333333333,0.611111111111111,0.638888888888889,0.666666666666667,
0.694444444444444,0.722222222222222,0.75,0.777777777777778,0.805555555555556,
0.833333333333333),.PIECEWISE_BEZIER_KNOTS.)
GEOMETRIC_REPRESENTATION_ITEM()
RATIONAL_B_SPLINE_SURFACE(((0.987945180393274,0.973749698729688,1.,0.965925826289068,
1.,0.965925826289068,1.,0.965925826289068,1.,0.965925826289068,1.,0.965925826289068,
1.,0.965925826289068,1.,0.965925826289068,1.,0.965925826289068,1.,0.965925826289068,
1.,0.965925826289068,1.,0.965925826289068,1.,0.965925826289068,1.,0.965925826289068,
1.,0.965925826289068,1.,0.965925826289068,1.,0.965925826289068,1.,0.965925826289068,
1.,0.965925826289068,1.,0.965925826289068,1.,0.965925826289068,1.,0.965925826289068,
1.,0.965925826289068,1.,0.965925826289068,1.,0.965925826289068,1.,0.965925826289068,
1.),(0.937809947736769,0.92433484387349,0.949253021674191,0.916908009318038,
0.949253021674191,0.916908009318038,0.949253021674191,0.916908009318038,
0.949253021674191,0.916908009318038,0.949253021674191,0.916908009318038,
0.949253021674191,0.916908009318038,0.949253021674191,0.916908009318038,
0.949253021674191,0.916908009318038,0.949253021674191,0.916908009318038,
0.949253021674191,0.916908009318038,0.949253021674191,0.916908009318038,
0.949253021674191,0.916908009318038,0.949253021674191,0.916908009318038,
0.949253021674191,0.916908009318038,0.949253021674191,0.916908009318038,
0.949253021674191,0.916908009318038,0.949253021674191,0.916908009318038,
0.949253021674191,0.916908009318038,0.949253021674191,0.916908009318038,
0.949253021674191,0.916908009318038,0.949253021674191,0.916908009318038,
0.949253021674191,0.916908009318038,0.949253021674191,0.916908009318038,
0.949253021674191,0.916908009318038,0.949253021674191,0.916908009318038,
0.949253021674191),(0.937809947736769,0.92433484387349,0.949253021674191,
0.916908009318038,0.949253021674191,0.916908009318038,0.949253021674191,
0.916908009318038,0.949253021674191,0.916908009318038,0.949253021674191,
0.916908009318038,0.949253021674191,0.916908009318038,0.949253021674191,
0.916908009318038,0.949253021674191,0.916908009318038,0.949253021674191,
0.916908009318038,0.949253021674191,0.916908009318038,0.949253021674191,
0.916908009318038,0.949253021674191,0.916908009318038,0.949253021674191,
0.916908009318038,0.949253021674191,0.916908009318038,0.949253021674191,
0.916908009318038,0.949253021674191,0.916908009318038,0.949253021674191,
0.916908009318038,0.949253021674191,0.916908009318038,0.949253021674191,
0.916908009318038,0.949253021674191,0.916908009318038,0.949253021674191,
0.916908009318038,0.949253021674191,0.916908009318038,0.949253021674191,
0.916908009318038,0.949253021674191,0.916908009318038,0.949253021674191,
0.916908009318038,0.949253021674191),(0.987945180393274,0.973749698729688,
1.,0.965925826289068,1.,0.965925826289068,1.,0.965925826289068,1.,0.965925826289068,
1.,0.965925826289068,1.,0.965925826289068,1.,0.965925826289068,1.,0.965925826289068,
1.,0.965925826289068,1.,0.965925826289068,1.,0.965925826289068,1.,0.965925826289068,
1.,0.965925826289068,1.,0.965925826289068,1.,0.965925826289068,1.,0.965925826289068,
1.,0.965925826289068,1.,0.965925826289068,1.,0.965925826289068,1.,0.965925826289068,
1.,0.965925826289068,1.,0.965925826289068,1.,0.965925826289068,1.,0.965925826289068,
1.,0.965925826289068,1.)))
REPRESENTATION_ITEM('')
SURFACE()
);
#12672=(
BOUNDED_SURFACE()
B_SPLINE_SURFACE(1,2,((#28050,#28051,#28052,#28053,#28054,#28055,#28056,
#28057,#28058,#28059,#28060,#28061,#28062,#28063,#28064,#28065,#28066,#28067,
#28068,#28069,#28070,#28071,#28072,#28073,#28074,#28075,#28076,#28077,#28078,
#28079,#28080,#28081,#28082,#28083,#28084,#28085,#28086,#28087,#28088,#28089,
#28090,#28091,#28092,#28093,#28094,#28095,#28096,#28097,#28098,#28099,#28100,
#28101,#28102,#28103,#28104,#28105,#28106,#28107,#28108),(#28109,#28110,
#28111,#28112,#28113,#28114,#28115,#28116,#28117,#28118,#28119,#28120,#28121,
#28122,#28123,#28124,#28125,#28126,#28127,#28128,#28129,#28130,#28131,#28132,
#28133,#28134,#28135,#28136,#28137,#28138,#28139,#28140,#28141,#28142,#28143,
#28144,#28145,#28146,#28147,#28148,#28149,#28150,#28151,#28152,#28153,#28154,
#28155,#28156,#28157,#28158,#28159,#28160,#28161,#28162,#28163,#28164,#28165,
#28166,#28167)),.RULED_SURF.,.F.,.F.,.F.)
B_SPLINE_SURFACE_WITH_KNOTS((2,2),(3,2,2,2,2,2,2,2,2,2,2,2,2,2,2,2,2,2,
2,2,2,2,2,2,2,2,2,2,2,3),(0.,1.),(0.051939905583397,0.0555555555555556,
0.0833333333333333,0.111111111111111,0.138888888888889,0.166666666666667,
0.194444444444445,0.222222222222222,0.25,0.277777777777778,0.305555555555555,
0.333333333333334,0.361111111111111,0.388888888888889,0.416666666666667,
0.444444444444444,0.472222222222222,0.5,0.527777777777778,0.555555555555556,
0.583333333333333,0.611111111111111,0.638888888888889,0.666666666666667,
0.694444444444444,0.722222222222222,0.75,0.777777777777778,0.805555555555556,
0.833333333333333),.PIECEWISE_BEZIER_KNOTS.)
GEOMETRIC_REPRESENTATION_ITEM()
RATIONAL_B_SPLINE_SURFACE(((0.992284183551064,0.995564789731747,1.,0.965925826289068,
1.,0.965925826289068,1.,0.965925826289068,1.,0.965925826289068,1.,0.965925826289068,
1.,0.965925826289068,1.,0.965925826289068,1.,0.965925826289068,1.,0.965925826289068,
1.,0.965925826289068,1.,0.965925826289068,1.,0.965925826289068,1.,0.965925826289068,
1.,0.965925826289068,1.,0.965925826289068,1.,0.965925826289068,1.,0.965925826289068,
1.,0.965925826289068,1.,0.965925826289068,1.,0.965925826289068,1.,0.965925826289068,
1.,0.965925826289068,1.,0.965925826289068,1.,0.965925826289068,1.,0.965925826289068,
1.,0.965925826289068,1.,0.965925826289068,1.,0.965925826289068,1.),(0.992284183551064,
0.995564789731747,1.,0.965925826289068,1.,0.965925826289068,1.,0.965925826289068,
1.,0.965925826289068,1.,0.965925826289068,1.,0.965925826289068,1.,0.965925826289068,
1.,0.965925826289068,1.,0.965925826289068,1.,0.965925826289068,1.,0.965925826289068,
1.,0.965925826289068,1.,0.965925826289068,1.,0.965925826289068,1.,0.965925826289068,
1.,0.965925826289068,1.,0.965925826289068,1.,0.965925826289068,1.,0.965925826289068,
1.,0.965925826289068,1.,0.965925826289068,1.,0.965925826289068,1.,0.965925826289068,
1.,0.965925826289068,1.,0.965925826289068,1.,0.965925826289068,1.,0.965925826289068,
1.,0.965925826289068,1.)))
REPRESENTATION_ITEM('')
SURFACE()
);
#12673=(
BOUNDED_SURFACE()
B_SPLINE_SURFACE(3,2,((#28234,#28235,#28236,#28237,#28238,#28239,#28240,
#28241,#28242,#28243,#28244,#28245,#28246,#28247,#28248,#28249,#28250,#28251,
#28252,#28253,#28254,#28255,#28256,#28257,#28258,#28259,#28260,#28261,#28262,
#28263,#28264,#28265,#28266,#28267,#28268,#28269,#28270,#28271,#28272,#28273,
#28274,#28275,#28276,#28277,#28278,#28279,#28280,#28281,#28282,#28283,#28284,
#28285,#28286,#28287,#28288,#28289,#28290,#28291,#28292,#28293,#28294),
(#28295,#28296,#28297,#28298,#28299,#28300,#28301,#28302,#28303,#28304,
#28305,#28306,#28307,#28308,#28309,#28310,#28311,#28312,#28313,#28314,#28315,
#28316,#28317,#28318,#28319,#28320,#28321,#28322,#28323,#28324,#28325,#28326,
#28327,#28328,#28329,#28330,#28331,#28332,#28333,#28334,#28335,#28336,#28337,
#28338,#28339,#28340,#28341,#28342,#28343,#28344,#28345,#28346,#28347,#28348,
#28349,#28350,#28351,#28352,#28353,#28354,#28355),(#28356,#28357,#28358,
#28359,#28360,#28361,#28362,#28363,#28364,#28365,#28366,#28367,#28368,#28369,
#28370,#28371,#28372,#28373,#28374,#28375,#28376,#28377,#28378,#28379,#28380,
#28381,#28382,#28383,#28384,#28385,#28386,#28387,#28388,#28389,#28390,#28391,
#28392,#28393,#28394,#28395,#28396,#28397,#28398,#28399,#28400,#28401,#28402,
#28403,#28404,#28405,#28406,#28407,#28408,#28409,#28410,#28411,#28412,#28413,
#28414,#28415,#28416),(#28417,#28418,#28419,#28420,#28421,#28422,#28423,
#28424,#28425,#28426,#28427,#28428,#28429,#28430,#28431,#28432,#28433,#28434,
#28435,#28436,#28437,#28438,#28439,#28440,#28441,#28442,#28443,#28444,#28445,
#28446,#28447,#28448,#28449,#28450,#28451,#28452,#28453,#28454,#28455,#28456,
#28457,#28458,#28459,#28460,#28461,#28462,#28463,#28464,#28465,#28466,#28467,
#28468,#28469,#28470,#28471,#28472,#28473,#28474,#28475,#28476,#28477)),
 .UNSPECIFIED.,.F.,.F.,.F.)
B_SPLINE_SURFACE_WITH_KNOTS((4,4),(3,2,2,2,2,2,2,2,2,2,2,2,2,2,2,2,2,2,
2,2,2,2,2,2,2,2,2,2,2,2,3),(0.,1.),(0.,0.0277777777777778,0.0555555555555556,
0.0833333333333333,0.111111111111111,0.138888888888889,0.166666666666667,
0.194444444444445,0.222222222222222,0.25,0.277777777777778,0.305555555555555,
0.333333333333334,0.361111111111111,0.388888888888889,0.416666666666667,
0.444444444444444,0.472222222222222,0.5,0.527777777777778,0.555555555555556,
0.583333333333333,0.611111111111111,0.638888888888889,0.666666666666667,
0.694444444444444,0.722222222222222,0.75,0.777777777777778,0.805555555555556,
0.833333333333333),.PIECEWISE_BEZIER_KNOTS.)
GEOMETRIC_REPRESENTATION_ITEM()
RATIONAL_B_SPLINE_SURFACE(((1.,0.965925826289068,1.,0.965925826289068,1.,
0.965925826289068,1.,0.965925826289068,1.,0.965925826289068,1.,0.965925826289068,
1.,0.965925826289068,1.,0.965925826289068,1.,0.965925826289068,1.,0.965925826289068,
1.,0.965925826289068,1.,0.965925826289068,1.,0.965925826289068,1.,0.965925826289068,
1.,0.965925826289068,1.,0.965925826289068,1.,0.965925826289068,1.,0.965925826289068,
1.,0.965925826289068,1.,0.965925826289068,1.,0.965925826289068,1.,0.965925826289068,
1.,0.965925826289068,1.,0.965925826289068,1.,0.965925826289068,1.,0.965925826289068,
1.,0.965925826289068,1.,0.965925826289068,1.,0.965925826289068,1.,0.965925826289068,
1.),(0.949253021674191,0.916908009318038,0.949253021674191,0.916908009318038,
0.949253021674191,0.916908009318038,0.949253021674191,0.916908009318038,
0.949253021674191,0.916908009318038,0.949253021674191,0.916908009318038,
0.949253021674191,0.916908009318038,0.949253021674191,0.916908009318038,
0.949253021674191,0.916908009318038,0.949253021674191,0.916908009318038,
0.949253021674191,0.916908009318038,0.949253021674191,0.916908009318038,
0.949253021674191,0.916908009318038,0.949253021674191,0.916908009318038,
0.949253021674191,0.916908009318038,0.949253021674191,0.916908009318038,
0.949253021674191,0.916908009318038,0.949253021674191,0.916908009318038,
0.949253021674191,0.916908009318038,0.949253021674191,0.916908009318038,
0.949253021674191,0.916908009318038,0.949253021674191,0.916908009318038,
0.949253021674191,0.916908009318038,0.949253021674191,0.916908009318038,
0.949253021674191,0.916908009318038,0.949253021674191,0.916908009318038,
0.949253021674191,0.916908009318038,0.949253021674191,0.916908009318038,
0.949253021674191,0.916908009318038,0.949253021674191,0.916908009318038,
0.949253021674191),(0.949253021674191,0.916908009318038,0.949253021674191,
0.916908009318038,0.949253021674191,0.916908009318038,0.949253021674191,
0.916908009318038,0.949253021674191,0.916908009318038,0.949253021674191,
0.916908009318038,0.949253021674191,0.916908009318038,0.949253021674191,
0.916908009318038,0.949253021674191,0.916908009318038,0.949253021674191,
0.916908009318038,0.949253021674191,0.916908009318038,0.949253021674191,
0.916908009318038,0.949253021674191,0.916908009318038,0.949253021674191,
0.916908009318038,0.949253021674191,0.916908009318038,0.949253021674191,
0.916908009318038,0.949253021674191,0.916908009318038,0.949253021674191,
0.916908009318038,0.949253021674191,0.916908009318038,0.949253021674191,
0.916908009318038,0.949253021674191,0.916908009318038,0.949253021674191,
0.916908009318038,0.949253021674191,0.916908009318038,0.949253021674191,
0.916908009318038,0.949253021674191,0.916908009318038,0.949253021674191,
0.916908009318038,0.949253021674191,0.916908009318038,0.949253021674191,
0.916908009318038,0.949253021674191,0.916908009318038,0.949253021674191,
0.916908009318038,0.949253021674191),(1.,0.965925826289068,1.,0.965925826289068,
1.,0.965925826289068,1.,0.965925826289068,1.,0.965925826289068,1.,0.965925826289068,
1.,0.965925826289068,1.,0.965925826289068,1.,0.965925826289068,1.,0.965925826289068,
1.,0.965925826289068,1.,0.965925826289068,1.,0.965925826289068,1.,0.965925826289068,
1.,0.965925826289068,1.,0.965925826289068,1.,0.965925826289068,1.,0.965925826289068,
1.,0.965925826289068,1.,0.965925826289068,1.,0.965925826289068,1.,0.965925826289068,
1.,0.965925826289068,1.,0.965925826289068,1.,0.965925826289068,1.,0.965925826289068,
1.,0.965925826289068,1.,0.965925826289068,1.,0.965925826289068,1.,0.965925826289068,
1.)))
REPRESENTATION_ITEM('')
SURFACE()
);
#12674=(
BOUNDED_SURFACE()
B_SPLINE_SURFACE(3,3,((#28570,#28571,#28572,#28573,#28574,#28575,#28576,
#28577,#28578,#28579,#28580,#28581,#28582,#28583,#28584,#28585,#28586,#28587,
#28588,#28589,#28590,#28591,#28592,#28593,#28594,#28595,#28596,#28597,#28598,
#28599,#28600,#28601,#28602,#28603,#28604,#28605,#28606,#28607,#28608,#28609,
#28610,#28611,#28612,#28613,#28614,#28615,#28616,#28617,#28618,#28619,#28620,
#28621,#28622,#28623,#28624,#28625,#28626,#28627,#28628,#28629,#28630,#28631,
#28632,#28633,#28634,#28635,#28636,#28637,#28638,#28639,#28640,#28641,#28642,
#28643,#28644,#28645,#28646,#28647,#28648,#28649,#28650,#28651,#28652,#28653,
#28654,#28655,#28656,#28657,#28658,#28659,#28660,#28661,#28662,#28663,#28664,
#28665,#28666,#28667,#28668,#28669,#28670,#28671,#28672,#28673,#28674,#28675,
#28676,#28677,#28678,#28679,#28680,#28681,#28682,#28683,#28684,#28685,#28686,
#28687,#28688,#28689,#28690,#28691,#28692,#28693,#28694,#28695,#28696,#28697,
#28698,#28699,#28700,#28701,#28702,#28703,#28704,#28705,#28706,#28707,#28708,
#28709,#28710,#28711,#28712,#28713,#28714,#28715,#28716,#28717,#28718,#28719,
#28720,#28721,#28722,#28723,#28724,#28725,#28726,#28727,#28728,#28729,#28730,
#28731,#28732,#28733,#28734,#28735,#28736,#28737,#28738,#28739,#28740,#28741,
#28742,#28743,#28744,#28745,#28746,#28747,#28748,#28749,#28750,#28751,#28752,
#28753,#28754,#28755,#28756,#28757,#28758,#28759,#28760,#28761,#28762,#28763,
#28764,#28765,#28766,#28767,#28768,#28769,#28770,#28771,#28772,#28773,#28774,
#28775,#28776,#28777,#28778,#28779,#28780,#28781,#28782,#28783,#28784,#28785,
#28786,#28787,#28788,#28789,#28790,#28791,#28792,#28793,#28794,#28795,#28796,
#28797,#28798,#28799,#28800,#28801,#28802,#28803,#28804,#28805,#28806,#28807,
#28808,#28809,#28810,#28811,#28812,#28813,#28814,#28815,#28816,#28817,#28818,
#28819,#28820,#28821,#28822,#28823,#28824,#28825,#28826,#28827,#28828,#28829,
#28830,#28831,#28832,#28833,#28834,#28835,#28836,#28837,#28838,#28839,#28840,
#28841,#28842,#28843,#28844,#28845,#28846,#28847,#28848,#28849,#28850,#28851,
#28852,#28853,#28854,#28855,#28856,#28857,#28858,#28859,#28860,#28861,#28862,
#28863,#28864,#28865,#28866,#28867,#28868,#28869,#28870,#28871,#28872,#28873,
#28874,#28875,#28876,#28877,#28878,#28879),(#28880,#28881,#28882,#28883,
#28884,#28885,#28886,#28887,#28888,#28889,#28890,#28891,#28892,#28893,#28894,
#28895,#28896,#28897,#28898,#28899,#28900,#28901,#28902,#28903,#28904,#28905,
#28906,#28907,#28908,#28909,#28910,#28911,#28912,#28913,#28914,#28915,#28916,
#28917,#28918,#28919,#28920,#28921,#28922,#28923,#28924,#28925,#28926,#28927,
#28928,#28929,#28930,#28931,#28932,#28933,#28934,#28935,#28936,#28937,#28938,
#28939,#28940,#28941,#28942,#28943,#28944,#28945,#28946,#28947,#28948,#28949,
#28950,#28951,#28952,#28953,#28954,#28955,#28956,#28957,#28958,#28959,#28960,
#28961,#28962,#28963,#28964,#28965,#28966,#28967,#28968,#28969,#28970,#28971,
#28972,#28973,#28974,#28975,#28976,#28977,#28978,#28979,#28980,#28981,#28982,
#28983,#28984,#28985,#28986,#28987,#28988,#28989,#28990,#28991,#28992,#28993,
#28994,#28995,#28996,#28997,#28998,#28999,#29000,#29001,#29002,#29003,#29004,
#29005,#29006,#29007,#29008,#29009,#29010,#29011,#29012,#29013,#29014,#29015,
#29016,#29017,#29018,#29019,#29020,#29021,#29022,#29023,#29024,#29025,#29026,
#29027,#29028,#29029,#29030,#29031,#29032,#29033,#29034,#29035,#29036,#29037,
#29038,#29039,#29040,#29041,#29042,#29043,#29044,#29045,#29046,#29047,#29048,
#29049,#29050,#29051,#29052,#29053,#29054,#29055,#29056,#29057,#29058,#29059,
#29060,#29061,#29062,#29063,#29064,#29065,#29066,#29067,#29068,#29069,#29070,
#29071,#29072,#29073,#29074,#29075,#29076,#29077,#29078,#29079,#29080,#29081,
#29082,#29083,#29084,#29085,#29086,#29087,#29088,#29089,#29090,#29091,#29092,
#29093,#29094,#29095,#29096,#29097,#29098,#29099,#29100,#29101,#29102,#29103,
#29104,#29105,#29106,#29107,#29108,#29109,#29110,#29111,#29112,#29113,#29114,
#29115,#29116,#29117,#29118,#29119,#29120,#29121,#29122,#29123,#29124,#29125,
#29126,#29127,#29128,#29129,#29130,#29131,#29132,#29133,#29134,#29135,#29136,
#29137,#29138,#29139,#29140,#29141,#29142,#29143,#29144,#29145,#29146,#29147,
#29148,#29149,#29150,#29151,#29152,#29153,#29154,#29155,#29156,#29157,#29158,
#29159,#29160,#29161,#29162,#29163,#29164,#29165,#29166,#29167,#29168,#29169,
#29170,#29171,#29172,#29173,#29174,#29175,#29176,#29177,#29178,#29179,#29180,
#29181,#29182,#29183,#29184,#29185,#29186,#29187,#29188,#29189),(#29190,
#29191,#29192,#29193,#29194,#29195,#29196,#29197,#29198,#29199,#29200,#29201,
#29202,#29203,#29204,#29205,#29206,#29207,#29208,#29209,#29210,#29211,#29212,
#29213,#29214,#29215,#29216,#29217,#29218,#29219,#29220,#29221,#29222,#29223,
#29224,#29225,#29226,#29227,#29228,#29229,#29230,#29231,#29232,#29233,#29234,
#29235,#29236,#29237,#29238,#29239,#29240,#29241,#29242,#29243,#29244,#29245,
#29246,#29247,#29248,#29249,#29250,#29251,#29252,#29253,#29254,#29255,#29256,
#29257,#29258,#29259,#29260,#29261,#29262,#29263,#29264,#29265,#29266,#29267,
#29268,#29269,#29270,#29271,#29272,#29273,#29274,#29275,#29276,#29277,#29278,
#29279,#29280,#29281,#29282,#29283,#29284,#29285,#29286,#29287,#29288,#29289,
#29290,#29291,#29292,#29293,#29294,#29295,#29296,#29297,#29298,#29299,#29300,
#29301,#29302,#29303,#29304,#29305,#29306,#29307,#29308,#29309,#29310,#29311,
#29312,#29313,#29314,#29315,#29316,#29317,#29318,#29319,#29320,#29321,#29322,
#29323,#29324,#29325,#29326,#29327,#29328,#29329,#29330,#29331,#29332,#29333,
#29334,#29335,#29336,#29337,#29338,#29339,#29340,#29341,#29342,#29343,#29344,
#29345,#29346,#29347,#29348,#29349,#29350,#29351,#29352,#29353,#29354,#29355,
#29356,#29357,#29358,#29359,#29360,#29361,#29362,#29363,#29364,#29365,#29366,
#29367,#29368,#29369,#29370,#29371,#29372,#29373,#29374,#29375,#29376,#29377,
#29378,#29379,#29380,#29381,#29382,#29383,#29384,#29385,#29386,#29387,#29388,
#29389,#29390,#29391,#29392,#29393,#29394,#29395,#29396,#29397,#29398,#29399,
#29400,#29401,#29402,#29403,#29404,#29405,#29406,#29407,#29408,#29409,#29410,
#29411,#29412,#29413,#29414,#29415,#29416,#29417,#29418,#29419,#29420,#29421,
#29422,#29423,#29424,#29425,#29426,#29427,#29428,#29429,#29430,#29431,#29432,
#29433,#29434,#29435,#29436,#29437,#29438,#29439,#29440,#29441,#29442,#29443,
#29444,#29445,#29446,#29447,#29448,#29449,#29450,#29451,#29452,#29453,#29454,
#29455,#29456,#29457,#29458,#29459,#29460,#29461,#29462,#29463,#29464,#29465,
#29466,#29467,#29468,#29469,#29470,#29471,#29472,#29473,#29474,#29475,#29476,
#29477,#29478,#29479,#29480,#29481,#29482,#29483,#29484,#29485,#29486,#29487,
#29488,#29489,#29490,#29491,#29492,#29493,#29494,#29495,#29496,#29497,#29498,
#29499),(#29500,#29501,#29502,#29503,#29504,#29505,#29506,#29507,#29508,
#29509,#29510,#29511,#29512,#29513,#29514,#29515,#29516,#29517,#29518,#29519,
#29520,#29521,#29522,#29523,#29524,#29525,#29526,#29527,#29528,#29529,#29530,
#29531,#29532,#29533,#29534,#29535,#29536,#29537,#29538,#29539,#29540,#29541,
#29542,#29543,#29544,#29545,#29546,#29547,#29548,#29549,#29550,#29551,#29552,
#29553,#29554,#29555,#29556,#29557,#29558,#29559,#29560,#29561,#29562,#29563,
#29564,#29565,#29566,#29567,#29568,#29569,#29570,#29571,#29572,#29573,#29574,
#29575,#29576,#29577,#29578,#29579,#29580,#29581,#29582,#29583,#29584,#29585,
#29586,#29587,#29588,#29589,#29590,#29591,#29592,#29593,#29594,#29595,#29596,
#29597,#29598,#29599,#29600,#29601,#29602,#29603,#29604,#29605,#29606,#29607,
#29608,#29609,#29610,#29611,#29612,#29613,#29614,#29615,#29616,#29617,#29618,
#29619,#29620,#29621,#29622,#29623,#29624,#29625,#29626,#29627,#29628,#29629,
#29630,#29631,#29632,#29633,#29634,#29635,#29636,#29637,#29638,#29639,#29640,
#29641,#29642,#29643,#29644,#29645,#29646,#29647,#29648,#29649,#29650,#29651,
#29652,#29653,#29654,#29655,#29656,#29657,#29658,#29659,#29660,#29661,#29662,
#29663,#29664,#29665,#29666,#29667,#29668,#29669,#29670,#29671,#29672,#29673,
#29674,#29675,#29676,#29677,#29678,#29679,#29680,#29681,#29682,#29683,#29684,
#29685,#29686,#29687,#29688,#29689,#29690,#29691,#29692,#29693,#29694,#29695,
#29696,#29697,#29698,#29699,#29700,#29701,#29702,#29703,#29704,#29705,#29706,
#29707,#29708,#29709,#29710,#29711,#29712,#29713,#29714,#29715,#29716,#29717,
#29718,#29719,#29720,#29721,#29722,#29723,#29724,#29725,#29726,#29727,#29728,
#29729,#29730,#29731,#29732,#29733,#29734,#29735,#29736,#29737,#29738,#29739,
#29740,#29741,#29742,#29743,#29744,#29745,#29746,#29747,#29748,#29749,#29750,
#29751,#29752,#29753,#29754,#29755,#29756,#29757,#29758,#29759,#29760,#29761,
#29762,#29763,#29764,#29765,#29766,#29767,#29768,#29769,#29770,#29771,#29772,
#29773,#29774,#29775,#29776,#29777,#29778,#29779,#29780,#29781,#29782,#29783,
#29784,#29785,#29786,#29787,#29788,#29789,#29790,#29791,#29792,#29793,#29794,
#29795,#29796,#29797,#29798,#29799,#29800,#29801,#29802,#29803,#29804,#29805,
#29806,#29807,#29808,#29809),(#29810,#29811,#29812,#29813,#29814,#29815,
#29816,#29817,#29818,#29819,#29820,#29821,#29822,#29823,#29824,#29825,#29826,
#29827,#29828,#29829,#29830,#29831,#29832,#29833,#29834,#29835,#29836,#29837,
#29838,#29839,#29840,#29841,#29842,#29843,#29844,#29845,#29846,#29847,#29848,
#29849,#29850,#29851,#29852,#29853,#29854,#29855,#29856,#29857,#29858,#29859,
#29860,#29861,#29862,#29863,#29864,#29865,#29866,#29867,#29868,#29869,#29870,
#29871,#29872,#29873,#29874,#29875,#29876,#29877,#29878,#29879,#29880,#29881,
#29882,#29883,#29884,#29885,#29886,#29887,#29888,#29889,#29890,#29891,#29892,
#29893,#29894,#29895,#29896,#29897,#29898,#29899,#29900,#29901,#29902,#29903,
#29904,#29905,#29906,#29907,#29908,#29909,#29910,#29911,#29912,#29913,#29914,
#29915,#29916,#29917,#29918,#29919,#29920,#29921,#29922,#29923,#29924,#29925,
#29926,#29927,#29928,#29929,#29930,#29931,#29932,#29933,#29934,#29935,#29936,
#29937,#29938,#29939,#29940,#29941,#29942,#29943,#29944,#29945,#29946,#29947,
#29948,#29949,#29950,#29951,#29952,#29953,#29954,#29955,#29956,#29957,#29958,
#29959,#29960,#29961,#29962,#29963,#29964,#29965,#29966,#29967,#29968,#29969,
#29970,#29971,#29972,#29973,#29974,#29975,#29976,#29977,#29978,#29979,#29980,
#29981,#29982,#29983,#29984,#29985,#29986,#29987,#29988,#29989,#29990,#29991,
#29992,#29993,#29994,#29995,#29996,#29997,#29998,#29999,#30000,#30001,#30002,
#30003,#30004,#30005,#30006,#30007,#30008,#30009,#30010,#30011,#30012,#30013,
#30014,#30015,#30016,#30017,#30018,#30019,#30020,#30021,#30022,#30023,#30024,
#30025,#30026,#30027,#30028,#30029,#30030,#30031,#30032,#30033,#30034,#30035,
#30036,#30037,#30038,#30039,#30040,#30041,#30042,#30043,#30044,#30045,#30046,
#30047,#30048,#30049,#30050,#30051,#30052,#30053,#30054,#30055,#30056,#30057,
#30058,#30059,#30060,#30061,#30062,#30063,#30064,#30065,#30066,#30067,#30068,
#30069,#30070,#30071,#30072,#30073,#30074,#30075,#30076,#30077,#30078,#30079,
#30080,#30081,#30082,#30083,#30084,#30085,#30086,#30087,#30088,#30089,#30090,
#30091,#30092,#30093,#30094,#30095,#30096,#30097,#30098,#30099,#30100,#30101,
#30102,#30103,#30104,#30105,#30106,#30107,#30108,#30109,#30110,#30111,#30112,
#30113,#30114,#30115,#30116,#30117,#30118,#30119),(#30120,#30121,#30122,
#30123,#30124,#30125,#30126,#30127,#30128,#30129,#30130,#30131,#30132,#30133,
#30134,#30135,#30136,#30137,#30138,#30139,#30140,#30141,#30142,#30143,#30144,
#30145,#30146,#30147,#30148,#30149,#30150,#30151,#30152,#30153,#30154,#30155,
#30156,#30157,#30158,#30159,#30160,#30161,#30162,#30163,#30164,#30165,#30166,
#30167,#30168,#30169,#30170,#30171,#30172,#30173,#30174,#30175,#30176,#30177,
#30178,#30179,#30180,#30181,#30182,#30183,#30184,#30185,#30186,#30187,#30188,
#30189,#30190,#30191,#30192,#30193,#30194,#30195,#30196,#30197,#30198,#30199,
#30200,#30201,#30202,#30203,#30204,#30205,#30206,#30207,#30208,#30209,#30210,
#30211,#30212,#30213,#30214,#30215,#30216,#30217,#30218,#30219,#30220,#30221,
#30222,#30223,#30224,#30225,#30226,#30227,#30228,#30229,#30230,#30231,#30232,
#30233,#30234,#30235,#30236,#30237,#30238,#30239,#30240,#30241,#30242,#30243,
#30244,#30245,#30246,#30247,#30248,#30249,#30250,#30251,#30252,#30253,#30254,
#30255,#30256,#30257,#30258,#30259,#30260,#30261,#30262,#30263,#30264,#30265,
#30266,#30267,#30268,#30269,#30270,#30271,#30272,#30273,#30274,#30275,#30276,
#30277,#30278,#30279,#30280,#30281,#30282,#30283,#30284,#30285,#30286,#30287,
#30288,#30289,#30290,#30291,#30292,#30293,#30294,#30295,#30296,#30297,#30298,
#30299,#30300,#30301,#30302,#30303,#30304,#30305,#30306,#30307,#30308,#30309,
#30310,#30311,#30312,#30313,#30314,#30315,#30316,#30317,#30318,#30319,#30320,
#30321,#30322,#30323,#30324,#30325,#30326,#30327,#30328,#30329,#30330,#30331,
#30332,#30333,#30334,#30335,#30336,#30337,#30338,#30339,#30340,#30341,#30342,
#30343,#30344,#30345,#30346,#30347,#30348,#30349,#30350,#30351,#30352,#30353,
#30354,#30355,#30356,#30357,#30358,#30359,#30360,#30361,#30362,#30363,#30364,
#30365,#30366,#30367,#30368,#30369,#30370,#30371,#30372,#30373,#30374,#30375,
#30376,#30377,#30378,#30379,#30380,#30381,#30382,#30383,#30384,#30385,#30386,
#30387,#30388,#30389,#30390,#30391,#30392,#30393,#30394,#30395,#30396,#30397,
#30398,#30399,#30400,#30401,#30402,#30403,#30404,#30405,#30406,#30407,#30408,
#30409,#30410,#30411,#30412,#30413,#30414,#30415,#30416,#30417,#30418,#30419,
#30420,#30421,#30422,#30423,#30424,#30425,#30426,#30427,#30428,#30429),
(#30430,#30431,#30432,#30433,#30434,#30435,#30436,#30437,#30438,#30439,
#30440,#30441,#30442,#30443,#30444,#30445,#30446,#30447,#30448,#30449,#30450,
#30451,#30452,#30453,#30454,#30455,#30456,#30457,#30458,#30459,#30460,#30461,
#30462,#30463,#30464,#30465,#30466,#30467,#30468,#30469,#30470,#30471,#30472,
#30473,#30474,#30475,#30476,#30477,#30478,#30479,#30480,#30481,#30482,#30483,
#30484,#30485,#30486,#30487,#30488,#30489,#30490,#30491,#30492,#30493,#30494,
#30495,#30496,#30497,#30498,#30499,#30500,#30501,#30502,#30503,#30504,#30505,
#30506,#30507,#30508,#30509,#30510,#30511,#30512,#30513,#30514,#30515,#30516,
#30517,#30518,#30519,#30520,#30521,#30522,#30523,#30524,#30525,#30526,#30527,
#30528,#30529,#30530,#30531,#30532,#30533,#30534,#30535,#30536,#30537,#30538,
#30539,#30540,#30541,#30542,#30543,#30544,#30545,#30546,#30547,#30548,#30549,
#30550,#30551,#30552,#30553,#30554,#30555,#30556,#30557,#30558,#30559,#30560,
#30561,#30562,#30563,#30564,#30565,#30566,#30567,#30568,#30569,#30570,#30571,
#30572,#30573,#30574,#30575,#30576,#30577,#30578,#30579,#30580,#30581,#30582,
#30583,#30584,#30585,#30586,#30587,#30588,#30589,#30590,#30591,#30592,#30593,
#30594,#30595,#30596,#30597,#30598,#30599,#30600,#30601,#30602,#30603,#30604,
#30605,#30606,#30607,#30608,#30609,#30610,#30611,#30612,#30613,#30614,#30615,
#30616,#30617,#30618,#30619,#30620,#30621,#30622,#30623,#30624,#30625,#30626,
#30627,#30628,#30629,#30630,#30631,#30632,#30633,#30634,#30635,#30636,#30637,
#30638,#30639,#30640,#30641,#30642,#30643,#30644,#30645,#30646,#30647,#30648,
#30649,#30650,#30651,#30652,#30653,#30654,#30655,#30656,#30657,#30658,#30659,
#30660,#30661,#30662,#30663,#30664,#30665,#30666,#30667,#30668,#30669,#30670,
#30671,#30672,#30673,#30674,#30675,#30676,#30677,#30678,#30679,#30680,#30681,
#30682,#30683,#30684,#30685,#30686,#30687,#30688,#30689,#30690,#30691,#30692,
#30693,#30694,#30695,#30696,#30697,#30698,#30699,#30700,#30701,#30702,#30703,
#30704,#30705,#30706,#30707,#30708,#30709,#30710,#30711,#30712,#30713,#30714,
#30715,#30716,#30717,#30718,#30719,#30720,#30721,#30722,#30723,#30724,#30725,
#30726,#30727,#30728,#30729,#30730,#30731,#30732,#30733,#30734,#30735,#30736,
#30737,#30738,#30739)),.UNSPECIFIED.,.T.,.F.,.F.)
B_SPLINE_SURFACE_WITH_KNOTS((4,3,4),(4,2,2,2,2,2,2,2,2,2,2,2,2,2,2,2,2,
2,2,2,2,2,2,2,2,2,2,2,2,2,2,2,2,2,2,2,2,2,2,2,2,2,2,2,2,2,2,2,2,2,2,2,2,
2,2,2,2,2,2,2,2,2,2,2,2,2,2,2,2,2,2,2,2,2,2,2,2,2,2,2,2,2,2,2,2,2,2,2,2,
2,2,2,2,2,2,2,2,2,2,2,2,2,2,2,2,2,2,2,2,2,2,2,2,2,2,2,2,2,2,2,2,2,2,2,2,
2,2,2,2,2,2,2,2,2,2,2,2,2,2,2,2,2,2,2,2,2,2,2,2,2,2,2,2,2,4),(0.,0.5,1.),
(0.,0.00568181818181819,0.0184659090909091,0.0248579545454546,0.03125,0.0376420454545455,
0.044034090909091,0.0504261363636365,0.0568181818181819,0.0632102272727274,
0.0696022727272729,0.0759943181818183,0.0823863636363638,0.0887784090909093,
0.0951704545454547,0.1015625,0.107954545454546,0.114346590909092,0.120738636363638,
0.127130681818185,0.133522727272731,0.139914772727278,0.146306818181824,
0.152698863636371,0.159090909090917,0.165482954545461,0.171875000000006,
0.17826704545455,0.184659090909095,0.19105113636364,0.197443181818184,0.203835227272728,
0.210227272727273,0.216619318181819,0.223011363636364,0.22940340909091,
0.235795454545455,0.2421875,0.248579545454546,0.254971590909091,0.261363636363637,
0.267755681818182,0.274147727272728,0.280539772727273,0.286931818181819,
0.293323863636364,0.29971590909091,0.306107954545455,0.3125,0.318892045454546,
0.325284090909092,0.331676136363637,0.338068181818183,0.344460227272728,
0.350852272727274,0.357244318181819,0.363636363636365,0.37002840909091,
0.376420454545456,0.3828125,0.389204545454547,0.395596590909092,0.401988636363638,
0.408380681818183,0.414772727272729,0.421164772727273,0.427556818181818,
0.433948863636362,0.440340909090907,0.446732954545451,0.453125,0.45951704545454,
0.465909090909084,0.472301136363631,0.478693181818177,0.485085227272724,
0.49147727272727,0.497869318181817,0.504261363636363,0.51065340909091,0.517045454545456,
0.5234375,0.529829545454547,0.536221590909093,0.542613636363638,0.549005681818184,
0.555397727272729,0.561789772727275,0.56818181818182,0.574573863636366,
0.580965909090911,0.587357954545456,0.59375,0.600142045454547,0.606534090909093,
0.612926136363638,0.619318181818184,0.625710227272729,0.632102272727275,
0.63849431818182,0.644886363636365,0.651278409090911,0.657670454545456,
0.6640625,0.670454545454547,0.676846590909094,0.68323863636364,0.689630681818186,
0.696022727272733,0.702414772727279,0.708806818181825,0.715198863636372,
0.721590909090918,0.727982954545463,0.734375,0.740767045454552,0.747159090909096,
0.753551136363641,0.759943181818185,0.766335227272729,0.772727272727274,
0.779119318181819,0.785511363636365,0.79190340909091,0.798295454545456,
0.8046875,0.811079545454546,0.817471590909092,0.823863636363637,0.830255681818183,
0.836647727272728,0.843039772727274,0.849431818181819,0.855823863636364,
0.86221590909091,0.868607954545455,0.875,0.881392045454546,0.887784090909092,
0.894176136363637,0.900568181818182,0.906960227272728,0.913352272727273,
0.919744318181819,0.926136363636364,0.932528409090909,0.938920454545455,
0.9453125,0.951704545454546,0.958096590909091,0.964488636363636,0.970880681818182,
0.977272727272727,0.988636363636364,1.),.UNSPECIFIED.)
GEOMETRIC_REPRESENTATION_ITEM()
RATIONAL_B_SPLINE_SURFACE(((1.,1.,1.,1.,1.,1.,1.,1.,1.,1.,1.,1.,1.,1.,1.,
1.,1.,1.,1.,1.,1.,1.,1.,1.,1.,1.,1.,1.,1.,1.,1.,1.,1.,1.,1.,1.,1.,1.,1.,
1.,1.,1.,1.,1.,1.,1.,1.,1.,1.,1.,1.,1.,1.,1.,1.,1.,1.,1.,1.,1.,1.,1.,1.,
1.,1.,1.,1.,1.,1.,1.,1.,1.,1.,1.,1.,1.,1.,1.,1.,1.,1.,1.,1.,1.,1.,1.,1.,
1.,1.,1.,1.,1.,1.,1.,1.,1.,1.,1.,1.,1.,1.,1.,1.,1.,1.,1.,1.,1.,1.,1.,1.,
1.,1.,1.,1.,1.,1.,1.,1.,1.,1.,1.,1.,1.,1.,1.,1.,1.,1.,1.,1.,1.,1.,1.,1.,
1.,1.,1.,1.,1.,1.,1.,1.,1.,1.,1.,1.,1.,1.,1.,1.,1.,1.,1.,1.,1.,1.,1.,1.,
1.,1.,1.,1.,1.,1.,1.,1.,1.,1.,1.,1.,1.,1.,1.,1.,1.,1.,1.,1.,1.,1.,1.,1.,
1.,1.,1.,1.,1.,1.,1.,1.,1.,1.,1.,1.,1.,1.,1.,1.,1.,1.,1.,1.,1.,1.,1.,1.,
1.,1.,1.,1.,1.,1.,1.,1.,1.,1.,1.,1.,1.,1.,1.,1.,1.,1.,1.,1.,1.,1.,1.,1.,
1.,1.,1.,1.,1.,1.,1.,1.,1.,1.,1.,1.,1.,1.,1.,1.,1.,1.,1.,1.,1.,1.,1.,1.,
1.,1.,1.,1.,1.,1.,1.,1.,1.,1.,1.,1.,1.,1.,1.,1.,1.,1.,1.,1.,1.,1.,1.,1.,
1.,1.,1.,1.,1.,1.,1.,1.,1.,1.,1.,1.,1.,1.,1.,1.,1.,1.,1.,1.,1.,1.,1.,1.,
1.,1.,1.,1.,1.,1.,1.),(0.333333333333334,0.333333333333334,0.333333333333334,
0.333333333333334,0.333333333333334,0.333333333333334,0.333333333333334,
0.333333333333334,0.333333333333334,0.333333333333334,0.333333333333334,
0.333333333333334,0.333333333333334,0.333333333333334,0.333333333333334,
0.333333333333334,0.333333333333334,0.333333333333334,0.333333333333334,
0.333333333333334,0.333333333333334,0.333333333333334,0.333333333333334,
0.333333333333334,0.333333333333334,0.333333333333334,0.333333333333334,
0.333333333333334,0.333333333333334,0.333333333333334,0.333333333333334,
0.333333333333334,0.333333333333334,0.333333333333334,0.333333333333334,
0.333333333333334,0.333333333333334,0.333333333333334,0.333333333333334,
0.333333333333334,0.333333333333334,0.333333333333334,0.333333333333334,
0.333333333333334,0.333333333333334,0.333333333333334,0.333333333333334,
0.333333333333334,0.333333333333334,0.333333333333334,0.333333333333334,
0.333333333333334,0.333333333333334,0.333333333333334,0.333333333333334,
0.333333333333334,0.333333333333334,0.333333333333334,0.333333333333334,
0.333333333333334,0.333333333333334,0.333333333333334,0.333333333333334,
0.333333333333334,0.333333333333334,0.333333333333334,0.333333333333334,
0.333333333333334,0.333333333333334,0.333333333333334,0.333333333333334,
0.333333333333334,0.333333333333334,0.333333333333334,0.333333333333334,
0.333333333333334,0.333333333333334,0.333333333333334,0.333333333333334,
0.333333333333334,0.333333333333334,0.333333333333334,0.333333333333334,
0.333333333333334,0.333333333333334,0.333333333333334,0.333333333333334,
0.333333333333334,0.333333333333334,0.333333333333334,0.333333333333334,
0.333333333333334,0.333333333333334,0.333333333333334,0.333333333333334,
0.333333333333334,0.333333333333334,0.333333333333334,0.333333333333334,
0.333333333333334,0.333333333333334,0.333333333333334,0.333333333333334,
0.333333333333334,0.333333333333334,0.333333333333334,0.333333333333334,
0.333333333333334,0.333333333333334,0.333333333333334,0.333333333333334,
0.333333333333334,0.333333333333334,0.333333333333334,0.333333333333334,
0.333333333333334,0.333333333333334,0.333333333333334,0.333333333333334,
0.333333333333334,0.333333333333334,0.333333333333334,0.333333333333334,
0.333333333333334,0.333333333333334,0.333333333333334,0.333333333333334,
0.333333333333334,0.333333333333334,0.333333333333334,0.333333333333334,
0.333333333333334,0.333333333333334,0.333333333333334,0.333333333333334,
0.333333333333334,0.333333333333334,0.333333333333334,0.333333333333334,
0.333333333333334,0.333333333333334,0.333333333333334,0.333333333333334,
0.333333333333334,0.333333333333334,0.333333333333334,0.333333333333334,
0.333333333333334,0.333333333333334,0.333333333333334,0.333333333333334,
0.333333333333334,0.333333333333334,0.333333333333334,0.333333333333334,
0.333333333333334,0.333333333333334,0.333333333333334,0.333333333333334,
0.333333333333334,0.333333333333334,0.333333333333334,0.333333333333334,
0.333333333333334,0.333333333333334,0.333333333333334,0.333333333333334,
0.333333333333334,0.333333333333334,0.333333333333334,0.333333333333334,
0.333333333333334,0.333333333333334,0.333333333333334,0.333333333333334,
0.333333333333334,0.333333333333334,0.333333333333334,0.333333333333334,
0.333333333333334,0.333333333333334,0.333333333333334,0.333333333333334,
0.333333333333334,0.333333333333334,0.333333333333334,0.333333333333334,
0.333333333333334,0.333333333333334,0.333333333333334,0.333333333333334,
0.333333333333334,0.333333333333334,0.333333333333334,0.333333333333334,
0.333333333333334,0.333333333333334,0.333333333333334,0.333333333333334,
0.333333333333334,0.333333333333334,0.333333333333334,0.333333333333334,
0.333333333333334,0.333333333333334,0.333333333333334,0.333333333333334,
0.333333333333334,0.333333333333334,0.333333333333334,0.333333333333334,
0.333333333333334,0.333333333333334,0.333333333333334,0.333333333333334,
0.333333333333334,0.333333333333334,0.333333333333334,0.333333333333334,
0.333333333333334,0.333333333333334,0.333333333333334,0.333333333333334,
0.333333333333334,0.333333333333334,0.333333333333334,0.333333333333334,
0.333333333333334,0.333333333333334,0.333333333333334,0.333333333333334,
0.333333333333334,0.333333333333334,0.333333333333334,0.333333333333334,
0.333333333333334,0.333333333333334,0.333333333333334,0.333333333333334,
0.333333333333334,0.333333333333334,0.333333333333334,0.333333333333334,
0.333333333333334,0.333333333333334,0.333333333333334,0.333333333333334,
0.333333333333334,0.333333333333334,0.333333333333334,0.333333333333334,
0.333333333333334,0.333333333333334,0.333333333333334,0.333333333333334,
0.333333333333334,0.333333333333334,0.333333333333334,0.333333333333334,
0.333333333333334,0.333333333333334,0.333333333333334,0.333333333333334,
0.333333333333334,0.333333333333334,0.333333333333334,0.333333333333334,
0.333333333333334,0.333333333333334,0.333333333333334,0.333333333333334,
0.333333333333334,0.333333333333334,0.333333333333334,0.333333333333334,
0.333333333333334,0.333333333333334,0.333333333333334,0.333333333333334,
0.333333333333334,0.333333333333334,0.333333333333334,0.333333333333334,
0.333333333333334,0.333333333333334,0.333333333333334,0.333333333333334,
0.333333333333334,0.333333333333334,0.333333333333334,0.333333333333334,
0.333333333333334,0.333333333333334,0.333333333333334,0.333333333333334,
0.333333333333334,0.333333333333334,0.333333333333334,0.333333333333334,
0.333333333333334,0.333333333333334,0.333333333333334,0.333333333333334,
0.333333333333334,0.333333333333334,0.333333333333334,0.333333333333334,
0.333333333333334,0.333333333333334,0.333333333333334),(0.333333333333334,
0.333333333333334,0.333333333333334,0.333333333333334,0.333333333333334,
0.333333333333334,0.333333333333334,0.333333333333334,0.333333333333334,
0.333333333333334,0.333333333333334,0.333333333333334,0.333333333333334,
0.333333333333334,0.333333333333334,0.333333333333334,0.333333333333334,
0.333333333333334,0.333333333333334,0.333333333333334,0.333333333333334,
0.333333333333334,0.333333333333334,0.333333333333334,0.333333333333334,
0.333333333333334,0.333333333333334,0.333333333333334,0.333333333333334,
0.333333333333334,0.333333333333334,0.333333333333334,0.333333333333334,
0.333333333333334,0.333333333333334,0.333333333333334,0.333333333333334,
0.333333333333334,0.333333333333334,0.333333333333334,0.333333333333334,
0.333333333333334,0.333333333333334,0.333333333333334,0.333333333333334,
0.333333333333334,0.333333333333334,0.333333333333334,0.333333333333334,
0.333333333333334,0.333333333333334,0.333333333333334,0.333333333333334,
0.333333333333334,0.333333333333334,0.333333333333334,0.333333333333334,
0.333333333333334,0.333333333333334,0.333333333333334,0.333333333333334,
0.333333333333334,0.333333333333334,0.333333333333334,0.333333333333334,
0.333333333333334,0.333333333333334,0.333333333333334,0.333333333333334,
0.333333333333334,0.333333333333334,0.333333333333334,0.333333333333334,
0.333333333333334,0.333333333333334,0.333333333333334,0.333333333333334,
0.333333333333334,0.333333333333334,0.333333333333334,0.333333333333334,
0.333333333333334,0.333333333333334,0.333333333333334,0.333333333333334,
0.333333333333334,0.333333333333334,0.333333333333334,0.333333333333334,
0.333333333333334,0.333333333333334,0.333333333333334,0.333333333333334,
0.333333333333334,0.333333333333334,0.333333333333334,0.333333333333334,
0.333333333333334,0.333333333333334,0.333333333333334,0.333333333333334,
0.333333333333334,0.333333333333334,0.333333333333334,0.333333333333334,
0.333333333333334,0.333333333333334,0.333333333333334,0.333333333333334,
0.333333333333334,0.333333333333334,0.333333333333334,0.333333333333334,
0.333333333333334,0.333333333333334,0.333333333333334,0.333333333333334,
0.333333333333334,0.333333333333334,0.333333333333334,0.333333333333334,
0.333333333333334,0.333333333333334,0.333333333333334,0.333333333333334,
0.333333333333334,0.333333333333334,0.333333333333334,0.333333333333334,
0.333333333333334,0.333333333333334,0.333333333333334,0.333333333333334,
0.333333333333334,0.333333333333334,0.333333333333334,0.333333333333334,
0.333333333333334,0.333333333333334,0.333333333333334,0.333333333333334,
0.333333333333334,0.333333333333334,0.333333333333334,0.333333333333334,
0.333333333333334,0.333333333333334,0.333333333333334,0.333333333333334,
0.333333333333334,0.333333333333334,0.333333333333334,0.333333333333334,
0.333333333333334,0.333333333333334,0.333333333333334,0.333333333333334,
0.333333333333334,0.333333333333334,0.333333333333334,0.333333333333334,
0.333333333333334,0.333333333333334,0.333333333333334,0.333333333333334,
0.333333333333334,0.333333333333334,0.333333333333334,0.333333333333334,
0.333333333333334,0.333333333333334,0.333333333333334,0.333333333333334,
0.333333333333334,0.333333333333334,0.333333333333334,0.333333333333334,
0.333333333333334,0.333333333333334,0.333333333333334,0.333333333333334,
0.333333333333334,0.333333333333334,0.333333333333334,0.333333333333334,
0.333333333333334,0.333333333333334,0.333333333333334,0.333333333333334,
0.333333333333334,0.333333333333334,0.333333333333334,0.333333333333334,
0.333333333333334,0.333333333333334,0.333333333333334,0.333333333333334,
0.333333333333334,0.333333333333334,0.333333333333334,0.333333333333334,
0.333333333333334,0.333333333333334,0.333333333333334,0.333333333333334,
0.333333333333334,0.333333333333334,0.333333333333334,0.333333333333334,
0.333333333333334,0.333333333333334,0.333333333333334,0.333333333333334,
0.333333333333334,0.333333333333334,0.333333333333334,0.333333333333334,
0.333333333333334,0.333333333333334,0.333333333333334,0.333333333333334,
0.333333333333334,0.333333333333334,0.333333333333334,0.333333333333334,
0.333333333333334,0.333333333333334,0.333333333333334,0.333333333333334,
0.333333333333334,0.333333333333334,0.333333333333334,0.333333333333334,
0.333333333333334,0.333333333333334,0.333333333333334,0.333333333333334,
0.333333333333334,0.333333333333334,0.333333333333334,0.333333333333334,
0.333333333333334,0.333333333333334,0.333333333333334,0.333333333333334,
0.333333333333334,0.333333333333334,0.333333333333334,0.333333333333334,
0.333333333333334,0.333333333333334,0.333333333333334,0.333333333333334,
0.333333333333334,0.333333333333334,0.333333333333334,0.333333333333334,
0.333333333333334,0.333333333333334,0.333333333333334,0.333333333333334,
0.333333333333334,0.333333333333334,0.333333333333334,0.333333333333334,
0.333333333333334,0.333333333333334,0.333333333333334,0.333333333333334,
0.333333333333334,0.333333333333334,0.333333333333334,0.333333333333334,
0.333333333333334,0.333333333333334,0.333333333333334,0.333333333333334,
0.333333333333334,0.333333333333334,0.333333333333334,0.333333333333334,
0.333333333333334,0.333333333333334,0.333333333333334,0.333333333333334,
0.333333333333334,0.333333333333334,0.333333333333334,0.333333333333334,
0.333333333333334,0.333333333333334,0.333333333333334,0.333333333333334,
0.333333333333334,0.333333333333334,0.333333333333334,0.333333333333334,
0.333333333333334,0.333333333333334,0.333333333333334,0.333333333333334,
0.333333333333334,0.333333333333334,0.333333333333334,0.333333333333334,
0.333333333333334,0.333333333333334,0.333333333333334,0.333333333333334,
0.333333333333334),(1.,1.,1.,1.,1.,1.,1.,1.,1.,1.,1.,1.,1.,1.,1.,1.,1.,
1.,1.,1.,1.,1.,1.,1.,1.,1.,1.,1.,1.,1.,1.,1.,1.,1.,1.,1.,1.,1.,1.,1.,1.,
1.,1.,1.,1.,1.,1.,1.,1.,1.,1.,1.,1.,1.,1.,1.,1.,1.,1.,1.,1.,1.,1.,1.,1.,
1.,1.,1.,1.,1.,1.,1.,1.,1.,1.,1.,1.,1.,1.,1.,1.,1.,1.,1.,1.,1.,1.,1.,1.,
1.,1.,1.,1.,1.,1.,1.,1.,1.,1.,1.,1.,1.,1.,1.,1.,1.,1.,1.,1.,1.,1.,1.,1.,
1.,1.,1.,1.,1.,1.,1.,1.,1.,1.,1.,1.,1.,1.,1.,1.,1.,1.,1.,1.,1.,1.,1.,1.,
1.,1.,1.,1.,1.,1.,1.,1.,1.,1.,1.,1.,1.,1.,1.,1.,1.,1.,1.,1.,1.,1.,1.,1.,
1.,1.,1.,1.,1.,1.,1.,1.,1.,1.,1.,1.,1.,1.,1.,1.,1.,1.,1.,1.,1.,1.,1.,1.,
1.,1.,1.,1.,1.,1.,1.,1.,1.,1.,1.,1.,1.,1.,1.,1.,1.,1.,1.,1.,1.,1.,1.,1.,
1.,1.,1.,1.,1.,1.,1.,1.,1.,1.,1.,1.,1.,1.,1.,1.,1.,1.,1.,1.,1.,1.,1.,1.,
1.,1.,1.,1.,1.,1.,1.,1.,1.,1.,1.,1.,1.,1.,1.,1.,1.,1.,1.,1.,1.,1.,1.,1.,
1.,1.,1.,1.,1.,1.,1.,1.,1.,1.,1.,1.,1.,1.,1.,1.,1.,1.,1.,1.,1.,1.,1.,1.,
1.,1.,1.,1.,1.,1.,1.,1.,1.,1.,1.,1.,1.,1.,1.,1.,1.,1.,1.,1.,1.,1.,1.,1.,
1.,1.,1.,1.,1.),(0.333333333333334,0.333333333333334,0.333333333333334,
0.333333333333334,0.333333333333334,0.333333333333334,0.333333333333334,
0.333333333333334,0.333333333333334,0.333333333333334,0.333333333333334,
0.333333333333334,0.333333333333334,0.333333333333334,0.333333333333334,
0.333333333333334,0.333333333333334,0.333333333333334,0.333333333333334,
0.333333333333334,0.333333333333334,0.333333333333334,0.333333333333334,
0.333333333333334,0.333333333333334,0.333333333333334,0.333333333333334,
0.333333333333334,0.333333333333334,0.333333333333334,0.333333333333334,
0.333333333333334,0.333333333333334,0.333333333333334,0.333333333333334,
0.333333333333334,0.333333333333334,0.333333333333334,0.333333333333334,
0.333333333333334,0.333333333333334,0.333333333333334,0.333333333333334,
0.333333333333334,0.333333333333334,0.333333333333334,0.333333333333334,
0.333333333333334,0.333333333333334,0.333333333333334,0.333333333333334,
0.333333333333334,0.333333333333334,0.333333333333334,0.333333333333334,
0.333333333333334,0.333333333333334,0.333333333333334,0.333333333333334,
0.333333333333334,0.333333333333334,0.333333333333334,0.333333333333334,
0.333333333333334,0.333333333333334,0.333333333333334,0.333333333333334,
0.333333333333334,0.333333333333334,0.333333333333334,0.333333333333334,
0.333333333333334,0.333333333333334,0.333333333333334,0.333333333333334,
0.333333333333334,0.333333333333334,0.333333333333334,0.333333333333334,
0.333333333333334,0.333333333333334,0.333333333333334,0.333333333333334,
0.333333333333334,0.333333333333334,0.333333333333334,0.333333333333334,
0.333333333333334,0.333333333333334,0.333333333333334,0.333333333333334,
0.333333333333334,0.333333333333334,0.333333333333334,0.333333333333334,
0.333333333333334,0.333333333333334,0.333333333333334,0.333333333333334,
0.333333333333334,0.333333333333334,0.333333333333334,0.333333333333334,
0.333333333333334,0.333333333333334,0.333333333333334,0.333333333333334,
0.333333333333334,0.333333333333334,0.333333333333334,0.333333333333334,
0.333333333333334,0.333333333333334,0.333333333333334,0.333333333333334,
0.333333333333334,0.333333333333334,0.333333333333334,0.333333333333334,
0.333333333333334,0.333333333333334,0.333333333333334,0.333333333333334,
0.333333333333334,0.333333333333334,0.333333333333334,0.333333333333334,
0.333333333333334,0.333333333333334,0.333333333333334,0.333333333333334,
0.333333333333334,0.333333333333334,0.333333333333334,0.333333333333334,
0.333333333333334,0.333333333333334,0.333333333333334,0.333333333333334,
0.333333333333334,0.333333333333334,0.333333333333334,0.333333333333334,
0.333333333333334,0.333333333333334,0.333333333333334,0.333333333333334,
0.333333333333334,0.333333333333334,0.333333333333334,0.333333333333334,
0.333333333333334,0.333333333333334,0.333333333333334,0.333333333333334,
0.333333333333334,0.333333333333334,0.333333333333334,0.333333333333334,
0.333333333333334,0.333333333333334,0.333333333333334,0.333333333333334,
0.333333333333334,0.333333333333334,0.333333333333334,0.333333333333334,
0.333333333333334,0.333333333333334,0.333333333333334,0.333333333333334,
0.333333333333334,0.333333333333334,0.333333333333334,0.333333333333334,
0.333333333333334,0.333333333333334,0.333333333333334,0.333333333333334,
0.333333333333334,0.333333333333334,0.333333333333334,0.333333333333334,
0.333333333333334,0.333333333333334,0.333333333333334,0.333333333333334,
0.333333333333334,0.333333333333334,0.333333333333334,0.333333333333334,
0.333333333333334,0.333333333333334,0.333333333333334,0.333333333333334,
0.333333333333334,0.333333333333334,0.333333333333334,0.333333333333334,
0.333333333333334,0.333333333333334,0.333333333333334,0.333333333333334,
0.333333333333334,0.333333333333334,0.333333333333334,0.333333333333334,
0.333333333333334,0.333333333333334,0.333333333333334,0.333333333333334,
0.333333333333334,0.333333333333334,0.333333333333334,0.333333333333334,
0.333333333333334,0.333333333333334,0.333333333333334,0.333333333333334,
0.333333333333334,0.333333333333334,0.333333333333334,0.333333333333334,
0.333333333333334,0.333333333333334,0.333333333333334,0.333333333333334,
0.333333333333334,0.333333333333334,0.333333333333334,0.333333333333334,
0.333333333333334,0.333333333333334,0.333333333333334,0.333333333333334,
0.333333333333334,0.333333333333334,0.333333333333334,0.333333333333334,
0.333333333333334,0.333333333333334,0.333333333333334,0.333333333333334,
0.333333333333334,0.333333333333334,0.333333333333334,0.333333333333334,
0.333333333333334,0.333333333333334,0.333333333333334,0.333333333333334,
0.333333333333334,0.333333333333334,0.333333333333334,0.333333333333334,
0.333333333333334,0.333333333333334,0.333333333333334,0.333333333333334,
0.333333333333334,0.333333333333334,0.333333333333334,0.333333333333334,
0.333333333333334,0.333333333333334,0.333333333333334,0.333333333333334,
0.333333333333334,0.333333333333334,0.333333333333334,0.333333333333334,
0.333333333333334,0.333333333333334,0.333333333333334,0.333333333333334,
0.333333333333334,0.333333333333334,0.333333333333334,0.333333333333334,
0.333333333333334,0.333333333333334,0.333333333333334,0.333333333333334,
0.333333333333334,0.333333333333334,0.333333333333334,0.333333333333334,
0.333333333333334,0.333333333333334,0.333333333333334,0.333333333333334,
0.333333333333334,0.333333333333334,0.333333333333334,0.333333333333334,
0.333333333333334,0.333333333333334,0.333333333333334,0.333333333333334,
0.333333333333334,0.333333333333334,0.333333333333334,0.333333333333334,
0.333333333333334,0.333333333333334,0.333333333333334,0.333333333333334,
0.333333333333334,0.333333333333334,0.333333333333334),(0.333333333333334,
0.333333333333334,0.333333333333334,0.333333333333334,0.333333333333334,
0.333333333333334,0.333333333333334,0.333333333333334,0.333333333333334,
0.333333333333334,0.333333333333334,0.333333333333334,0.333333333333334,
0.333333333333334,0.333333333333334,0.333333333333334,0.333333333333334,
0.333333333333334,0.333333333333334,0.333333333333334,0.333333333333334,
0.333333333333334,0.333333333333334,0.333333333333334,0.333333333333334,
0.333333333333334,0.333333333333334,0.333333333333334,0.333333333333334,
0.333333333333334,0.333333333333334,0.333333333333334,0.333333333333334,
0.333333333333334,0.333333333333334,0.333333333333334,0.333333333333334,
0.333333333333334,0.333333333333334,0.333333333333334,0.333333333333334,
0.333333333333334,0.333333333333334,0.333333333333334,0.333333333333334,
0.333333333333334,0.333333333333334,0.333333333333334,0.333333333333334,
0.333333333333334,0.333333333333334,0.333333333333334,0.333333333333334,
0.333333333333334,0.333333333333334,0.333333333333334,0.333333333333334,
0.333333333333334,0.333333333333334,0.333333333333334,0.333333333333334,
0.333333333333334,0.333333333333334,0.333333333333334,0.333333333333334,
0.333333333333334,0.333333333333334,0.333333333333334,0.333333333333334,
0.333333333333334,0.333333333333334,0.333333333333334,0.333333333333334,
0.333333333333334,0.333333333333334,0.333333333333334,0.333333333333334,
0.333333333333334,0.333333333333334,0.333333333333334,0.333333333333334,
0.333333333333334,0.333333333333334,0.333333333333334,0.333333333333334,
0.333333333333334,0.333333333333334,0.333333333333334,0.333333333333334,
0.333333333333334,0.333333333333334,0.333333333333334,0.333333333333334,
0.333333333333334,0.333333333333334,0.333333333333334,0.333333333333334,
0.333333333333334,0.333333333333334,0.333333333333334,0.333333333333334,
0.333333333333334,0.333333333333334,0.333333333333334,0.333333333333334,
0.333333333333334,0.333333333333334,0.333333333333334,0.333333333333334,
0.333333333333334,0.333333333333334,0.333333333333334,0.333333333333334,
0.333333333333334,0.333333333333334,0.333333333333334,0.333333333333334,
0.333333333333334,0.333333333333334,0.333333333333334,0.333333333333334,
0.333333333333334,0.333333333333334,0.333333333333334,0.333333333333334,
0.333333333333334,0.333333333333334,0.333333333333334,0.333333333333334,
0.333333333333334,0.333333333333334,0.333333333333334,0.333333333333334,
0.333333333333334,0.333333333333334,0.333333333333334,0.333333333333334,
0.333333333333334,0.333333333333334,0.333333333333334,0.333333333333334,
0.333333333333334,0.333333333333334,0.333333333333334,0.333333333333334,
0.333333333333334,0.333333333333334,0.333333333333334,0.333333333333334,
0.333333333333334,0.333333333333334,0.333333333333334,0.333333333333334,
0.333333333333334,0.333333333333334,0.333333333333334,0.333333333333334,
0.333333333333334,0.333333333333334,0.333333333333334,0.333333333333334,
0.333333333333334,0.333333333333334,0.333333333333334,0.333333333333334,
0.333333333333334,0.333333333333334,0.333333333333334,0.333333333333334,
0.333333333333334,0.333333333333334,0.333333333333334,0.333333333333334,
0.333333333333334,0.333333333333334,0.333333333333334,0.333333333333334,
0.333333333333334,0.333333333333334,0.333333333333334,0.333333333333334,
0.333333333333334,0.333333333333334,0.333333333333334,0.333333333333334,
0.333333333333334,0.333333333333334,0.333333333333334,0.333333333333334,
0.333333333333334,0.333333333333334,0.333333333333334,0.333333333333334,
0.333333333333334,0.333333333333334,0.333333333333334,0.333333333333334,
0.333333333333334,0.333333333333334,0.333333333333334,0.333333333333334,
0.333333333333334,0.333333333333334,0.333333333333334,0.333333333333334,
0.333333333333334,0.333333333333334,0.333333333333334,0.333333333333334,
0.333333333333334,0.333333333333334,0.333333333333334,0.333333333333334,
0.333333333333334,0.333333333333334,0.333333333333334,0.333333333333334,
0.333333333333334,0.333333333333334,0.333333333333334,0.333333333333334,
0.333333333333334,0.333333333333334,0.333333333333334,0.333333333333334,
0.333333333333334,0.333333333333334,0.333333333333334,0.333333333333334,
0.333333333333334,0.333333333333334,0.333333333333334,0.333333333333334,
0.333333333333334,0.333333333333334,0.333333333333334,0.333333333333334,
0.333333333333334,0.333333333333334,0.333333333333334,0.333333333333334,
0.333333333333334,0.333333333333334,0.333333333333334,0.333333333333334,
0.333333333333334,0.333333333333334,0.333333333333334,0.333333333333334,
0.333333333333334,0.333333333333334,0.333333333333334,0.333333333333334,
0.333333333333334,0.333333333333334,0.333333333333334,0.333333333333334,
0.333333333333334,0.333333333333334,0.333333333333334,0.333333333333334,
0.333333333333334,0.333333333333334,0.333333333333334,0.333333333333334,
0.333333333333334,0.333333333333334,0.333333333333334,0.333333333333334,
0.333333333333334,0.333333333333334,0.333333333333334,0.333333333333334,
0.333333333333334,0.333333333333334,0.333333333333334,0.333333333333334,
0.333333333333334,0.333333333333334,0.333333333333334,0.333333333333334,
0.333333333333334,0.333333333333334,0.333333333333334,0.333333333333334,
0.333333333333334,0.333333333333334,0.333333333333334,0.333333333333334,
0.333333333333334,0.333333333333334,0.333333333333334,0.333333333333334,
0.333333333333334,0.333333333333334,0.333333333333334,0.333333333333334,
0.333333333333334,0.333333333333334,0.333333333333334,0.333333333333334,
0.333333333333334,0.333333333333334,0.333333333333334,0.333333333333334,
0.333333333333334,0.333333333333334,0.333333333333334,0.333333333333334,
0.333333333333334),(1.,1.,1.,1.,1.,1.,1.,1.,1.,1.,1.,1.,1.,1.,1.,1.,1.,
1.,1.,1.,1.,1.,1.,1.,1.,1.,1.,1.,1.,1.,1.,1.,1.,1.,1.,1.,1.,1.,1.,1.,1.,
1.,1.,1.,1.,1.,1.,1.,1.,1.,1.,1.,1.,1.,1.,1.,1.,1.,1.,1.,1.,1.,1.,1.,1.,
1.,1.,1.,1.,1.,1.,1.,1.,1.,1.,1.,1.,1.,1.,1.,1.,1.,1.,1.,1.,1.,1.,1.,1.,
1.,1.,1.,1.,1.,1.,1.,1.,1.,1.,1.,1.,1.,1.,1.,1.,1.,1.,1.,1.,1.,1.,1.,1.,
1.,1.,1.,1.,1.,1.,1.,1.,1.,1.,1.,1.,1.,1.,1.,1.,1.,1.,1.,1.,1.,1.,1.,1.,
1.,1.,1.,1.,1.,1.,1.,1.,1.,1.,1.,1.,1.,1.,1.,1.,1.,1.,1.,1.,1.,1.,1.,1.,
1.,1.,1.,1.,1.,1.,1.,1.,1.,1.,1.,1.,1.,1.,1.,1.,1.,1.,1.,1.,1.,1.,1.,1.,
1.,1.,1.,1.,1.,1.,1.,1.,1.,1.,1.,1.,1.,1.,1.,1.,1.,1.,1.,1.,1.,1.,1.,1.,
1.,1.,1.,1.,1.,1.,1.,1.,1.,1.,1.,1.,1.,1.,1.,1.,1.,1.,1.,1.,1.,1.,1.,1.,
1.,1.,1.,1.,1.,1.,1.,1.,1.,1.,1.,1.,1.,1.,1.,1.,1.,1.,1.,1.,1.,1.,1.,1.,
1.,1.,1.,1.,1.,1.,1.,1.,1.,1.,1.,1.,1.,1.,1.,1.,1.,1.,1.,1.,1.,1.,1.,1.,
1.,1.,1.,1.,1.,1.,1.,1.,1.,1.,1.,1.,1.,1.,1.,1.,1.,1.,1.,1.,1.,1.,1.,1.,
1.,1.,1.,1.,1.)))
REPRESENTATION_ITEM('')
SURFACE()
);
#12675=(
BOUNDED_SURFACE()
B_SPLINE_SURFACE(1,2,((#31067,#31068,#31069,#31070,#31071,#31072,#31073,
#31074,#31075,#31076,#31077,#31078,#31079,#31080,#31081,#31082,#31083,#31084,
#31085,#31086,#31087,#31088,#31089,#31090,#31091,#31092,#31093,#31094,#31095,
#31096,#31097,#31098,#31099,#31100,#31101),(#31102,#31103,#31104,#31105,
#31106,#31107,#31108,#31109,#31110,#31111,#31112,#31113,#31114,#31115,#31116,
#31117,#31118,#31119,#31120,#31121,#31122,#31123,#31124,#31125,#31126,#31127,
#31128,#31129,#31130,#31131,#31132,#31133,#31134,#31135,#31136)),
 .RULED_SURF.,.F.,.F.,.F.)
B_SPLINE_SURFACE_WITH_KNOTS((2,2),(3,2,2,2,2,2,2,2,2,2,2,2,2,2,2,2,2,3),
(0.,1.),(0.,0.05,0.1,0.15,0.2,0.25,0.3,0.35,0.4,0.45,0.5,0.55,0.6,0.65,
0.7,0.75,0.8,0.826757087433802),.UNSPECIFIED.)
GEOMETRIC_REPRESENTATION_ITEM()
RATIONAL_B_SPLINE_SURFACE(((1.,0.951056516295154,1.,0.951056516295154,1.,
0.951056516295154,1.,0.951056516295154,1.,0.951056516295154,1.,0.951056516295154,
1.,0.951056516295154,1.,0.951056516295154,1.,0.951056516295154,1.,0.951056516295154,
1.,0.951056516295154,1.,0.951056516295154,1.,0.951056516295154,1.,0.951056516295154,
1.,0.951056516295154,1.,0.951056516295154,1.,0.973808298543891,0.975649142923828),
(1.,0.951056516295154,1.,0.951056516295154,1.,0.951056516295154,1.,0.951056516295154,
1.,0.951056516295154,1.,0.951056516295154,1.,0.951056516295154,1.,0.951056516295154,
1.,0.951056516295154,1.,0.951056516295154,1.,0.951056516295154,1.,0.951056516295154,
1.,0.951056516295154,1.,0.951056516295154,1.,0.951056516295154,1.,0.951056516295154,
1.,0.973808298543891,0.975649142923828)))
REPRESENTATION_ITEM('')
SURFACE()
);
#12676=(
BOUNDED_SURFACE()
B_SPLINE_SURFACE(3,2,((#31722,#31723,#31724,#31725,#31726,#31727,#31728,
#31729,#31730,#31731,#31732,#31733,#31734,#31735,#31736,#31737,#31738,#31739,
#31740,#31741,#31742,#31743,#31744,#31745,#31746,#31747,#31748,#31749,#31750,
#31751,#31752,#31753,#31754,#31755,#31756,#31757,#31758,#31759,#31760,#31761,
#31762,#31763,#31764,#31765,#31766,#31767,#31768,#31769,#31770,#31771,#31772,
#31773,#31774,#31775,#31776,#31777,#31778,#31779,#31780,#31781,#31782),
(#31783,#31784,#31785,#31786,#31787,#31788,#31789,#31790,#31791,#31792,
#31793,#31794,#31795,#31796,#31797,#31798,#31799,#31800,#31801,#31802,#31803,
#31804,#31805,#31806,#31807,#31808,#31809,#31810,#31811,#31812,#31813,#31814,
#31815,#31816,#31817,#31818,#31819,#31820,#31821,#31822,#31823,#31824,#31825,
#31826,#31827,#31828,#31829,#31830,#31831,#31832,#31833,#31834,#31835,#31836,
#31837,#31838,#31839,#31840,#31841,#31842,#31843),(#31844,#31845,#31846,
#31847,#31848,#31849,#31850,#31851,#31852,#31853,#31854,#31855,#31856,#31857,
#31858,#31859,#31860,#31861,#31862,#31863,#31864,#31865,#31866,#31867,#31868,
#31869,#31870,#31871,#31872,#31873,#31874,#31875,#31876,#31877,#31878,#31879,
#31880,#31881,#31882,#31883,#31884,#31885,#31886,#31887,#31888,#31889,#31890,
#31891,#31892,#31893,#31894,#31895,#31896,#31897,#31898,#31899,#31900,#31901,
#31902,#31903,#31904),(#31905,#31906,#31907,#31908,#31909,#31910,#31911,
#31912,#31913,#31914,#31915,#31916,#31917,#31918,#31919,#31920,#31921,#31922,
#31923,#31924,#31925,#31926,#31927,#31928,#31929,#31930,#31931,#31932,#31933,
#31934,#31935,#31936,#31937,#31938,#31939,#31940,#31941,#31942,#31943,#31944,
#31945,#31946,#31947,#31948,#31949,#31950,#31951,#31952,#31953,#31954,#31955,
#31956,#31957,#31958,#31959,#31960,#31961,#31962,#31963,#31964,#31965)),
 .UNSPECIFIED.,.F.,.F.,.F.)
B_SPLINE_SURFACE_WITH_KNOTS((4,4),(3,2,2,2,2,2,2,2,2,2,2,2,2,2,2,2,2,2,
2,2,2,2,2,2,2,2,2,2,2,2,3),(0.,1.),(0.,0.0277777777777778,0.0555555555555556,
0.0833333333333333,0.111111111111111,0.138888888888889,0.166666666666667,
0.194444444444445,0.222222222222222,0.25,0.277777777777778,0.305555555555555,
0.333333333333334,0.361111111111111,0.388888888888889,0.416666666666667,
0.444444444444444,0.472222222222222,0.5,0.527777777777778,0.555555555555556,
0.583333333333333,0.611111111111111,0.638888888888889,0.666666666666667,
0.694444444444444,0.722222222222222,0.75,0.777777777777778,0.805555555555556,
0.833333333333333),.PIECEWISE_BEZIER_KNOTS.)
GEOMETRIC_REPRESENTATION_ITEM()
RATIONAL_B_SPLINE_SURFACE(((1.,0.965925826289068,1.,0.965925826289068,1.,
0.965925826289068,1.,0.965925826289068,1.,0.965925826289068,1.,0.965925826289068,
1.,0.965925826289068,1.,0.965925826289068,1.,0.965925826289068,1.,0.965925826289068,
1.,0.965925826289068,1.,0.965925826289068,1.,0.965925826289068,1.,0.965925826289068,
1.,0.965925826289068,1.,0.965925826289068,1.,0.965925826289068,1.,0.965925826289068,
1.,0.965925826289068,1.,0.965925826289068,1.,0.965925826289068,1.,0.965925826289068,
1.,0.965925826289068,1.,0.965925826289068,1.,0.965925826289068,1.,0.965925826289068,
1.,0.965925826289068,1.,0.965925826289068,1.,0.965925826289068,1.,0.965925826289068,
1.),(0.949253021674191,0.916908009318038,0.949253021674191,0.916908009318038,
0.949253021674191,0.916908009318038,0.949253021674191,0.916908009318038,
0.949253021674191,0.916908009318038,0.949253021674191,0.916908009318038,
0.949253021674191,0.916908009318038,0.949253021674191,0.916908009318038,
0.949253021674191,0.916908009318038,0.949253021674191,0.916908009318038,
0.949253021674191,0.916908009318038,0.949253021674191,0.916908009318038,
0.949253021674191,0.916908009318038,0.949253021674191,0.916908009318038,
0.949253021674191,0.916908009318038,0.949253021674191,0.916908009318038,
0.949253021674191,0.916908009318038,0.949253021674191,0.916908009318038,
0.949253021674191,0.916908009318038,0.949253021674191,0.916908009318038,
0.949253021674191,0.916908009318038,0.949253021674191,0.916908009318038,
0.949253021674191,0.916908009318038,0.949253021674191,0.916908009318038,
0.949253021674191,0.916908009318038,0.949253021674191,0.916908009318038,
0.949253021674191,0.916908009318038,0.949253021674191,0.916908009318038,
0.949253021674191,0.916908009318038,0.949253021674191,0.916908009318038,
0.949253021674191),(0.949253021674191,0.916908009318038,0.949253021674191,
0.916908009318038,0.949253021674191,0.916908009318038,0.949253021674191,
0.916908009318038,0.949253021674191,0.916908009318038,0.949253021674191,
0.916908009318038,0.949253021674191,0.916908009318038,0.949253021674191,
0.916908009318038,0.949253021674191,0.916908009318038,0.949253021674191,
0.916908009318038,0.949253021674191,0.916908009318038,0.949253021674191,
0.916908009318038,0.949253021674191,0.916908009318038,0.949253021674191,
0.916908009318038,0.949253021674191,0.916908009318038,0.949253021674191,
0.916908009318038,0.949253021674191,0.916908009318038,0.949253021674191,
0.916908009318038,0.949253021674191,0.916908009318038,0.949253021674191,
0.916908009318038,0.949253021674191,0.916908009318038,0.949253021674191,
0.916908009318038,0.949253021674191,0.916908009318038,0.949253021674191,
0.916908009318038,0.949253021674191,0.916908009318038,0.949253021674191,
0.916908009318038,0.949253021674191,0.916908009318038,0.949253021674191,
0.916908009318038,0.949253021674191,0.916908009318038,0.949253021674191,
0.916908009318038,0.949253021674191),(1.,0.965925826289068,1.,0.965925826289068,
1.,0.965925826289068,1.,0.965925826289068,1.,0.965925826289068,1.,0.965925826289068,
1.,0.965925826289068,1.,0.965925826289068,1.,0.965925826289068,1.,0.965925826289068,
1.,0.965925826289068,1.,0.965925826289068,1.,0.965925826289068,1.,0.965925826289068,
1.,0.965925826289068,1.,0.965925826289068,1.,0.965925826289068,1.,0.965925826289068,
1.,0.965925826289068,1.,0.965925826289068,1.,0.965925826289068,1.,0.965925826289068,
1.,0.965925826289068,1.,0.965925826289068,1.,0.965925826289068,1.,0.965925826289068,
1.,0.965925826289068,1.,0.965925826289068,1.,0.965925826289068,1.,0.965925826289068,
1.)))
REPRESENTATION_ITEM('')
SURFACE()
);
#12677=(
BOUNDED_SURFACE()
B_SPLINE_SURFACE(1,2,((#32102,#32103,#32104,#32105,#32106,#32107,#32108,
#32109,#32110,#32111,#32112,#32113,#32114,#32115,#32116,#32117,#32118,#32119,
#32120,#32121,#32122,#32123,#32124,#32125,#32126,#32127,#32128,#32129,#32130,
#32131,#32132,#32133,#32134,#32135,#32136,#32137,#32138,#32139,#32140,#32141,
#32142,#32143,#32144,#32145,#32146,#32147,#32148,#32149,#32150,#32151,#32152,
#32153,#32154,#32155,#32156,#32157,#32158,#32159,#32160,#32161,#32162),
(#32163,#32164,#32165,#32166,#32167,#32168,#32169,#32170,#32171,#32172,
#32173,#32174,#32175,#32176,#32177,#32178,#32179,#32180,#32181,#32182,#32183,
#32184,#32185,#32186,#32187,#32188,#32189,#32190,#32191,#32192,#32193,#32194,
#32195,#32196,#32197,#32198,#32199,#32200,#32201,#32202,#32203,#32204,#32205,
#32206,#32207,#32208,#32209,#32210,#32211,#32212,#32213,#32214,#32215,#32216,
#32217,#32218,#32219,#32220,#32221,#32222,#32223)),.RULED_SURF.,.F.,.F.,
 .F.)
B_SPLINE_SURFACE_WITH_KNOTS((2,2),(3,2,2,2,2,2,2,2,2,2,2,2,2,2,2,2,2,2,
2,2,2,2,2,2,2,2,2,2,2,2,3),(0.,1.),(0.,0.0277777777777778,0.0555555555555556,
0.0833333333333333,0.111111111111111,0.138888888888889,0.166666666666667,
0.194444444444445,0.222222222222222,0.25,0.277777777777778,0.305555555555555,
0.333333333333334,0.361111111111111,0.388888888888889,0.416666666666667,
0.444444444444444,0.472222222222222,0.5,0.527777777777778,0.555555555555556,
0.583333333333333,0.611111111111111,0.638888888888889,0.666666666666667,
0.694444444444444,0.722222222222222,0.75,0.777777777777778,0.805555555555556,
0.833333333333333),.UNSPECIFIED.)
GEOMETRIC_REPRESENTATION_ITEM()
RATIONAL_B_SPLINE_SURFACE(((1.,0.965925826289068,1.,0.965925826289068,1.,
0.965925826289068,1.,0.965925826289068,1.,0.965925826289068,1.,0.965925826289068,
1.,0.965925826289068,1.,0.965925826289068,1.,0.965925826289068,1.,0.965925826289068,
1.,0.965925826289068,1.,0.965925826289068,1.,0.965925826289068,1.,0.965925826289068,
1.,0.965925826289068,1.,0.965925826289068,1.,0.965925826289068,1.,0.965925826289068,
1.,0.965925826289068,1.,0.965925826289068,1.,0.965925826289068,1.,0.965925826289068,
1.,0.965925826289068,1.,0.965925826289068,1.,0.965925826289068,1.,0.965925826289068,
1.,0.965925826289068,1.,0.965925826289068,1.,0.965925826289068,1.,0.965925826289068,
1.),(1.,0.965925826289068,1.,0.965925826289068,1.,0.965925826289068,1.,
0.965925826289068,1.,0.965925826289068,1.,0.965925826289068,1.,0.965925826289068,
1.,0.965925826289068,1.,0.965925826289068,1.,0.965925826289068,1.,0.965925826289068,
1.,0.965925826289068,1.,0.965925826289068,1.,0.965925826289068,1.,0.965925826289068,
1.,0.965925826289068,1.,0.965925826289068,1.,0.965925826289068,1.,0.965925826289068,
1.,0.965925826289068,1.,0.965925826289068,1.,0.965925826289068,1.,0.965925826289068,
1.,0.965925826289068,1.,0.965925826289068,1.,0.965925826289068,1.,0.965925826289068,
1.,0.965925826289068,1.,0.965925826289068,1.,0.965925826289068,1.)))
REPRESENTATION_ITEM('')
SURFACE()
);
#12678=(
BOUNDED_SURFACE()
B_SPLINE_SURFACE(3,2,((#32292,#32293,#32294,#32295,#32296,#32297,#32298,
#32299,#32300,#32301,#32302,#32303,#32304,#32305,#32306,#32307,#32308,#32309,
#32310,#32311,#32312,#32313,#32314,#32315,#32316,#32317,#32318,#32319,#32320,
#32321,#32322,#32323,#32324,#32325,#32326,#32327,#32328,#32329,#32330,#32331,
#32332,#32333,#32334,#32335,#32336,#32337,#32338,#32339,#32340,#32341,#32342,
#32343,#32344,#32345,#32346,#32347,#32348,#32349,#32350),(#32351,#32352,
#32353,#32354,#32355,#32356,#32357,#32358,#32359,#32360,#32361,#32362,#32363,
#32364,#32365,#32366,#32367,#32368,#32369,#32370,#32371,#32372,#32373,#32374,
#32375,#32376,#32377,#32378,#32379,#32380,#32381,#32382,#32383,#32384,#32385,
#32386,#32387,#32388,#32389,#32390,#32391,#32392,#32393,#32394,#32395,#32396,
#32397,#32398,#32399,#32400,#32401,#32402,#32403,#32404,#32405,#32406,#32407,
#32408,#32409),(#32410,#32411,#32412,#32413,#32414,#32415,#32416,#32417,
#32418,#32419,#32420,#32421,#32422,#32423,#32424,#32425,#32426,#32427,#32428,
#32429,#32430,#32431,#32432,#32433,#32434,#32435,#32436,#32437,#32438,#32439,
#32440,#32441,#32442,#32443,#32444,#32445,#32446,#32447,#32448,#32449,#32450,
#32451,#32452,#32453,#32454,#32455,#32456,#32457,#32458,#32459,#32460,#32461,
#32462,#32463,#32464,#32465,#32466,#32467,#32468),(#32469,#32470,#32471,
#32472,#32473,#32474,#32475,#32476,#32477,#32478,#32479,#32480,#32481,#32482,
#32483,#32484,#32485,#32486,#32487,#32488,#32489,#32490,#32491,#32492,#32493,
#32494,#32495,#32496,#32497,#32498,#32499,#32500,#32501,#32502,#32503,#32504,
#32505,#32506,#32507,#32508,#32509,#32510,#32511,#32512,#32513,#32514,#32515,
#32516,#32517,#32518,#32519,#32520,#32521,#32522,#32523,#32524,#32525,#32526,
#32527)),.UNSPECIFIED.,.F.,.F.,.F.)
B_SPLINE_SURFACE_WITH_KNOTS((4,4),(3,2,2,2,2,2,2,2,2,2,2,2,2,2,2,2,2,2,
2,2,2,2,2,2,2,2,2,2,2,3),(0.,1.),(0.,0.0277777777777778,0.0555555555555556,
0.0833333333333333,0.111111111111111,0.138888888888889,0.166666666666667,
0.194444444444445,0.222222222222222,0.25,0.277777777777778,0.305555555555555,
0.333333333333334,0.361111111111111,0.388888888888889,0.416666666666667,
0.444444444444444,0.472222222222222,0.5,0.527777777777778,0.555555555555556,
0.583333333333333,0.611111111111111,0.638888888888889,0.666666666666667,
0.694444444444444,0.722222222222222,0.75,0.777777777777778,0.796430048543053),
 .PIECEWISE_BEZIER_KNOTS.)
GEOMETRIC_REPRESENTATION_ITEM()
RATIONAL_B_SPLINE_SURFACE(((1.,0.965925826289068,1.,0.965925826289068,1.,
0.965925826289068,1.,0.965925826289068,1.,0.965925826289068,1.,0.965925826289068,
1.,0.965925826289068,1.,0.965925826289068,1.,0.965925826289068,1.,0.965925826289068,
1.,0.965925826289068,1.,0.965925826289068,1.,0.965925826289068,1.,0.965925826289068,
1.,0.965925826289068,1.,0.965925826289068,1.,0.965925826289068,1.,0.965925826289068,
1.,0.965925826289068,1.,0.965925826289068,1.,0.965925826289068,1.,0.965925826289068,
1.,0.965925826289068,1.,0.965925826289068,1.,0.965925826289068,1.,0.965925826289068,
1.,0.965925826289068,1.,0.965925826289068,1.,0.977119814290265,0.984966882749808),
(0.949253021674191,0.916908009318038,0.949253021674191,0.916908009318038,
0.949253021674191,0.916908009318038,0.949253021674191,0.916908009318038,
0.949253021674191,0.916908009318038,0.949253021674191,0.916908009318038,
0.949253021674191,0.916908009318038,0.949253021674191,0.916908009318038,
0.949253021674191,0.916908009318038,0.949253021674191,0.916908009318038,
0.949253021674191,0.916908009318038,0.949253021674191,0.916908009318038,
0.949253021674191,0.916908009318038,0.949253021674191,0.916908009318038,
0.949253021674191,0.916908009318038,0.949253021674191,0.916908009318038,
0.949253021674191,0.916908009318038,0.949253021674191,0.916908009318038,
0.949253021674191,0.916908009318038,0.949253021674191,0.916908009318038,
0.949253021674191,0.916908009318038,0.949253021674191,0.916908009318038,
0.949253021674191,0.916908009318038,0.949253021674191,0.916908009318038,
0.949253021674191,0.916908009318038,0.949253021674191,0.916908009318038,
0.949253021674191,0.916908009318038,0.949253021674191,0.916908009318038,
0.949253021674191,0.927533936252759,0.934982789699264),(0.949253021674191,
0.916908009318038,0.949253021674191,0.916908009318038,0.949253021674191,
0.916908009318038,0.949253021674191,0.916908009318038,0.949253021674191,
0.916908009318038,0.949253021674191,0.916908009318038,0.949253021674191,
0.916908009318038,0.949253021674191,0.916908009318038,0.949253021674191,
0.916908009318038,0.949253021674191,0.916908009318038,0.949253021674191,
0.916908009318038,0.949253021674191,0.916908009318038,0.949253021674191,
0.916908009318038,0.949253021674191,0.916908009318038,0.949253021674191,
0.916908009318038,0.949253021674191,0.916908009318038,0.949253021674191,
0.916908009318038,0.949253021674191,0.916908009318038,0.949253021674191,
0.916908009318038,0.949253021674191,0.916908009318038,0.949253021674191,
0.916908009318038,0.949253021674191,0.916908009318038,0.949253021674191,
0.916908009318038,0.949253021674191,0.916908009318038,0.949253021674191,
0.916908009318038,0.949253021674191,0.916908009318038,0.949253021674191,
0.916908009318038,0.949253021674191,0.916908009318038,0.949253021674191,
0.927533936252759,0.934982789699264),(1.,0.965925826289068,1.,0.965925826289068,
1.,0.965925826289068,1.,0.965925826289068,1.,0.965925826289068,1.,0.965925826289068,
1.,0.965925826289068,1.,0.965925826289068,1.,0.965925826289068,1.,0.965925826289068,
1.,0.965925826289068,1.,0.965925826289068,1.,0.965925826289068,1.,0.965925826289068,
1.,0.965925826289068,1.,0.965925826289068,1.,0.965925826289068,1.,0.965925826289068,
1.,0.965925826289068,1.,0.965925826289068,1.,0.965925826289068,1.,0.965925826289068,
1.,0.965925826289068,1.,0.965925826289068,1.,0.965925826289068,1.,0.965925826289068,
1.,0.965925826289068,1.,0.965925826289068,1.,0.977119814290265,0.984966882749808)))
REPRESENTATION_ITEM('')
SURFACE()
);
#12679=(
BOUNDED_SURFACE()
B_SPLINE_SURFACE(3,2,((#32672,#32673,#32674,#32675,#32676,#32677,#32678,
#32679,#32680,#32681,#32682,#32683,#32684,#32685,#32686,#32687,#32688,#32689,
#32690,#32691,#32692,#32693,#32694,#32695,#32696,#32697,#32698,#32699,#32700,
#32701,#32702,#32703,#32704,#32705,#32706,#32707,#32708,#32709,#32710,#32711,
#32712,#32713,#32714,#32715,#32716,#32717,#32718,#32719,#32720,#32721,#32722,
#32723,#32724),(#32725,#32726,#32727,#32728,#32729,#32730,#32731,#32732,
#32733,#32734,#32735,#32736,#32737,#32738,#32739,#32740,#32741,#32742,#32743,
#32744,#32745,#32746,#32747,#32748,#32749,#32750,#32751,#32752,#32753,#32754,
#32755,#32756,#32757,#32758,#32759,#32760,#32761,#32762,#32763,#32764,#32765,
#32766,#32767,#32768,#32769,#32770,#32771,#32772,#32773,#32774,#32775,#32776,
#32777),(#32778,#32779,#32780,#32781,#32782,#32783,#32784,#32785,#32786,
#32787,#32788,#32789,#32790,#32791,#32792,#32793,#32794,#32795,#32796,#32797,
#32798,#32799,#32800,#32801,#32802,#32803,#32804,#32805,#32806,#32807,#32808,
#32809,#32810,#32811,#32812,#32813,#32814,#32815,#32816,#32817,#32818,#32819,
#32820,#32821,#32822,#32823,#32824,#32825,#32826,#32827,#32828,#32829,#32830),
(#32831,#32832,#32833,#32834,#32835,#32836,#32837,#32838,#32839,#32840,
#32841,#32842,#32843,#32844,#32845,#32846,#32847,#32848,#32849,#32850,#32851,
#32852,#32853,#32854,#32855,#32856,#32857,#32858,#32859,#32860,#32861,#32862,
#32863,#32864,#32865,#32866,#32867,#32868,#32869,#32870,#32871,#32872,#32873,
#32874,#32875,#32876,#32877,#32878,#32879,#32880,#32881,#32882,#32883)),
 .UNSPECIFIED.,.F.,.F.,.F.)
B_SPLINE_SURFACE_WITH_KNOTS((4,4),(3,2,2,2,2,2,2,2,2,2,2,2,2,2,2,2,2,2,
2,2,2,2,2,2,2,2,3),(0.,1.),(0.,0.0277777777777778,0.0555555555555556,0.0833333333333333,
0.111111111111111,0.138888888888889,0.166666666666667,0.194444444444445,
0.222222222222222,0.25,0.277777777777778,0.305555555555555,0.333333333333334,
0.361111111111111,0.388888888888889,0.416666666666667,0.444444444444444,
0.472222222222222,0.5,0.527777777777778,0.555555555555556,0.583333333333333,
0.611111111111111,0.638888888888889,0.666666666666667,0.694444444444444,
0.702647985953411),.PIECEWISE_BEZIER_KNOTS.)
GEOMETRIC_REPRESENTATION_ITEM()
RATIONAL_B_SPLINE_SURFACE(((1.,0.965925826289068,1.,0.965925826289068,1.,
0.965925826289068,1.,0.965925826289068,1.,0.965925826289068,1.,0.965925826289068,
1.,0.965925826289068,1.,0.965925826289068,1.,0.965925826289068,1.,0.965925826289068,
1.,0.965925826289068,1.,0.965925826289068,1.,0.965925826289068,1.,0.965925826289068,
1.,0.965925826289068,1.,0.965925826289068,1.,0.965925826289068,1.,0.965925826289068,
1.,0.965925826289068,1.,0.965925826289068,1.,0.965925826289068,1.,0.965925826289068,
1.,0.965925826289068,1.,0.965925826289068,1.,0.965925826289068,1.,0.98993695965683,
0.985817704293295),(0.844029628745982,0.815270016558918,0.844029628745982,
0.815270016558918,0.844029628745982,0.815270016558918,0.844029628745982,
0.815270016558918,0.844029628745982,0.815270016558918,0.844029628745982,
0.815270016558918,0.844029628745982,0.815270016558918,0.844029628745982,
0.815270016558918,0.844029628745982,0.815270016558918,0.844029628745982,
0.815270016558918,0.844029628745982,0.815270016558918,0.844029628745982,
0.815270016558918,0.844029628745982,0.815270016558918,0.844029628745982,
0.815270016558918,0.844029628745982,0.815270016558918,0.844029628745982,
0.815270016558918,0.844029628745982,0.815270016558918,0.844029628745982,
0.815270016558918,0.844029628745982,0.815270016558918,0.844029628745982,
0.815270016558918,0.844029628745982,0.815270016558918,0.844029628745982,
0.815270016558918,0.844029628745982,0.815270016558918,0.844029628745982,
0.815270016558918,0.844029628745982,0.815270016558918,0.844029628745982,
0.83553612454108,0.832059350965886),(0.844029628745982,0.815270016558918,
0.844029628745982,0.815270016558918,0.844029628745982,0.815270016558918,
0.844029628745982,0.815270016558918,0.844029628745982,0.815270016558918,
0.844029628745982,0.815270016558918,0.844029628745982,0.815270016558918,
0.844029628745982,0.815270016558918,0.844029628745982,0.815270016558918,
0.844029628745982,0.815270016558918,0.844029628745982,0.815270016558918,
0.844029628745982,0.815270016558918,0.844029628745982,0.815270016558918,
0.844029628745982,0.815270016558918,0.844029628745982,0.815270016558918,
0.844029628745982,0.815270016558918,0.844029628745982,0.815270016558918,
0.844029628745982,0.815270016558918,0.844029628745982,0.815270016558918,
0.844029628745982,0.815270016558918,0.844029628745982,0.815270016558918,
0.844029628745982,0.815270016558918,0.844029628745982,0.815270016558918,
0.844029628745982,0.815270016558918,0.844029628745982,0.815270016558918,
0.844029628745982,0.83553612454108,0.832059350965886),(1.,0.965925826289068,
1.,0.965925826289068,1.,0.965925826289068,1.,0.965925826289068,1.,0.965925826289068,
1.,0.965925826289068,1.,0.965925826289068,1.,0.965925826289068,1.,0.965925826289068,
1.,0.965925826289068,1.,0.965925826289068,1.,0.965925826289068,1.,0.965925826289068,
1.,0.965925826289068,1.,0.965925826289068,1.,0.965925826289068,1.,0.965925826289068,
1.,0.965925826289068,1.,0.965925826289068,1.,0.965925826289068,1.,0.965925826289068,
1.,0.965925826289068,1.,0.965925826289068,1.,0.965925826289068,1.,0.965925826289068,
1.,0.98993695965683,0.985817704293295)))
REPRESENTATION_ITEM('')
SURFACE()
);
#12680=(
BOUNDED_SURFACE()
B_SPLINE_SURFACE(1,2,((#32944,#32945,#32946,#32947,#32948,#32949,#32950,
#32951,#32952,#32953,#32954,#32955,#32956,#32957,#32958,#32959,#32960,#32961,
#32962,#32963,#32964,#32965,#32966,#32967,#32968,#32969,#32970,#32971,#32972,
#32973,#32974,#32975,#32976,#32977,#32978,#32979,#32980,#32981,#32982,#32983,
#32984,#32985,#32986,#32987,#32988,#32989,#32990,#32991,#32992,#32993,#32994),
(#32995,#32996,#32997,#32998,#32999,#33000,#33001,#33002,#33003,#33004,
#33005,#33006,#33007,#33008,#33009,#33010,#33011,#33012,#33013,#33014,#33015,
#33016,#33017,#33018,#33019,#33020,#33021,#33022,#33023,#33024,#33025,#33026,
#33027,#33028,#33029,#33030,#33031,#33032,#33033,#33034,#33035,#33036,#33037,
#33038,#33039,#33040,#33041,#33042,#33043,#33044,#33045)),.RULED_SURF.,
 .F.,.F.,.F.)
B_SPLINE_SURFACE_WITH_KNOTS((2,2),(3,2,2,2,2,2,2,2,2,2,2,2,2,2,2,2,2,2,
2,2,2,2,2,2,2,3),(0.,1.),(0.,0.0277777777777778,0.0555555555555556,0.0833333333333333,
0.111111111111111,0.138888888888889,0.166666666666667,0.194444444444445,
0.222222222222222,0.25,0.277777777777778,0.305555555555555,0.333333333333334,
0.361111111111111,0.388888888888889,0.416666666666667,0.444444444444444,
0.472222222222222,0.5,0.527777777777778,0.555555555555556,0.583333333333333,
0.611111111111111,0.638888888888889,0.666666666666667,0.67623687285605),
 .PIECEWISE_BEZIER_KNOTS.)
GEOMETRIC_REPRESENTATION_ITEM()
RATIONAL_B_SPLINE_SURFACE(((1.,0.965925826289068,1.,0.965925826289068,1.,
0.965925826289068,1.,0.965925826289068,1.,0.965925826289068,1.,0.965925826289068,
1.,0.965925826289068,1.,0.965925826289068,1.,0.965925826289068,1.,0.965925826289068,
1.,0.965925826289068,1.,0.965925826289068,1.,0.965925826289068,1.,0.965925826289068,
1.,0.965925826289068,1.,0.965925826289068,1.,0.965925826289068,1.,0.965925826289068,
1.,0.965925826289068,1.,0.965925826289068,1.,0.965925826289068,1.,0.965925826289068,
1.,0.965925826289068,1.,0.965925826289068,1.,0.988260512746727,0.984610176070599),
(1.,0.965925826289068,1.,0.965925826289068,1.,0.965925826289068,1.,0.965925826289068,
1.,0.965925826289068,1.,0.965925826289068,1.,0.965925826289068,1.,0.965925826289068,
1.,0.965925826289068,1.,0.965925826289068,1.,0.965925826289068,1.,0.965925826289068,
1.,0.965925826289068,1.,0.965925826289068,1.,0.965925826289068,1.,0.965925826289068,
1.,0.965925826289068,1.,0.965925826289068,1.,0.965925826289068,1.,0.965925826289068,
1.,0.965925826289068,1.,0.965925826289068,1.,0.965925826289068,1.,0.965925826289068,
1.,0.988260512746727,0.984610176070599)))
REPRESENTATION_ITEM('')
SURFACE()
);
#12681=(
BOUNDED_SURFACE()
B_SPLINE_SURFACE(3,2,((#33100,#33101,#33102,#33103,#33104,#33105,#33106,
#33107,#33108,#33109,#33110,#33111,#33112,#33113,#33114,#33115,#33116,#33117,
#33118,#33119,#33120,#33121,#33122,#33123,#33124,#33125,#33126,#33127,#33128,
#33129,#33130,#33131,#33132,#33133,#33134,#33135,#33136,#33137,#33138,#33139,
#33140,#33141,#33142,#33143,#33144,#33145,#33146,#33147,#33148),(#33149,
#33150,#33151,#33152,#33153,#33154,#33155,#33156,#33157,#33158,#33159,#33160,
#33161,#33162,#33163,#33164,#33165,#33166,#33167,#33168,#33169,#33170,#33171,
#33172,#33173,#33174,#33175,#33176,#33177,#33178,#33179,#33180,#33181,#33182,
#33183,#33184,#33185,#33186,#33187,#33188,#33189,#33190,#33191,#33192,#33193,
#33194,#33195,#33196,#33197),(#33198,#33199,#33200,#33201,#33202,#33203,
#33204,#33205,#33206,#33207,#33208,#33209,#33210,#33211,#33212,#33213,#33214,
#33215,#33216,#33217,#33218,#33219,#33220,#33221,#33222,#33223,#33224,#33225,
#33226,#33227,#33228,#33229,#33230,#33231,#33232,#33233,#33234,#33235,#33236,
#33237,#33238,#33239,#33240,#33241,#33242,#33243,#33244,#33245,#33246),
(#33247,#33248,#33249,#33250,#33251,#33252,#33253,#33254,#33255,#33256,
#33257,#33258,#33259,#33260,#33261,#33262,#33263,#33264,#33265,#33266,#33267,
#33268,#33269,#33270,#33271,#33272,#33273,#33274,#33275,#33276,#33277,#33278,
#33279,#33280,#33281,#33282,#33283,#33284,#33285,#33286,#33287,#33288,#33289,
#33290,#33291,#33292,#33293,#33294,#33295)),.UNSPECIFIED.,.F.,.F.,.F.)
B_SPLINE_SURFACE_WITH_KNOTS((4,4),(3,2,2,2,2,2,2,2,2,2,2,2,2,2,2,2,2,2,
2,2,2,2,2,2,3),(0.,1.),(0.,0.0277777777777778,0.0555555555555556,0.0833333333333333,
0.111111111111111,0.138888888888889,0.166666666666667,0.194444444444445,
0.222222222222222,0.25,0.277777777777778,0.305555555555555,0.333333333333334,
0.361111111111111,0.388888888888889,0.416666666666667,0.444444444444444,
0.472222222222222,0.5,0.527777777777778,0.555555555555556,0.583333333333333,
0.611111111111111,0.638888888888889,0.664003515027687),
 .PIECEWISE_BEZIER_KNOTS.)
GEOMETRIC_REPRESENTATION_ITEM()
RATIONAL_B_SPLINE_SURFACE(((1.,0.965925826289068,1.,0.965925826289068,1.,
0.965925826289068,1.,0.965925826289068,1.,0.965925826289068,1.,0.965925826289068,
1.,0.965925826289068,1.,0.965925826289068,1.,0.965925826289068,1.,0.965925826289068,
1.,0.965925826289068,1.,0.965925826289068,1.,0.965925826289068,1.,0.965925826289068,
1.,0.965925826289068,1.,0.965925826289068,1.,0.965925826289068,1.,0.965925826289068,
1.,0.965925826289068,1.,0.965925826289068,1.,0.965925826289068,1.,0.965925826289068,
1.,0.965925826289068,1.,0.969192635185413,0.9940927827449),(0.844029628745984,
0.81527001655892,0.844029628745984,0.81527001655892,0.844029628745984,0.81527001655892,
0.844029628745984,0.81527001655892,0.844029628745984,0.81527001655892,0.844029628745984,
0.81527001655892,0.844029628745984,0.81527001655892,0.844029628745984,0.81527001655892,
0.844029628745984,0.81527001655892,0.844029628745984,0.81527001655892,0.844029628745984,
0.81527001655892,0.844029628745984,0.81527001655892,0.844029628745984,0.81527001655892,
0.844029628745984,0.81527001655892,0.844029628745984,0.81527001655892,0.844029628745984,
0.81527001655892,0.844029628745984,0.81527001655892,0.844029628745984,0.81527001655892,
0.844029628745984,0.81527001655892,0.844029628745984,0.81527001655892,0.844029628745984,
0.81527001655892,0.844029628745984,0.81527001655892,0.844029628745984,0.81527001655892,
0.844029628745984,0.818027300058886,0.83904376235924),(0.844029628745984,
0.81527001655892,0.844029628745984,0.81527001655892,0.844029628745984,0.81527001655892,
0.844029628745984,0.81527001655892,0.844029628745984,0.81527001655892,0.844029628745984,
0.81527001655892,0.844029628745984,0.81527001655892,0.844029628745984,0.81527001655892,
0.844029628745984,0.81527001655892,0.844029628745984,0.81527001655892,0.844029628745984,
0.81527001655892,0.844029628745984,0.81527001655892,0.844029628745984,0.81527001655892,
0.844029628745984,0.81527001655892,0.844029628745984,0.81527001655892,0.844029628745984,
0.81527001655892,0.844029628745984,0.81527001655892,0.844029628745984,0.81527001655892,
0.844029628745984,0.81527001655892,0.844029628745984,0.81527001655892,0.844029628745984,
0.81527001655892,0.844029628745984,0.81527001655892,0.844029628745984,0.81527001655892,
0.844029628745984,0.818027300058886,0.83904376235924),(1.,0.965925826289068,
1.,0.965925826289068,1.,0.965925826289068,1.,0.965925826289068,1.,0.965925826289068,
1.,0.965925826289068,1.,0.965925826289068,1.,0.965925826289068,1.,0.965925826289068,
1.,0.965925826289068,1.,0.965925826289068,1.,0.965925826289068,1.,0.965925826289068,
1.,0.965925826289068,1.,0.965925826289068,1.,0.965925826289068,1.,0.965925826289068,
1.,0.965925826289068,1.,0.965925826289068,1.,0.965925826289068,1.,0.965925826289068,
1.,0.965925826289068,1.,0.965925826289068,1.,0.969192635185413,0.9940927827449)))
REPRESENTATION_ITEM('')
SURFACE()
);
#12682=(
BOUNDED_SURFACE()
B_SPLINE_SURFACE(3,2,((#33370,#33371,#33372,#33373,#33374,#33375,#33376),
(#33377,#33378,#33379,#33380,#33381,#33382,#33383),(#33384,#33385,#33386,
#33387,#33388,#33389,#33390),(#33391,#33392,#33393,#33394,#33395,#33396,
#33397)),.UNSPECIFIED.,.F.,.F.,.F.)
B_SPLINE_SURFACE_WITH_KNOTS((4,4),(3,2,2,3),(0.,1.),(0.769890375742853,
0.777777777777778,0.805555555555556,0.833333333333333),
 .PIECEWISE_BEZIER_KNOTS.)
GEOMETRIC_REPRESENTATION_ITEM()
RATIONAL_B_SPLINE_SURFACE(((0.986144018469014,0.990324758545624,1.,0.965925826289068,
1.,0.965925826289068,1.),(0.832334769798475,0.83586343829322,0.844029628745984,
0.81527001655892,0.844029628745984,0.81527001655892,0.844029628745984),
(0.832334769798475,0.83586343829322,0.844029628745984,0.81527001655892,
0.844029628745984,0.81527001655892,0.844029628745984),(0.986144018469014,
0.990324758545624,1.,0.965925826289068,1.,0.965925826289068,1.)))
REPRESENTATION_ITEM('')
SURFACE()
);
#12683=(
BOUNDED_SURFACE()
B_SPLINE_SURFACE(3,2,((#33450,#33451,#33452),(#33453,#33454,#33455),(#33456,
#33457,#33458),(#33459,#33460,#33461)),.UNSPECIFIED.,.F.,.F.,.F.)
B_SPLINE_SURFACE_WITH_KNOTS((4,4),(3,3),(0.0382659980764476,1.),(0.808520334142405,
0.833333333333333),.PIECEWISE_BEZIER_KNOTS.)
GEOMETRIC_REPRESENTATION_ITEM()
RATIONAL_B_SPLINE_SURFACE(((0.976394668876932,0.952866831529329,0.982780070198817),
(0.83877262990258,0.818561022202317,0.844258014071977),(0.844475312244286,
0.824126289022556,0.849997990672371),(0.99350271590205,0.969562631990048,
1.)))
REPRESENTATION_ITEM('')
SURFACE()
);
#12684=(
BOUNDED_SURFACE()
B_SPLINE_SURFACE(1,2,((#33568,#33569,#33570,#33571,#33572,#33573,#33574,
#33575,#33576,#33577,#33578,#33579,#33580,#33581,#33582,#33583,#33584,#33585,
#33586,#33587,#33588,#33589,#33590,#33591,#33592,#33593,#33594,#33595,#33596,
#33597,#33598,#33599,#33600,#33601,#33602,#33603,#33604,#33605,#33606,#33607,
#33608,#33609,#33610,#33611,#33612,#33613,#33614,#33615,#33616,#33617,#33618,
#33619,#33620,#33621,#33622,#33623,#33624),(#33625,#33626,#33627,#33628,
#33629,#33630,#33631,#33632,#33633,#33634,#33635,#33636,#33637,#33638,#33639,
#33640,#33641,#33642,#33643,#33644,#33645,#33646,#33647,#33648,#33649,#33650,
#33651,#33652,#33653,#33654,#33655,#33656,#33657,#33658,#33659,#33660,#33661,
#33662,#33663,#33664,#33665,#33666,#33667,#33668,#33669,#33670,#33671,#33672,
#33673,#33674,#33675,#33676,#33677,#33678,#33679,#33680,#33681)),
 .RULED_SURF.,.F.,.F.,.F.)
B_SPLINE_SURFACE_WITH_KNOTS((2,2),(3,2,2,2,2,2,2,2,2,2,2,2,2,2,2,2,2,2,
2,2,2,2,2,2,2,2,2,2,3),(0.,1.),(0.,0.03125,0.0625,0.09375,0.125,0.15625,
0.1875,0.21875,0.25,0.28125,0.3125,0.34375,0.375,0.40625,0.4375,0.46875,
0.5,0.53125,0.5625,0.59375,0.625,0.65625,0.6875,0.71875,0.75,0.78125,0.8125,
0.84375,0.875),.UNSPECIFIED.)
GEOMETRIC_REPRESENTATION_ITEM()
RATIONAL_B_SPLINE_SURFACE(((1.,0.923879532511287,1.,0.923879532511287,1.,
0.923879532511287,1.,0.923879532511287,1.,0.923879532511287,1.,0.923879532511287,
1.,0.923879532511287,1.,0.923879532511287,1.,0.923879532511287,1.,0.923879532511287,
1.,0.923879532511287,1.,0.923879532511287,1.,0.923879532511287,1.,0.923879532511287,
1.,0.923879532511287,1.,0.923879532511287,1.,0.923879532511287,1.,0.923879532511287,
1.,0.923879532511287,1.,0.923879532511287,1.,0.923879532511287,1.,0.923879532511287,
1.,0.923879532511287,1.,0.923879532511287,1.,0.923879532511287,1.,0.923879532511287,
1.,0.923879532511287,1.,0.923879532511287,1.),(1.,0.923879532511287,1.,
0.923879532511287,1.,0.923879532511287,1.,0.923879532511287,1.,0.923879532511287,
1.,0.923879532511287,1.,0.923879532511287,1.,0.923879532511287,1.,0.923879532511287,
1.,0.923879532511287,1.,0.923879532511287,1.,0.923879532511287,1.,0.923879532511287,
1.,0.923879532511287,1.,0.923879532511287,1.,0.923879532511287,1.,0.923879532511287,
1.,0.923879532511287,1.,0.923879532511287,1.,0.923879532511287,1.,0.923879532511287,
1.,0.923879532511287,1.,0.923879532511287,1.,0.923879532511287,1.,0.923879532511287,
1.,0.923879532511287,1.,0.923879532511287,1.,0.923879532511287,1.)))
REPRESENTATION_ITEM('')
SURFACE()
);
#12685=(
BOUNDED_SURFACE()
B_SPLINE_SURFACE(1,2,((#33816,#33817,#33818,#33819,#33820,#33821,#33822,
#33823,#33824,#33825,#33826,#33827,#33828,#33829,#33830,#33831,#33832,#33833,
#33834,#33835,#33836,#33837,#33838,#33839,#33840,#33841,#33842,#33843,#33844,
#33845,#33846,#33847,#33848,#33849,#33850,#33851,#33852,#33853,#33854,#33855,
#33856,#33857,#33858,#33859,#33860,#33861,#33862,#33863,#33864,#33865,#33866,
#33867,#33868,#33869,#33870,#33871,#33872),(#33873,#33874,#33875,#33876,
#33877,#33878,#33879,#33880,#33881,#33882,#33883,#33884,#33885,#33886,#33887,
#33888,#33889,#33890,#33891,#33892,#33893,#33894,#33895,#33896,#33897,#33898,
#33899,#33900,#33901,#33902,#33903,#33904,#33905,#33906,#33907,#33908,#33909,
#33910,#33911,#33912,#33913,#33914,#33915,#33916,#33917,#33918,#33919,#33920,
#33921,#33922,#33923,#33924,#33925,#33926,#33927,#33928,#33929)),
 .RULED_SURF.,.F.,.F.,.F.)
B_SPLINE_SURFACE_WITH_KNOTS((2,2),(3,2,2,2,2,2,2,2,2,2,2,2,2,2,2,2,2,2,
2,2,2,2,2,2,2,2,2,2,3),(0.,1.),(0.,0.03125,0.0625,0.09375,0.125,0.15625,
0.1875,0.21875,0.25,0.28125,0.3125,0.34375,0.375,0.40625,0.4375,0.46875,
0.5,0.53125,0.5625,0.59375,0.625,0.65625,0.6875,0.71875,0.75,0.78125,0.8125,
0.84375,0.875),.UNSPECIFIED.)
GEOMETRIC_REPRESENTATION_ITEM()
RATIONAL_B_SPLINE_SURFACE(((1.,0.923879532511287,1.,0.923879532511287,1.,
0.923879532511287,1.,0.923879532511287,1.,0.923879532511287,1.,0.923879532511287,
1.,0.923879532511287,1.,0.923879532511287,1.,0.923879532511287,1.,0.923879532511287,
1.,0.923879532511287,1.,0.923879532511287,1.,0.923879532511287,1.,0.923879532511287,
1.,0.923879532511287,1.,0.923879532511287,1.,0.923879532511287,1.,0.923879532511287,
1.,0.923879532511287,1.,0.923879532511287,1.,0.923879532511287,1.,0.923879532511287,
1.,0.923879532511287,1.,0.923879532511287,1.,0.923879532511287,1.,0.923879532511287,
1.,0.923879532511287,1.,0.923879532511287,1.),(1.,0.923879532511287,1.,
0.923879532511287,1.,0.923879532511287,1.,0.923879532511287,1.,0.923879532511287,
1.,0.923879532511287,1.,0.923879532511287,1.,0.923879532511287,1.,0.923879532511287,
1.,0.923879532511287,1.,0.923879532511287,1.,0.923879532511287,1.,0.923879532511287,
1.,0.923879532511287,1.,0.923879532511287,1.,0.923879532511287,1.,0.923879532511287,
1.,0.923879532511287,1.,0.923879532511287,1.,0.923879532511287,1.,0.923879532511287,
1.,0.923879532511287,1.,0.923879532511287,1.,0.923879532511287,1.,0.923879532511287,
1.,0.923879532511287,1.,0.923879532511287,1.,0.923879532511287,1.)))
REPRESENTATION_ITEM('')
SURFACE()
);
#12686=(
BOUNDED_SURFACE()
B_SPLINE_SURFACE(1,2,((#35593,#35594,#35595,#35596,#35597,#35598,#35599,
#35600,#35601,#35602,#35603,#35604,#35605,#35606,#35607,#35608,#35609,#35610,
#35611,#35612,#35613,#35614,#35615,#35616,#35617,#35618,#35619,#35620,#35621,
#35622,#35623,#35624,#35625,#35626,#35627,#35628,#35629,#35630,#35631,#35632,
#35633,#35634,#35635,#35636,#35637,#35638,#35639,#35640,#35641,#35642,#35643,
#35644,#35645,#35646,#35647,#35648,#35649,#35650,#35651,#35652,#35653,#35654,
#35655,#35656,#35657),(#35658,#35659,#35660,#35661,#35662,#35663,#35664,
#35665,#35666,#35667,#35668,#35669,#35670,#35671,#35672,#35673,#35674,#35675,
#35676,#35677,#35678,#35679,#35680,#35681,#35682,#35683,#35684,#35685,#35686,
#35687,#35688,#35689,#35690,#35691,#35692,#35693,#35694,#35695,#35696,#35697,
#35698,#35699,#35700,#35701,#35702,#35703,#35704,#35705,#35706,#35707,#35708,
#35709,#35710,#35711,#35712,#35713,#35714,#35715,#35716,#35717,#35718,#35719,
#35720,#35721,#35722)),.RULED_SURF.,.F.,.F.,.F.)
B_SPLINE_SURFACE_WITH_KNOTS((2,2),(3,2,2,2,2,2,2,2,2,2,2,2,2,2,2,2,2,2,
2,2,2,2,2,2,2,2,2,2,2,2,2,2,3),(0.,1.),(0.,0.03125,0.0625,0.09375,0.125,
0.15625,0.1875,0.21875,0.25,0.28125,0.3125,0.34375,0.375,0.40625,0.4375,
0.46875,0.5,0.53125,0.5625,0.59375,0.625,0.65625,0.6875,0.71875,0.75,0.78125,
0.8125,0.84375,0.875,0.90625,0.9375,0.96875,1.),.UNSPECIFIED.)
GEOMETRIC_REPRESENTATION_ITEM()
RATIONAL_B_SPLINE_SURFACE(((1.,0.923879532511287,1.,0.923879532511287,1.,
0.923879532511287,1.,0.923879532511287,1.,0.923879532511287,1.,0.923879532511287,
1.,0.923879532511287,1.,0.923879532511287,1.,0.923879532511287,1.,0.923879532511287,
1.,0.923879532511287,1.,0.923879532511287,1.,0.923879532511287,1.,0.923879532511287,
1.,0.923879532511287,1.,0.923879532511287,1.,0.923879532511287,1.,0.923879532511287,
1.,0.923879532511287,1.,0.923879532511287,1.,0.923879532511287,1.,0.923879532511287,
1.,0.923879532511287,1.,0.923879532511287,1.,0.923879532511287,1.,0.923879532511287,
1.,0.923879532511287,1.,0.923879532511287,1.,0.923879532511287,1.,0.923879532511287,
1.,0.923879532511287,1.,0.923879532511287,1.),(1.,0.923879532511287,1.,
0.923879532511287,1.,0.923879532511287,1.,0.923879532511287,1.,0.923879532511287,
1.,0.923879532511287,1.,0.923879532511287,1.,0.923879532511287,1.,0.923879532511287,
1.,0.923879532511287,1.,0.923879532511287,1.,0.923879532511287,1.,0.923879532511287,
1.,0.923879532511287,1.,0.923879532511287,1.,0.923879532511287,1.,0.923879532511287,
1.,0.923879532511287,1.,0.923879532511287,1.,0.923879532511287,1.,0.923879532511287,
1.,0.923879532511287,1.,0.923879532511287,1.,0.923879532511287,1.,0.923879532511287,
1.,0.923879532511287,1.,0.923879532511287,1.,0.923879532511287,1.,0.923879532511287,
1.,0.923879532511287,1.,0.923879532511287,1.,0.923879532511287,1.)))
REPRESENTATION_ITEM('')
SURFACE()
);
#12687=(
BOUNDED_SURFACE()
B_SPLINE_SURFACE(1,2,((#35873,#35874,#35875,#35876,#35877,#35878,#35879,
#35880,#35881,#35882,#35883,#35884,#35885,#35886,#35887,#35888,#35889,#35890,
#35891,#35892,#35893,#35894,#35895,#35896,#35897,#35898,#35899,#35900,#35901,
#35902,#35903,#35904,#35905,#35906,#35907,#35908,#35909,#35910,#35911,#35912,
#35913,#35914,#35915,#35916,#35917,#35918,#35919,#35920,#35921,#35922,#35923,
#35924,#35925,#35926,#35927,#35928,#35929,#35930,#35931,#35932,#35933,#35934,
#35935,#35936,#35937),(#35938,#35939,#35940,#35941,#35942,#35943,#35944,
#35945,#35946,#35947,#35948,#35949,#35950,#35951,#35952,#35953,#35954,#35955,
#35956,#35957,#35958,#35959,#35960,#35961,#35962,#35963,#35964,#35965,#35966,
#35967,#35968,#35969,#35970,#35971,#35972,#35973,#35974,#35975,#35976,#35977,
#35978,#35979,#35980,#35981,#35982,#35983,#35984,#35985,#35986,#35987,#35988,
#35989,#35990,#35991,#35992,#35993,#35994,#35995,#35996,#35997,#35998,#35999,
#36000,#36001,#36002)),.RULED_SURF.,.F.,.F.,.F.)
B_SPLINE_SURFACE_WITH_KNOTS((2,2),(3,2,2,2,2,2,2,2,2,2,2,2,2,2,2,2,2,2,
2,2,2,2,2,2,2,2,2,2,2,2,2,2,3),(0.,1.),(0.,0.03125,0.0625,0.09375,0.125,
0.15625,0.1875,0.21875,0.25,0.28125,0.3125,0.34375,0.375,0.40625,0.4375,
0.46875,0.5,0.53125,0.5625,0.59375,0.625,0.65625,0.6875,0.71875,0.75,0.78125,
0.8125,0.84375,0.875,0.90625,0.9375,0.96875,1.),.UNSPECIFIED.)
GEOMETRIC_REPRESENTATION_ITEM()
RATIONAL_B_SPLINE_SURFACE(((1.,0.923879532511287,1.,0.923879532511287,1.,
0.923879532511287,1.,0.923879532511287,1.,0.923879532511287,1.,0.923879532511287,
1.,0.923879532511287,1.,0.923879532511287,1.,0.923879532511287,1.,0.923879532511287,
1.,0.923879532511287,1.,0.923879532511287,1.,0.923879532511287,1.,0.923879532511287,
1.,0.923879532511287,1.,0.923879532511287,1.,0.923879532511287,1.,0.923879532511287,
1.,0.923879532511287,1.,0.923879532511287,1.,0.923879532511287,1.,0.923879532511287,
1.,0.923879532511287,1.,0.923879532511287,1.,0.923879532511287,1.,0.923879532511287,
1.,0.923879532511287,1.,0.923879532511287,1.,0.923879532511287,1.,0.923879532511287,
1.,0.923879532511287,1.,0.923879532511287,1.),(1.,0.923879532511287,1.,
0.923879532511287,1.,0.923879532511287,1.,0.923879532511287,1.,0.923879532511287,
1.,0.923879532511287,1.,0.923879532511287,1.,0.923879532511287,1.,0.923879532511287,
1.,0.923879532511287,1.,0.923879532511287,1.,0.923879532511287,1.,0.923879532511287,
1.,0.923879532511287,1.,0.923879532511287,1.,0.923879532511287,1.,0.923879532511287,
1.,0.923879532511287,1.,0.923879532511287,1.,0.923879532511287,1.,0.923879532511287,
1.,0.923879532511287,1.,0.923879532511287,1.,0.923879532511287,1.,0.923879532511287,
1.,0.923879532511287,1.,0.923879532511287,1.,0.923879532511287,1.,0.923879532511287,
1.,0.923879532511287,1.,0.923879532511287,1.,0.923879532511287,1.)))
REPRESENTATION_ITEM('')
SURFACE()
);
#12688=(
BOUNDED_SURFACE()
B_SPLINE_SURFACE(3,2,((#36164,#36165,#36166),(#36167,#36168,#36169),(#36170,
#36171,#36172),(#36173,#36174,#36175),(#36176,#36177,#36178),(#36179,#36180,
#36181),(#36182,#36183,#36184),(#36185,#36186,#36187),(#36188,#36189,#36190),
(#36191,#36192,#36193),(#36194,#36195,#36196),(#36197,#36198,#36199),(#36200,
#36201,#36202),(#36203,#36204,#36205),(#36206,#36207,#36208),(#36209,#36210,
#36211),(#36212,#36213,#36214),(#36215,#36216,#36217),(#36218,#36219,#36220),
(#36221,#36222,#36223),(#36224,#36225,#36226),(#36227,#36228,#36229),(#36230,
#36231,#36232),(#36233,#36234,#36235),(#36236,#36237,#36238),(#36239,#36240,
#36241),(#36242,#36243,#36244),(#36245,#36246,#36247),(#36248,#36249,#36250),
(#36251,#36252,#36253),(#36254,#36255,#36256),(#36257,#36258,#36259),(#36260,
#36261,#36262),(#36263,#36264,#36265),(#36266,#36267,#36268),(#36269,#36270,
#36271),(#36272,#36273,#36274),(#36275,#36276,#36277),(#36278,#36279,#36280),
(#36281,#36282,#36283),(#36284,#36285,#36286),(#36287,#36288,#36289),(#36290,
#36291,#36292),(#36293,#36294,#36295),(#36296,#36297,#36298),(#36299,#36300,
#36301),(#36302,#36303,#36304),(#36305,#36306,#36307),(#36308,#36309,#36310),
(#36311,#36312,#36313),(#36314,#36315,#36316),(#36317,#36318,#36319),(#36320,
#36321,#36322),(#36323,#36324,#36325),(#36326,#36327,#36328),(#36329,#36330,
#36331),(#36332,#36333,#36334),(#36335,#36336,#36337),(#36338,#36339,#36340),
(#36341,#36342,#36343),(#36344,#36345,#36346),(#36347,#36348,#36349),(#36350,
#36351,#36352),(#36353,#36354,#36355),(#36356,#36357,#36358),(#36359,#36360,
#36361),(#36362,#36363,#36364),(#36365,#36366,#36367),(#36368,#36369,#36370),
(#36371,#36372,#36373),(#36374,#36375,#36376),(#36377,#36378,#36379),(#36380,
#36381,#36382),(#36383,#36384,#36385),(#36386,#36387,#36388),(#36389,#36390,
#36391),(#36392,#36393,#36394),(#36395,#36396,#36397),(#36398,#36399,#36400),
(#36401,#36402,#36403),(#36404,#36405,#36406),(#36407,#36408,#36409),(#36410,
#36411,#36412),(#36413,#36414,#36415),(#36416,#36417,#36418),(#36419,#36420,
#36421),(#36422,#36423,#36424),(#36425,#36426,#36427),(#36428,#36429,#36430),
(#36431,#36432,#36433),(#36434,#36435,#36436),(#36437,#36438,#36439),(#36440,
#36441,#36442),(#36443,#36444,#36445),(#36446,#36447,#36448),(#36449,#36450,
#36451),(#36452,#36453,#36454),(#36455,#36456,#36457),(#36458,#36459,#36460),
(#36461,#36462,#36463),(#36464,#36465,#36466),(#36467,#36468,#36469),(#36470,
#36471,#36472),(#36473,#36474,#36475),(#36476,#36477,#36478),(#36479,#36480,
#36481),(#36482,#36483,#36484),(#36485,#36486,#36487),(#36488,#36489,#36490),
(#36491,#36492,#36493),(#36494,#36495,#36496),(#36497,#36498,#36499),(#36500,
#36501,#36502),(#36503,#36504,#36505),(#36506,#36507,#36508),(#36509,#36510,
#36511),(#36512,#36513,#36514),(#36515,#36516,#36517),(#36518,#36519,#36520),
(#36521,#36522,#36523),(#36524,#36525,#36526),(#36527,#36528,#36529),(#36530,
#36531,#36532),(#36533,#36534,#36535),(#36536,#36537,#36538),(#36539,#36540,
#36541),(#36542,#36543,#36544),(#36545,#36546,#36547),(#36548,#36549,#36550),
(#36551,#36552,#36553),(#36554,#36555,#36556),(#36557,#36558,#36559),(#36560,
#36561,#36562),(#36563,#36564,#36565),(#36566,#36567,#36568),(#36569,#36570,
#36571),(#36572,#36573,#36574),(#36575,#36576,#36577),(#36578,#36579,#36580),
(#36581,#36582,#36583),(#36584,#36585,#36586),(#36587,#36588,#36589),(#36590,
#36591,#36592),(#36593,#36594,#36595),(#36596,#36597,#36598),(#36599,#36600,
#36601),(#36602,#36603,#36604),(#36605,#36606,#36607),(#36608,#36609,#36610),
(#36611,#36612,#36613),(#36614,#36615,#36616),(#36617,#36618,#36619),(#36620,
#36621,#36622),(#36623,#36624,#36625),(#36626,#36627,#36628),(#36629,#36630,
#36631),(#36632,#36633,#36634),(#36635,#36636,#36637),(#36638,#36639,#36640),
(#36641,#36642,#36643),(#36644,#36645,#36646),(#36647,#36648,#36649),(#36650,
#36651,#36652),(#36653,#36654,#36655),(#36656,#36657,#36658),(#36659,#36660,
#36661),(#36662,#36663,#36664),(#36665,#36666,#36667),(#36668,#36669,#36670),
(#36671,#36672,#36673),(#36674,#36675,#36676),(#36677,#36678,#36679),(#36680,
#36681,#36682),(#36683,#36684,#36685),(#36686,#36687,#36688),(#36689,#36690,
#36691),(#36692,#36693,#36694),(#36695,#36696,#36697),(#36698,#36699,#36700),
(#36701,#36702,#36703),(#36704,#36705,#36706),(#36707,#36708,#36709),(#36710,
#36711,#36712),(#36713,#36714,#36715),(#36716,#36717,#36718),(#36719,#36720,
#36721),(#36722,#36723,#36724),(#36725,#36726,#36727),(#36728,#36729,#36730),
(#36731,#36732,#36733),(#36734,#36735,#36736),(#36737,#36738,#36739),(#36740,
#36741,#36742),(#36743,#36744,#36745),(#36746,#36747,#36748),(#36749,#36750,
#36751),(#36752,#36753,#36754),(#36755,#36756,#36757),(#36758,#36759,#36760),
(#36761,#36762,#36763),(#36764,#36765,#36766),(#36767,#36768,#36769),(#36770,
#36771,#36772),(#36773,#36774,#36775),(#36776,#36777,#36778),(#36779,#36780,
#36781),(#36782,#36783,#36784),(#36785,#36786,#36787),(#36788,#36789,#36790),
(#36791,#36792,#36793),(#36794,#36795,#36796),(#36797,#36798,#36799),(#36800,
#36801,#36802),(#36803,#36804,#36805),(#36806,#36807,#36808),(#36809,#36810,
#36811),(#36812,#36813,#36814),(#36815,#36816,#36817),(#36818,#36819,#36820),
(#36821,#36822,#36823),(#36824,#36825,#36826),(#36827,#36828,#36829),(#36830,
#36831,#36832),(#36833,#36834,#36835),(#36836,#36837,#36838),(#36839,#36840,
#36841),(#36842,#36843,#36844),(#36845,#36846,#36847),(#36848,#36849,#36850),
(#36851,#36852,#36853),(#36854,#36855,#36856),(#36857,#36858,#36859),(#36860,
#36861,#36862),(#36863,#36864,#36865),(#36866,#36867,#36868),(#36869,#36870,
#36871),(#36872,#36873,#36874),(#36875,#36876,#36877),(#36878,#36879,#36880),
(#36881,#36882,#36883),(#36884,#36885,#36886),(#36887,#36888,#36889),(#36890,
#36891,#36892),(#36893,#36894,#36895),(#36896,#36897,#36898),(#36899,#36900,
#36901),(#36902,#36903,#36904),(#36905,#36906,#36907),(#36908,#36909,#36910),
(#36911,#36912,#36913),(#36914,#36915,#36916),(#36917,#36918,#36919),(#36920,
#36921,#36922),(#36923,#36924,#36925),(#36926,#36927,#36928),(#36929,#36930,
#36931),(#36932,#36933,#36934),(#36935,#36936,#36937),(#36938,#36939,#36940),
(#36941,#36942,#36943),(#36944,#36945,#36946),(#36947,#36948,#36949),(#36950,
#36951,#36952),(#36953,#36954,#36955),(#36956,#36957,#36958),(#36959,#36960,
#36961),(#36962,#36963,#36964),(#36965,#36966,#36967),(#36968,#36969,#36970),
(#36971,#36972,#36973),(#36974,#36975,#36976),(#36977,#36978,#36979),(#36980,
#36981,#36982),(#36983,#36984,#36985),(#36986,#36987,#36988),(#36989,#36990,
#36991),(#36992,#36993,#36994),(#36995,#36996,#36997),(#36998,#36999,#37000),
(#37001,#37002,#37003),(#37004,#37005,#37006),(#37007,#37008,#37009),(#37010,
#37011,#37012),(#37013,#37014,#37015),(#37016,#37017,#37018),(#37019,#37020,
#37021),(#37022,#37023,#37024),(#37025,#37026,#37027),(#37028,#37029,#37030),
(#37031,#37032,#37033),(#37034,#37035,#37036),(#37037,#37038,#37039),(#37040,
#37041,#37042),(#37043,#37044,#37045),(#37046,#37047,#37048),(#37049,#37050,
#37051),(#37052,#37053,#37054),(#37055,#37056,#37057),(#37058,#37059,#37060),
(#37061,#37062,#37063),(#37064,#37065,#37066),(#37067,#37068,#37069),(#37070,
#37071,#37072),(#37073,#37074,#37075),(#37076,#37077,#37078),(#37079,#37080,
#37081),(#37082,#37083,#37084),(#37085,#37086,#37087),(#37088,#37089,#37090),
(#37091,#37092,#37093),(#37094,#37095,#37096),(#37097,#37098,#37099),(#37100,
#37101,#37102),(#37103,#37104,#37105),(#37106,#37107,#37108),(#37109,#37110,
#37111),(#37112,#37113,#37114),(#37115,#37116,#37117),(#37118,#37119,#37120),
(#37121,#37122,#37123),(#37124,#37125,#37126),(#37127,#37128,#37129),(#37130,
#37131,#37132),(#37133,#37134,#37135),(#37136,#37137,#37138),(#37139,#37140,
#37141),(#37142,#37143,#37144),(#37145,#37146,#37147),(#37148,#37149,#37150),
(#37151,#37152,#37153),(#37154,#37155,#37156),(#37157,#37158,#37159),(#37160,
#37161,#37162),(#37163,#37164,#37165),(#37166,#37167,#37168),(#37169,#37170,
#37171),(#37172,#37173,#37174),(#37175,#37176,#37177),(#37178,#37179,#37180),
(#37181,#37182,#37183),(#37184,#37185,#37186),(#37187,#37188,#37189),(#37190,
#37191,#37192),(#37193,#37194,#37195),(#37196,#37197,#37198),(#37199,#37200,
#37201),(#37202,#37203,#37204),(#37205,#37206,#37207),(#37208,#37209,#37210),
(#37211,#37212,#37213)),.UNSPECIFIED.,.F.,.F.,.F.)
B_SPLINE_SURFACE_WITH_KNOTS((4,2,2,2,2,2,2,2,2,2,2,2,2,2,2,2,2,2,2,2,2,
2,2,2,2,2,2,2,2,2,2,2,2,2,2,2,2,2,2,2,2,2,2,2,2,2,2,2,2,2,2,2,2,2,2,2,2,
2,2,2,2,2,2,2,2,2,2,2,2,2,2,2,2,2,2,2,2,2,2,2,2,2,2,2,2,2,2,2,2,2,2,2,2,
2,2,2,2,2,2,2,2,2,2,2,2,2,2,2,2,2,2,2,2,2,2,2,2,2,2,2,2,2,2,2,2,2,2,2,2,
2,2,2,2,2,2,2,2,2,2,2,2,2,2,2,2,2,2,2,2,2,2,2,2,2,2,2,2,2,2,2,2,2,2,2,2,
2,2,2,2,2,2,2,2,2,4),(3,3),(0.193149276135837,0.194573475589254,0.19599767504267,
0.197421874496086,0.198846073949502,0.201694472856334,0.203118672309751,
0.204542871763166,0.207391270669999,0.208815470123415,0.210239669576831,
0.213088068483663,0.21451226793708,0.215936467390495,0.218784866297328,
0.22163326520416,0.223057464657577,0.224481664110992,0.227330063017825,
0.228754262471241,0.230178461924657,0.233026860831489,0.234451060284905,
0.235875259738322,0.238723658645154,0.241572057551987,0.244420456458819,
0.247268855365651,0.248693054819067,0.250117254272483,0.252965653179316,
0.255814052086148,0.25866245099298,0.260086650446396,0.261510849899812,
0.264359248806645,0.267207647713477,0.27005604662031,0.272904445527142,
0.274328644980558,0.275752844433974,0.278601243340806,0.280025442794223,
0.281449642247639,0.284298041154471,0.285722240607887,0.287146440061304,
0.289994838968135,0.292843237874968,0.294267437328384,0.2956916367818,0.298540035688632,
0.299964235142049,0.301388434595465,0.304236833502297,0.305661032955714,
0.307085232409129,0.309933631315962,0.311357830769378,0.312782030222794,
0.315630429129626,0.318478828036458,0.319903027489875,0.321327226943291,
0.324175625850124,0.32559982530354,0.327024024756956,0.329872423663788,
0.331296623117204,0.33272082257062,0.335569221477452,0.336993420930868,
0.338417620384285,0.341266019291117,0.344114418197949,0.345538617651366,
0.346962817104781,0.349811216011614,0.35123541546503,0.352659614918446,
0.355508013825279,0.356932213278695,0.358356412732111,0.361204811638944,
0.364053210545775,0.366901609452608,0.36975000835944,0.371174207812856,
0.372598407266273,0.375446806173105,0.378295205079937,0.381143603986769,
0.383992002893602,0.385416202347018,0.386840401800434,0.389688800707267,
0.392537199614098,0.395385598520931,0.398233997427763,0.39965819688118,
0.401082396334596,0.403930795241428,0.40677919414826,0.409627593055092,
0.411051792508509,0.412475991961925,0.415324390868757,0.418172789775589,
0.421021188682421,0.423869587589254,0.42529378704267,0.426717986496086,
0.429566385402918,0.432414784309751,0.435263183216583,0.43668738267,0.438111582123415,
0.440959981030248,0.44380837993708,0.446656778843912,0.449505177750745,
0.450929377204161,0.452353576657577,0.455201975564409,0.456626175017826,
0.458050374471242,0.460898773378074,0.46232297283149,0.463747172284906,
0.466595571191739,0.469443970098571,0.470868169551987,0.472292369005403,
0.475140767912236,0.476564967365652,0.477989166819068,0.4808375657259,0.482261765179316,
0.483685964632732,0.486534363539565,0.487958562992981,0.489382762446397,
0.492231161353229,0.495079560260062,0.496503759713478,0.497927959166894,
0.500776358073726,0.502200557527142,0.503624756980559,0.506473155887391,
0.507897355340807,0.509321554794223,0.512169953701055,0.513594153154472,
0.515018352607888,0.51786675151472,0.520715150421552,0.522139349874969,
0.523563549328385,0.526411948235217,0.527836147688633,0.529260347142049,
0.532108746048882,0.533532945502298,0.534957144955714,0.537805543862546,
0.540653942769379,0.543502341676211,0.546350740583043,0.547774940036459,
0.549199139489875,0.552047538396708,0.55489593730354,0.556320136756956,
0.557744336210372),(0.,1.),.UNSPECIFIED.)
GEOMETRIC_REPRESENTATION_ITEM()
RATIONAL_B_SPLINE_SURFACE(((1.,0.722699314797039,1.),(1.,0.739505233921062,
1.),(1.,0.750913931065822,1.),(1.,0.763867107266192,1.),(1.,0.763748327602808,
1.),(1.,0.763840788023146,1.),(1.,0.763934660767682,1.),(1.,0.764075220899086,
1.),(1.,0.764122201658888,1.),(1.,0.764124519516567,1.),(1.,0.763899183527604,
1.),(1.,0.763724776258188,1.),(1.,0.763718186244016,1.),(1.,0.763733433596857,
1.),(1.,0.763753474169701,1.),(1.,0.76378697338056,1.),(1.,0.763752776696806,
1.),(1.,0.763751538604513,1.),(1.,0.763763940574543,1.),(1.,0.76396102079176,
1.),(1.,0.764115220844393,1.),(1.,0.764546159205604,1.),(1.,0.764765645744293,
1.),(1.,0.764727907314652,1.),(1.,0.764660932529331,1.),(1.,0.764455367186594,
1.),(1.,0.764316238910568,1.),(1.,0.763935188171349,1.),(1.,0.763859972893716,
1.),(1.,0.764274012465505,1.),(1.,0.76457343122981,1.),(1.,0.764686738337569,
1.),(1.,0.764674014513268,1.),(1.,0.764551476703936,1.),(1.,0.764442146422493,
1.),(1.,0.764057990860656,1.),(1.,0.763712262722046,1.),(1.,0.763810315046671,
1.),(1.,0.763927911530464,1.),(1.,0.764191701339472,1.),(1.,0.764336047024834,
1.),(1.,0.764669419545292,1.),(1.,0.764732856732067,1.),(1.,0.764530427751721,
1.),(1.,0.764419860629288,1.),(1.,0.764182994716093,1.),(1.,0.764056864941671,
1.),(1.,0.763847972269309,1.),(1.,0.764090105631719,1.),(1.,0.764557854644049,
1.),(1.,0.764727075408901,1.),(1.,0.764592469893156,1.),(1.,0.76429205517341,
1.),(1.,0.763778933821465,1.),(1.,0.763714479620357,1.),(1.,0.764064348110842,
1.),(1.,0.764214432578513,1.),(1.,0.764468330597694,1.),(1.,0.76457255700642,
1.),(1.,0.764738627262064,1.),(1.,0.764627762575867,1.),(1.,0.764184080030961,
1.),(1.,0.763869939463043,1.),(1.,0.764028580212725,1.),(1.,0.764371448031126,
1.),(1.,0.764629675614398,1.),(1.,0.764679319927948,1.),(1.,0.764673366372952,
1.),(1.,0.764617034573576,1.),(1.,0.76432860904734,1.),(1.,0.763955320692206,
1.),(1.,0.763676394380582,1.),(1.,0.763950171983398,1.),(1.,0.764492856603529,
1.),(1.,0.764699044829153,1.),(1.,0.764646790603644,1.),(1.,0.764389512112811,
1.),(1.,0.764047552656364,1.),(1.,0.763947820879635,1.),(1.,0.7639238839966,
1.),(1.,0.764008346032025,1.),(1.,0.764331498413827,1.),(1.,0.764611886319225,
1.),(1.,0.764692272869539,1.),(1.,0.764668655970716,1.),(1.,0.764526003286365,
1.),(1.,0.764407585602509,1.),(1.,0.76401108352945,1.),(1.,0.763691597605849,
1.),(1.,0.763839790873091,1.),(1.,0.763964817595917,1.),(1.,0.764232389234053,
1.),(1.,0.764375097736406,1.),(1.,0.764691651150716,1.),(1.,0.764728274974876,
1.),(1.,0.764425962489577,1.),(1.,0.76408640921874,1.),(1.,0.763910378354219,
1.),(1.,0.763940222092509,1.),(1.,0.764114492355252,1.),(1.,0.764244146959905,
1.),(1.,0.764588972482738,1.),(1.,0.764734205927101,1.),(1.,0.764606540240188,
1.),(1.,0.764512157040054,1.),(1.,0.764269236036256,1.),(1.,0.764121427321446,
1.),(1.,0.763749143028262,1.),(1.,0.763738472511642,1.),(1.,0.764104348255375,
1.),(1.,0.764252603446921,1.),(1.,0.764499401472594,1.),(1.,0.764596727279848,
1.),(1.,0.764735435145248,1.),(1.,0.764599860555111,1.),(1.,0.764258563412971,
1.),(1.,0.764128257509806,1.),(1.,0.763947151915775,1.),(1.,0.763909077799273,
1.),(1.,0.764069787586111,1.),(1.,0.764411198803846,1.),(1.,0.76472602456633,
1.),(1.,0.764699635747033,1.),(1.,0.764390238431946,1.),(1.,0.764249113212434,
1.),(1.,0.76398024343851,1.),(1.,0.76385228181124,1.),(1.,0.763685718677883,
1.),(1.,0.763993094277294,1.),(1.,0.764392354435882,1.),(1.,0.764513634094182,
1.),(1.,0.764662651735703,1.),(1.,0.764690398115232,1.),(1.,0.764621689213982,
1.),(1.,0.764347939142106,1.),(1.,0.764019298699886,1.),(1.,0.76392987954948,
1.),(1.,0.763939856257347,1.),(1.,0.764035977098891,1.),(1.,0.764373733783113,
1.),(1.,0.764638010806738,1.),(1.,0.764689070469253,1.),(1.,0.764655118678298,
1.),(1.,0.764497116908555,1.),(1.,0.764372434889717,1.),(1.,0.763967351373681,
1.),(1.,0.763679332198018,1.),(1.,0.763936049040803,1.),(1.,0.764310708178265,
1.),(1.,0.764607884141716,1.),(1.,0.764667933623475,1.),(1.,0.764681694245897,
1.),(1.,0.764636097985227,1.),(1.,0.764386747051517,1.),(1.,0.764045117651283,
1.),(1.,0.763908872524616,1.),(1.,0.76395754226787,1.),(1.,0.764149013532703,
1.),(1.,0.764280900945993,1.),(1.,0.764617975384813,1.),(1.,0.764738649656064,
1.),(1.,0.764583519945107,1.),(1.,0.764482287442958,1.),(1.,0.764230946224071,
1.),(1.,0.764080793566669,1.),(1.,0.763723362703644,1.),(1.,0.763766722502332,
1.),(1.,0.76427291441918,1.),(1.,0.764580062163821,1.),(1.,0.764729453155635,
1.),(1.,0.764569528540465,1.),(1.,0.764105164381652,1.),(1.,0.763848474045922,
1.),(1.,0.764044371934837,1.),(1.,0.76416925555259,1.),(1.,0.764407167526877,
1.),(1.,0.764520334285805,1.),(1.,0.764733406914302,1.),(1.,0.764680756093071,
1.),(1.,0.764245428286248,1.),(1.,0.763860766458277,1.),(1.,0.763702734210281,
1.),(1.,0.764048836280064,1.),(1.,0.764566623657068,1.),(1.,0.764724834305744,
1.),(1.,0.764625210011228,1.),(1.,0.764542331423941,1.),(1.,0.764326337118295,
1.),(1.,0.764193221628244,1.),(1.,0.763882510299014,1.),(1.,0.763955361792152,
1.),(1.,0.764416713168217,1.),(1.,0.764665129414208,1.),(1.,0.764686940352922,
1.),(1.,0.764460460724398,1.),(1.,0.76392208068725,1.),(1.,0.763672740817721,
1.),(1.,0.763911324525423,1.),(1.,0.764051931517915,1.),(1.,0.764323031146854,
1.),(1.,0.764453731360604,1.),(1.,0.764720907693508,1.),(1.,0.764706351034155,
1.),(1.,0.764343019630522,1.),(1.,0.763994121210039,1.),(1.,0.763887698205184,
1.),(1.,0.764212830355328,1.),(1.,0.764537011123856,1.),(1.,0.764622045143321,
1.),(1.,0.764692681407165,1.),(1.,0.764677599503643,1.),(1.,0.764487344119654,
1.),(1.,0.764144753839761,1.),(1.,0.763702587630224,1.),(1.,0.763799887222974,
1.),(1.,0.764330273475046,1.),(1.,0.764614508454279,1.),(1.,0.76471671542289,
1.),(1.,0.764535560686859,1.),(1.,0.764179665899326,1.),(1.,0.764053667616838,
1.),(1.,0.763916268430484,1.),(1.,0.763926969747539,1.),(1.,0.764161781488297,
1.),(1.,0.764488323704147,1.),(1.,0.764737663853121,1.),(1.,0.76465390164221,
1.),(1.,0.764189010841196,1.),(1.,0.763814890315767,1.),(1.,0.763751197251442,
1.),(1.,0.763833803031666,1.),(1.,0.764068070995748,1.),(1.,0.764218139786203,
1.),(1.,0.764598269472164,1.),(1.,0.764731993944393,1.),(1.,0.764561917625315,
1.),(1.,0.764257407337477,1.),(1.,0.763865858127282,1.),(1.,0.763986854740837,
1.),(1.,0.764456099242501,1.),(1.,0.764684057417691,1.),(1.,0.764672342131847,
1.),(1.,0.764615183579261,1.),(1.,0.764421331097182,1.),(1.,0.764285304332037,
1.),(1.,0.763880849253991,1.),(1.,0.763675921984343,1.),(1.,0.763946650092346,
1.),(1.,0.764089650304982,1.),(1.,0.764360438200807,1.),(1.,0.764486720466232,
1.),(1.,0.764730902773989,1.),(1.,0.76468994788372,1.),(1.,0.764400105207107,
1.),(1.,0.76427192956214,1.),(1.,0.764044803269244,1.),(1.,0.763945914264244,
1.),(1.,0.763914820230933,1.),(1.,0.764254555421925,1.),(1.,0.764667433474705,
1.),(1.,0.764739498660029,1.),(1.,0.76452342410793,1.),(1.,0.764404140660104,
1.),(1.,0.764139137351779,1.),(1.,0.763993333719004,1.),(1.,0.763687184023814,
1.),(1.,0.763834660278889,1.),(1.,0.764236201135504,1.),(1.,0.764378436194924,
1.),(1.,0.764588470001048,1.),(1.,0.764656185266166,1.),(1.,0.764703128203519,
1.),(1.,0.764500442535882,1.),(1.,0.764145398632785,1.),(1.,0.764024978752906,
1.),(1.,0.763910063563777,1.),(1.,0.763941793066124,1.),(1.,0.764205956929848,
1.),(1.,0.764523303545078,1.),(1.,0.764683865095869,1.),(1.,0.764691313612272,
1.),(1.,0.764604453303825,1.),(1.,0.764509476141111,1.),(1.,0.764143354152028,
1.),(1.,0.76377288563184,1.),(1.,0.763764830719989,1.),(1.,0.764133605247446,
1.),(1.,0.764502115195786,1.),(1.,0.76459889368469,1.),(1.,0.764689625425294,
1.),(1.,0.764684310949503,1.),(1.,0.764529245268432,1.),(1.,0.764214503367863,
1.),(1.,0.763945490960164,1.),(1.,0.763909269234188,1.),(1.,0.764018931218163,
1.),(1.,0.764138489117333,1.),(1.,0.764493972977306,1.),(1.,0.764700928871412,
1.),(1.,0.764659938305659,1.),(1.,0.764594156328028,1.),(1.,0.76438685338652,
1.),(1.,0.764245191949504,1.),(1.,0.763842015003482,1.),(1.,0.763684920017492,
1.),(1.,0.763985174574737,1.),(1.,0.764130310945844,1.),(1.,0.764395784805852,
1.),(1.,0.764516186506651,1.),(1.,0.7647374102588,1.),(1.,0.764670099972414,
1.),(1.,0.764261299224288,1.),(1.,0.763920339000742,1.),(1.,0.763939902291723,
1.),(1.,0.764037338315704,1.),(1.,0.764264861871258,1.),(1.,0.764394777042652,
1.),(1.,0.764691836447148,1.),(1.,0.76474026082274,1.),(1.,0.764502444879734,
1.),(1.,0.764377615086339,1.),(1.,0.764105911424375,1.),(1.,0.763960844285112,
1.),(1.,0.763677550033968,1.),(1.,0.763867750516721,1.),(1.,0.764275857523739,
1.),(1.,0.764415362774288,1.),(1.,0.764618984869432,1.),(1.,0.764682548102571,
1.),(1.,0.764714269609273,1.),(1.,0.764500783672347,1.),(1.,0.764050275516554,
1.),(1.,0.763947142258318,1.),(1.,0.764253243543243,1.),(1.,0.76447716836975,
1.),(1.,0.764542829763807,1.),(1.,0.764385405357976,1.),(1.,0.764045762298611,
1.),(1.,0.763921199778699,1.),(1.,0.763756105588418,1.),(1.,0.76372541036921,
1.),(1.,0.763900015681686,1.),(1.,0.764124851617388,1.),(1.,0.764121206660071,
1.),(1.,0.763885915644855,1.),(1.,0.763748500497105,1.),(1.,0.763869356955843,
1.),(1.,0.750994184797527,1.),(1.,0.739646079293118,1.),(1.,0.722895202390289,
1.)))
REPRESENTATION_ITEM('')
SURFACE()
);
#12689=(
BOUNDED_SURFACE()
B_SPLINE_SURFACE(3,2,((#37478,#37479,#37480),(#37481,#37482,#37483),(#37484,
#37485,#37486),(#37487,#37488,#37489),(#37490,#37491,#37492),(#37493,#37494,
#37495),(#37496,#37497,#37498),(#37499,#37500,#37501),(#37502,#37503,#37504),
(#37505,#37506,#37507),(#37508,#37509,#37510),(#37511,#37512,#37513),(#37514,
#37515,#37516),(#37517,#37518,#37519),(#37520,#37521,#37522),(#37523,#37524,
#37525),(#37526,#37527,#37528),(#37529,#37530,#37531),(#37532,#37533,#37534),
(#37535,#37536,#37537),(#37538,#37539,#37540),(#37541,#37542,#37543),(#37544,
#37545,#37546),(#37547,#37548,#37549),(#37550,#37551,#37552),(#37553,#37554,
#37555),(#37556,#37557,#37558),(#37559,#37560,#37561),(#37562,#37563,#37564),
(#37565,#37566,#37567),(#37568,#37569,#37570),(#37571,#37572,#37573),(#37574,
#37575,#37576),(#37577,#37578,#37579),(#37580,#37581,#37582),(#37583,#37584,
#37585),(#37586,#37587,#37588),(#37589,#37590,#37591),(#37592,#37593,#37594),
(#37595,#37596,#37597),(#37598,#37599,#37600),(#37601,#37602,#37603),(#37604,
#37605,#37606),(#37607,#37608,#37609),(#37610,#37611,#37612),(#37613,#37614,
#37615),(#37616,#37617,#37618),(#37619,#37620,#37621),(#37622,#37623,#37624),
(#37625,#37626,#37627),(#37628,#37629,#37630),(#37631,#37632,#37633),(#37634,
#37635,#37636),(#37637,#37638,#37639),(#37640,#37641,#37642),(#37643,#37644,
#37645),(#37646,#37647,#37648),(#37649,#37650,#37651),(#37652,#37653,#37654),
(#37655,#37656,#37657),(#37658,#37659,#37660),(#37661,#37662,#37663),(#37664,
#37665,#37666),(#37667,#37668,#37669),(#37670,#37671,#37672),(#37673,#37674,
#37675),(#37676,#37677,#37678),(#37679,#37680,#37681),(#37682,#37683,#37684),
(#37685,#37686,#37687),(#37688,#37689,#37690),(#37691,#37692,#37693),(#37694,
#37695,#37696),(#37697,#37698,#37699),(#37700,#37701,#37702),(#37703,#37704,
#37705),(#37706,#37707,#37708),(#37709,#37710,#37711),(#37712,#37713,#37714),
(#37715,#37716,#37717),(#37718,#37719,#37720),(#37721,#37722,#37723),(#37724,
#37725,#37726),(#37727,#37728,#37729),(#37730,#37731,#37732),(#37733,#37734,
#37735),(#37736,#37737,#37738),(#37739,#37740,#37741),(#37742,#37743,#37744),
(#37745,#37746,#37747),(#37748,#37749,#37750),(#37751,#37752,#37753),(#37754,
#37755,#37756),(#37757,#37758,#37759),(#37760,#37761,#37762),(#37763,#37764,
#37765),(#37766,#37767,#37768),(#37769,#37770,#37771),(#37772,#37773,#37774),
(#37775,#37776,#37777),(#37778,#37779,#37780),(#37781,#37782,#37783),(#37784,
#37785,#37786),(#37787,#37788,#37789),(#37790,#37791,#37792),(#37793,#37794,
#37795),(#37796,#37797,#37798),(#37799,#37800,#37801),(#37802,#37803,#37804),
(#37805,#37806,#37807),(#37808,#37809,#37810),(#37811,#37812,#37813),(#37814,
#37815,#37816),(#37817,#37818,#37819),(#37820,#37821,#37822),(#37823,#37824,
#37825),(#37826,#37827,#37828),(#37829,#37830,#37831),(#37832,#37833,#37834),
(#37835,#37836,#37837),(#37838,#37839,#37840),(#37841,#37842,#37843),(#37844,
#37845,#37846),(#37847,#37848,#37849),(#37850,#37851,#37852),(#37853,#37854,
#37855),(#37856,#37857,#37858),(#37859,#37860,#37861),(#37862,#37863,#37864),
(#37865,#37866,#37867),(#37868,#37869,#37870),(#37871,#37872,#37873),(#37874,
#37875,#37876),(#37877,#37878,#37879),(#37880,#37881,#37882),(#37883,#37884,
#37885),(#37886,#37887,#37888),(#37889,#37890,#37891),(#37892,#37893,#37894),
(#37895,#37896,#37897),(#37898,#37899,#37900),(#37901,#37902,#37903),(#37904,
#37905,#37906),(#37907,#37908,#37909),(#37910,#37911,#37912),(#37913,#37914,
#37915),(#37916,#37917,#37918),(#37919,#37920,#37921),(#37922,#37923,#37924),
(#37925,#37926,#37927),(#37928,#37929,#37930),(#37931,#37932,#37933),(#37934,
#37935,#37936),(#37937,#37938,#37939),(#37940,#37941,#37942),(#37943,#37944,
#37945),(#37946,#37947,#37948),(#37949,#37950,#37951),(#37952,#37953,#37954),
(#37955,#37956,#37957),(#37958,#37959,#37960),(#37961,#37962,#37963),(#37964,
#37965,#37966),(#37967,#37968,#37969),(#37970,#37971,#37972),(#37973,#37974,
#37975),(#37976,#37977,#37978),(#37979,#37980,#37981),(#37982,#37983,#37984),
(#37985,#37986,#37987),(#37988,#37989,#37990),(#37991,#37992,#37993),(#37994,
#37995,#37996),(#37997,#37998,#37999),(#38000,#38001,#38002),(#38003,#38004,
#38005),(#38006,#38007,#38008),(#38009,#38010,#38011),(#38012,#38013,#38014),
(#38015,#38016,#38017),(#38018,#38019,#38020),(#38021,#38022,#38023),(#38024,
#38025,#38026),(#38027,#38028,#38029),(#38030,#38031,#38032),(#38033,#38034,
#38035),(#38036,#38037,#38038),(#38039,#38040,#38041),(#38042,#38043,#38044),
(#38045,#38046,#38047),(#38048,#38049,#38050),(#38051,#38052,#38053),(#38054,
#38055,#38056),(#38057,#38058,#38059),(#38060,#38061,#38062),(#38063,#38064,
#38065),(#38066,#38067,#38068),(#38069,#38070,#38071),(#38072,#38073,#38074),
(#38075,#38076,#38077),(#38078,#38079,#38080),(#38081,#38082,#38083),(#38084,
#38085,#38086),(#38087,#38088,#38089),(#38090,#38091,#38092),(#38093,#38094,
#38095),(#38096,#38097,#38098),(#38099,#38100,#38101),(#38102,#38103,#38104),
(#38105,#38106,#38107),(#38108,#38109,#38110),(#38111,#38112,#38113),(#38114,
#38115,#38116),(#38117,#38118,#38119),(#38120,#38121,#38122),(#38123,#38124,
#38125),(#38126,#38127,#38128),(#38129,#38130,#38131),(#38132,#38133,#38134),
(#38135,#38136,#38137),(#38138,#38139,#38140),(#38141,#38142,#38143),(#38144,
#38145,#38146),(#38147,#38148,#38149),(#38150,#38151,#38152),(#38153,#38154,
#38155),(#38156,#38157,#38158),(#38159,#38160,#38161),(#38162,#38163,#38164),
(#38165,#38166,#38167),(#38168,#38169,#38170),(#38171,#38172,#38173),(#38174,
#38175,#38176),(#38177,#38178,#38179),(#38180,#38181,#38182),(#38183,#38184,
#38185),(#38186,#38187,#38188),(#38189,#38190,#38191),(#38192,#38193,#38194),
(#38195,#38196,#38197),(#38198,#38199,#38200),(#38201,#38202,#38203),(#38204,
#38205,#38206),(#38207,#38208,#38209),(#38210,#38211,#38212),(#38213,#38214,
#38215),(#38216,#38217,#38218),(#38219,#38220,#38221),(#38222,#38223,#38224),
(#38225,#38226,#38227),(#38228,#38229,#38230),(#38231,#38232,#38233),(#38234,
#38235,#38236),(#38237,#38238,#38239),(#38240,#38241,#38242),(#38243,#38244,
#38245),(#38246,#38247,#38248),(#38249,#38250,#38251),(#38252,#38253,#38254),
(#38255,#38256,#38257),(#38258,#38259,#38260),(#38261,#38262,#38263),(#38264,
#38265,#38266),(#38267,#38268,#38269),(#38270,#38271,#38272),(#38273,#38274,
#38275),(#38276,#38277,#38278),(#38279,#38280,#38281),(#38282,#38283,#38284),
(#38285,#38286,#38287),(#38288,#38289,#38290),(#38291,#38292,#38293),(#38294,
#38295,#38296),(#38297,#38298,#38299),(#38300,#38301,#38302),(#38303,#38304,
#38305),(#38306,#38307,#38308),(#38309,#38310,#38311),(#38312,#38313,#38314),
(#38315,#38316,#38317),(#38318,#38319,#38320),(#38321,#38322,#38323),(#38324,
#38325,#38326),(#38327,#38328,#38329),(#38330,#38331,#38332),(#38333,#38334,
#38335),(#38336,#38337,#38338),(#38339,#38340,#38341),(#38342,#38343,#38344),
(#38345,#38346,#38347),(#38348,#38349,#38350),(#38351,#38352,#38353),(#38354,
#38355,#38356),(#38357,#38358,#38359),(#38360,#38361,#38362),(#38363,#38364,
#38365),(#38366,#38367,#38368),(#38369,#38370,#38371),(#38372,#38373,#38374),
(#38375,#38376,#38377),(#38378,#38379,#38380),(#38381,#38382,#38383),(#38384,
#38385,#38386),(#38387,#38388,#38389),(#38390,#38391,#38392),(#38393,#38394,
#38395),(#38396,#38397,#38398),(#38399,#38400,#38401),(#38402,#38403,#38404),
(#38405,#38406,#38407),(#38408,#38409,#38410),(#38411,#38412,#38413),(#38414,
#38415,#38416),(#38417,#38418,#38419),(#38420,#38421,#38422),(#38423,#38424,
#38425),(#38426,#38427,#38428),(#38429,#38430,#38431),(#38432,#38433,#38434),
(#38435,#38436,#38437),(#38438,#38439,#38440),(#38441,#38442,#38443),(#38444,
#38445,#38446),(#38447,#38448,#38449),(#38450,#38451,#38452),(#38453,#38454,
#38455),(#38456,#38457,#38458),(#38459,#38460,#38461),(#38462,#38463,#38464),
(#38465,#38466,#38467),(#38468,#38469,#38470),(#38471,#38472,#38473),(#38474,
#38475,#38476),(#38477,#38478,#38479),(#38480,#38481,#38482),(#38483,#38484,
#38485),(#38486,#38487,#38488),(#38489,#38490,#38491),(#38492,#38493,#38494),
(#38495,#38496,#38497),(#38498,#38499,#38500),(#38501,#38502,#38503),(#38504,
#38505,#38506),(#38507,#38508,#38509),(#38510,#38511,#38512),(#38513,#38514,
#38515)),.UNSPECIFIED.,.F.,.F.,.F.)
B_SPLINE_SURFACE_WITH_KNOTS((4,2,2,2,2,2,2,2,2,2,2,2,2,2,2,2,2,2,2,2,2,
2,2,2,2,2,2,2,2,2,2,2,2,2,2,2,2,2,2,2,2,2,2,2,2,2,2,2,2,2,2,2,2,2,2,2,2,
2,2,2,2,2,2,2,2,2,2,2,2,2,2,2,2,2,2,2,2,2,2,2,2,2,2,2,2,2,2,2,2,2,2,2,2,
2,2,2,2,2,2,2,2,2,2,2,2,2,2,2,2,2,2,2,2,2,2,2,2,2,2,2,2,2,2,2,2,2,2,2,2,
2,2,2,2,2,2,2,2,2,2,2,2,2,2,2,2,2,2,2,2,2,2,2,2,2,2,2,2,2,2,2,2,2,2,2,2,
2,2,2,2,2,2,2,4),(3,3),(0.193194020715734,0.19458015398761,0.195966287259486,
0.19735242053136,0.198738553803236,0.201510820346987,0.204283086890738,
0.207055353434488,0.208441486706364,0.209827619978239,0.212599886521989,
0.21537215306574,0.216758286337615,0.218144419609491,0.220916686153242,
0.222302819425117,0.223688952696992,0.226461219240743,0.227847352512619,
0.229233485784493,0.232005752328244,0.234778018871995,0.23616415214387,
0.237550285415745,0.240322551959497,0.241708685231372,0.243094818503247,
0.245867085046998,0.247253218318873,0.248639351590749,0.251411618134499,
0.25418388467825,0.255570017950125,0.256956151222,0.259728417765751,0.261114551037626,
0.262500684309502,0.265272950853253,0.266659084125128,0.268045217397003,
0.270817483940754,0.273589750484505,0.276362017028256,0.279134283572006,
0.280520416843882,0.281906550115756,0.284678816659508,0.286064949931383,
0.287451083203258,0.290223349747009,0.29299561629076,0.29576788283451,0.29854014937826,
0.299926282650136,0.301312415922012,0.304084682465762,0.305470815737638,
0.306856949009513,0.309629215553264,0.312401482097014,0.315173748640765,
0.317946015184516,0.319332148456391,0.320718281728266,0.323490548272017,
0.324876681543892,0.326262814815768,0.329035081359519,0.331807347903269,
0.33457961444702,0.337351880990771,0.338738014262645,0.340124147534521,
0.342896414078271,0.344282547350147,0.345668680622022,0.348440947165773,
0.349827080437648,0.351213213709524,0.353985480253275,0.356757746797025,
0.358143880068901,0.359530013340776,0.362302279884527,0.363688413156402,
0.365074546428277,0.367846812972028,0.369232946243904,0.370619079515778,
0.37339134605953,0.37616361260328,0.37893587914703,0.380322012418906,0.381708145690781,
0.384480412234532,0.387252678778283,0.390024945322034,0.391411078593909,
0.392797211865784,0.395569478409534,0.398341744953286,0.399727878225161,
0.401114011497036,0.403886278040787,0.406658544584537,0.409430811128288,
0.410816944400164,0.412203077672039,0.41497534421579,0.41774761075954,0.419133744031415,
0.420519877303291,0.423292143847042,0.426064410390793,0.428836676934543,
0.430222810206419,0.431608943478294,0.434381210022044,0.437153476565795,
0.43853960983767,0.439925743109545,0.442698009653296,0.444084142925172,
0.445470276197047,0.448242542740798,0.449628676012673,0.451014809284549,
0.453787075828299,0.45655934237205,0.457945475643925,0.459331608915801,
0.462103875459551,0.463490008731427,0.464876142003302,0.467648408547053,
0.469034541818928,0.470420675090803,0.473192941634554,0.475965208178305,
0.47735134145018,0.478737474722055,0.481509741265806,0.482895874537681,
0.484282007809557,0.487054274353307,0.488440407625183,0.489826540897058,
0.492598807440809,0.495371073984559,0.49814334052831,0.500915607072061,
0.502301740343936,0.503687873615812,0.506460140159562,0.507846273431438,
0.509232406703313,0.512004673247064,0.514776939790814,0.517549206334565,
0.520321472878316,0.521707606150191,0.523093739422066,0.525866005965817,
0.527252139237692,0.528638272509568,0.531410539053318,0.534182805597069,
0.53695507214082,0.53972733868457,0.541113471956446,0.542499605228321,0.545271871772072,
0.548044138315822),(0.,1.),.UNSPECIFIED.)
GEOMETRIC_REPRESENTATION_ITEM()
RATIONAL_B_SPLINE_SURFACE(((1.,0.724284384183872,1.),(1.,0.740305127237413,
1.),(1.,0.751232954189051,1.),(1.,0.763742821539273,1.),(1.,0.763748825819259,
1.),(1.,0.763834413771316,1.),(1.,0.763924465861183,1.),(1.,0.764064751530991,
1.),(1.,0.764115143190699,1.),(1.,0.764135968375271,1.),(1.,0.76393847009999,
1.),(1.,0.763675888999986,1.),(1.,0.763876016878027,1.),(1.,0.764321026152726,
1.),(1.,0.764509104980298,1.),(1.,0.76451608219454,1.),(1.,0.76447775031199,
1.),(1.,0.764346212201205,1.),(1.,0.764252566231277,1.),(1.,0.764000135558632,
1.),(1.,0.763965766551896,1.),(1.,0.764364555014901,1.),(1.,0.764630270967712,
1.),(1.,0.764711027046936,1.),(1.,0.764689932612344,1.),(1.,0.764558244124265,
1.),(1.,0.764447962391867,1.),(1.,0.764066111419482,1.),(1.,0.763726565682464,
1.),(1.,0.763796776005459,1.),(1.,0.763904914089681,1.),(1.,0.764157901026904,
1.),(1.,0.764300924283023,1.),(1.,0.764645734647822,1.),(1.,0.764739970352618,
1.),(1.,0.764582273953922,1.),(1.,0.764485721950045,1.),(1.,0.764260579879712,
1.),(1.,0.764131679720444,1.),(1.,0.763860735254699,1.),(1.,0.763994368914939,
1.),(1.,0.764451904711763,1.),(1.,0.764675420085065,1.),(1.,0.764676435702143,
1.),(1.,0.764626319914614,1.),(1.,0.764448678783329,1.),(1.,0.764321322928903,
1.),(1.,0.763928094157012,1.),(1.,0.763678648076241,1.),(1.,0.763890075019292,
1.),(1.,0.764021879641345,1.),(1.,0.764286917309977,1.),(1.,0.764418752057724,
1.),(1.,0.764702707473528,1.),(1.,0.764720013103519,1.),(1.,0.764487759524574,
1.),(1.,0.764373147804989,1.),(1.,0.764141505001544,1.),(1.,0.764024512063168,
1.),(1.,0.763855645361392,1.),(1.,0.764113660855987,1.),(1.,0.764565836609295,
1.),(1.,0.764724131926724,1.),(1.,0.764629033790115,1.),(1.,0.764547656618952,
1.),(1.,0.764326190273316,1.),(1.,0.764186143918983,1.),(1.,0.763805229077168,
1.),(1.,0.763699618536614,1.),(1.,0.764013359048112,1.),(1.,0.764157064792652,
1.),(1.,0.764414467893511,1.),(1.,0.764527285422471,1.),(1.,0.764733735803131,
1.),(1.,0.764672147726954,1.),(1.,0.764378491171655,1.),(1.,0.764252882168725,
1.),(1.,0.764034494546627,1.),(1.,0.763942201634753,1.),(1.,0.763920903382263,
1.),(1.,0.764244527340539,1.),(1.,0.764653633517867,1.),(1.,0.764738192767595,
1.),(1.,0.76448908915439,1.),(1.,0.764159736215753,1.),(1.,0.763716715490157,
1.),(1.,0.76377587103168,1.),(1.,0.764149322081957,1.),(1.,0.764292891647004,
1.),(1.,0.764524133102802,1.),(1.,0.764611439973631,1.),(1.,0.764729271281352,
1.),(1.,0.764592564976275,1.),(1.,0.764259450599018,1.),(1.,0.764132866751854,
1.),(1.,0.763952940534743,1.),(1.,0.763909940937905,1.),(1.,0.764047564751732,
1.),(1.,0.764376050918383,1.),(1.,0.764710874387109,1.),(1.,0.764716717096199,
1.),(1.,0.764358367100507,1.),(1.,0.764002110091814,1.),(1.,0.763678666741915,
1.),(1.,0.763890791093845,1.),(1.,0.764286151554894,1.),(1.,0.76441927129705,
1.),(1.,0.764609474764907,1.),(1.,0.764666635980878,1.),(1.,0.764690318511911,
1.),(1.,0.76448601338486,1.),(1.,0.764140706416799,1.),(1.,0.764024893163625,
1.),(1.,0.763911882511275,1.),(1.,0.763938692841781,1.),(1.,0.764187733769396,
1.),(1.,0.764497658159542,1.),(1.,0.764734199223594,1.),(1.,0.764660097132399,
1.),(1.,0.76421324129478,1.),(1.,0.763851792592164,1.),(1.,0.763708665296719,
1.),(1.,0.764029246906871,1.),(1.,0.764413677710061,1.),(1.,0.76452781916181,
1.),(1.,0.7646658134995,1.),(1.,0.764690072542689,1.),(1.,0.764619697565954,
1.),(1.,0.764359052346609,1.),(1.,0.764034028102741,1.),(1.,0.763942399287252,
1.),(1.,0.763927844141164,1.),(1.,0.764011858926398,1.),(1.,0.764328562594867,
1.),(1.,0.764600555208422,1.),(1.,0.764722148145367,1.),(1.,0.764570469279582,
1.),(1.,0.764063816259676,1.),(1.,0.763726910127108,1.),(1.,0.763819983432828,
1.),(1.,0.76417767845136,1.),(1.,0.764523503616313,1.),(1.,0.76461198390526,
1.),(1.,0.764690348954903,1.),(1.,0.764680836895054,1.),(1.,0.76452210843659,
1.),(1.,0.764220072361436,1.),(1.,0.763952836450435,1.),(1.,0.763909765698979,
1.),(1.,0.764001660074815,1.),(1.,0.764114021416086,1.),(1.,0.764459450111386,
1.),(1.,0.764677768912382,1.),(1.,0.764675817192644,1.),(1.,0.764626188605873,
1.),(1.,0.764448334836733,1.),(1.,0.764319649606282,1.),(1.,0.76392144937362,
1.),(1.,0.763678954739498,1.),(1.,0.763966705816651,1.),(1.,0.764324181625799,
1.),(1.,0.764609052799967,1.),(1.,0.764667080350501,1.),(1.,0.764682173323424,
1.),(1.,0.764639909041378,1.),(1.,0.764404109006945,1.),(1.,0.764079253557161,
1.),(1.,0.76391211996651,1.),(1.,0.763938204725637,1.),(1.,0.764104954676349,
1.),(1.,0.764231320468568,1.),(1.,0.764571581565062,1.),(1.,0.764724181309951,
1.),(1.,0.764627747558348,1.),(1.,0.764547299804896,1.),(1.,0.764325646198393,
1.),(1.,0.764183899644622,1.),(1.,0.763799361853443,1.),(1.,0.763703181785222,
1.),(1.,0.764123550653324,1.),(1.,0.764458577730754,1.),(1.,0.764734613928835,
1.),(1.,0.764669103511761,1.),(1.,0.764367907046241,1.),(1.,0.764240302577737,
1.),(1.,0.76402494244893,1.),(1.,0.763937135559565,1.),(1.,0.763929882961757,
1.),(1.,0.764253286273473,1.),(1.,0.764659669769347,1.),(1.,0.764736610859316,
1.),(1.,0.764478373141418,1.),(1.,0.764149224099175,1.),(1.,0.763821487056611,
1.),(1.,0.763748372230787,1.),(1.,0.763801098390883,1.),(1.,0.763911183371908,
1.),(1.,0.764290057432388,1.),(1.,0.764579381227941,1.),(1.,0.764727426427296,
1.),(1.,0.764586296776282,1.),(1.,0.764248306196083,1.),(1.,0.764120922979176,
1.),(1.,0.763946879813119,1.),(1.,0.763910536288566,1.),(1.,0.764057706241362,
1.),(1.,0.76438462516118,1.),(1.,0.76471447438699,1.),(1.,0.764711120531398,
1.),(1.,0.764346703878295,1.),(1.,0.76399170176065,1.),(1.,0.763756582327334,
1.),(1.,0.763752110504806,1.),(1.,0.763901328422942,1.),(1.,0.764035450100222,
1.),(1.,0.76443236193701,1.),(1.,0.764663646141859,1.),(1.,0.764686363906065,
1.),(1.,0.764477694984837,1.),(1.,0.764129890053359,1.),(1.,0.764014977127996,
1.),(1.,0.763910804517628,1.),(1.,0.763943547724003,1.),(1.,0.764197787087454,
1.),(1.,0.764505416587815,1.),(1.,0.764735065981735,1.),(1.,0.764650795813227,
1.),(1.,0.764201499620299,1.),(1.,0.763842254050267,1.),(1.,0.763745729500901,
1.),(1.,0.76381182195424,1.),(1.,0.76402644812972,1.),(1.,0.764171057297587,
1.),(1.,0.764553541563368,1.),(1.,0.764715935999787,1.),(1.,0.764613884843303,
1.),(1.,0.764349088181113,1.),(1.,0.764024757422653,1.),(1.,0.763936087572711,
1.),(1.,0.763933281394626,1.),(1.,0.764019522637573,1.),(1.,0.764337859143539,
1.),(1.,0.764606969286635,1.),(1.,0.764691835149024,1.),(1.,0.764672390149729,
1.),(1.,0.764541959203006,1.),(1.,0.764431856676212,1.),(1.,0.764052655452415,
1.),(1.,0.763720892206212,1.),(1.,0.763802318721878,1.),(1.,0.763911148353123,
1.),(1.,0.764163074576283,1.),(1.,0.76430628255999,1.),(1.,0.764647184874934,
1.),(1.,0.764733604516214,1.),(1.,0.7645148011791,1.),(1.,0.764209006825961,
1.),(1.,0.763946554515086,1.),(1.,0.763910418541632,1.),(1.,0.764010587040542,
1.),(1.,0.764123233796092,1.),(1.,0.764467443928139,1.),(1.,0.764682413968858,
1.),(1.,0.76467328554026,1.),(1.,0.764620305145998,1.),(1.,0.764436387977514,
1.),(1.,0.764306466960175,1.),(1.,0.763911800910976,1.),(1.,0.763678258157877,
1.),(1.,0.763902697590758,1.),(1.,0.764035192882901,1.),(1.,0.764299476715184,
1.),(1.,0.764431141631408,1.),(1.,0.764708752226097,1.),(1.,0.764715902370825,
1.),(1.,0.764395783925963,1.),(1.,0.764067776783428,1.),(1.,0.763910501816556,
1.),(1.,0.763944254604468,1.),(1.,0.764115592875844,1.),(1.,0.764241007152287,
1.),(1.,0.764577846837585,1.),(1.,0.764726738859265,1.),(1.,0.764622633857058,
1.),(1.,0.764538607993317,1.),(1.,0.764312012546189,1.),(1.,0.764170421879028,
1.),(1.,0.763792232864636,1.),(1.,0.76370659012842,1.),(1.,0.764027763125852,
1.),(1.,0.764170621154752,1.),(1.,0.764425646706682,1.),(1.,0.764537442869453,
1.),(1.,0.764735596081267,1.),(1.,0.764663981931681,1.),(1.,0.764265331217681,
1.),(1.,0.763937466031569,1.),(1.,0.763931901903142,1.),(1.,0.764260343346382,
1.),(1.,0.764662203747841,1.),(1.,0.764736820790307,1.),(1.,0.764542417955957,
1.),(1.,0.764431774438024,1.),(1.,0.764176976560631,1.),(1.,0.764033631618057,
1.),(1.,0.763708839179177,1.),(1.,0.76378808686829,1.),(1.,0.764164189211495,
1.),(1.,0.764305748334095,1.),(1.,0.764533380352393,1.),(1.,0.764618865966987,
1.),(1.,0.764727061043886,1.),(1.,0.76458103112283,1.),(1.,0.764133984783778,
1.),(1.,0.763859901665259,1.),(1.,0.76406202396653,1.),(1.,0.764391062212757,
1.),(1.,0.76471420648425,1.),(1.,0.764709508679019,1.),(1.,0.764434815138151,
1.),(1.,0.764303896710659,1.),(1.,0.764039283569035,1.),(1.,0.763906140471446,
1.),(1.,0.763678071029506,1.),(1.,0.763907797434181,1.),(1.,0.764300330435456,
1.),(1.,0.764429809231862,1.),(1.,0.764613336272094,1.),(1.,0.764666656725297,
1.),(1.,0.764675678313187,1.),(1.,0.764459912120916,1.),(1.,0.763994763845434,
1.),(1.,0.763828888332753,1.),(1.,0.764197718857373,1.),(1.,0.764534267618665,
1.),(1.,0.764803818543527,1.),(1.,0.764737840759975,1.),(1.,0.764395415450403,
1.),(1.,0.764246141205225,1.),(1.,0.76396864128702,1.),(1.,0.763840712706475,
1.),(1.,0.763683379268838,1.),(1.,0.763772086503981,1.),(1.,0.763779013551137,
1.),(1.,0.763732611162939,1.),(1.,0.763723138090074,1.)))
REPRESENTATION_ITEM('')
SURFACE()
);
#12690=(
BOUNDED_SURFACE()
B_SPLINE_SURFACE(3,2,((#38707,#38708,#38709),(#38710,#38711,#38712),(#38713,
#38714,#38715),(#38716,#38717,#38718)),.UNSPECIFIED.,.F.,.F.,.F.)
B_SPLINE_SURFACE_WITH_KNOTS((4,4),(3,3),(0.00258460052115835,0.00277094492006339),
(0.188652408414785,1.),.PIECEWISE_BEZIER_KNOTS.)
GEOMETRIC_REPRESENTATION_ITEM()
RATIONAL_B_SPLINE_SURFACE(((0.911321524900829,0.764968611203214,1.),(0.911099518239721,
0.764380209859776,1.),(0.910872217507487,0.763777777232107,1.),(0.910640530053848,
0.763163718139024,1.)))
REPRESENTATION_ITEM('')
SURFACE()
);
#12691=(
BOUNDED_SURFACE()
B_SPLINE_SURFACE(3,2,((#38730,#38731,#38732),(#38733,#38734,#38735),(#38736,
#38737,#38738),(#38739,#38740,#38741),(#38742,#38743,#38744),(#38745,#38746,
#38747),(#38748,#38749,#38750),(#38751,#38752,#38753),(#38754,#38755,#38756),
(#38757,#38758,#38759)),.UNSPECIFIED.,.F.,.F.,.F.)
B_SPLINE_SURFACE_WITH_KNOTS((4,2,2,2,4),(3,3),(0.0442495418135926,0.0460556664569336,
0.0478617911002747,0.0496679157436157,0.0514740403869568),(0.,1.),
 .UNSPECIFIED.)
GEOMETRIC_REPRESENTATION_ITEM()
RATIONAL_B_SPLINE_SURFACE(((1.,0.763723138090958,1.),(1.,0.757306565135894,
1.),(1.,0.751046655980244,1.),(1.,0.738750551500846,1.),(1.,0.732694138219894,
1.),(1.,0.720501130718487,1.),(1.,0.714363531034312,1.),(1.,0.702102216800646,
1.),(1.,0.696457132575243,1.),(1.,0.689508268890299,1.)))
REPRESENTATION_ITEM('')
SURFACE()
);
#12692=(
BOUNDED_SURFACE()
B_SPLINE_SURFACE(3,3,((#38826,#38827,#38828,#38829,#38830,#38831,#38832,
#38833,#38834,#38835,#38836,#38837,#38838,#38839,#38840,#38841,#38842,#38843,
#38844,#38845,#38846,#38847,#38848,#38849,#38850,#38851,#38852,#38853,#38854,
#38855,#38856,#38857,#38858,#38859,#38860,#38861,#38862,#38863,#38864,#38865,
#38866,#38867,#38868,#38869,#38870,#38871,#38872,#38873,#38874,#38875,#38876,
#38877,#38878,#38879,#38880,#38881,#38882,#38883,#38884,#38885,#38886,#38887,
#38888,#38889,#38890,#38891,#38892,#38893,#38894,#38895,#38896,#38897,#38898,
#38899,#38900,#38901,#38902,#38903,#38904,#38905,#38906,#38907,#38908,#38909,
#38910,#38911),(#38912,#38913,#38914,#38915,#38916,#38917,#38918,#38919,
#38920,#38921,#38922,#38923,#38924,#38925,#38926,#38927,#38928,#38929,#38930,
#38931,#38932,#38933,#38934,#38935,#38936,#38937,#38938,#38939,#38940,#38941,
#38942,#38943,#38944,#38945,#38946,#38947,#38948,#38949,#38950,#38951,#38952,
#38953,#38954,#38955,#38956,#38957,#38958,#38959,#38960,#38961,#38962,#38963,
#38964,#38965,#38966,#38967,#38968,#38969,#38970,#38971,#38972,#38973,#38974,
#38975,#38976,#38977,#38978,#38979,#38980,#38981,#38982,#38983,#38984,#38985,
#38986,#38987,#38988,#38989,#38990,#38991,#38992,#38993,#38994,#38995,#38996,
#38997),(#38998,#38999,#39000,#39001,#39002,#39003,#39004,#39005,#39006,
#39007,#39008,#39009,#39010,#39011,#39012,#39013,#39014,#39015,#39016,#39017,
#39018,#39019,#39020,#39021,#39022,#39023,#39024,#39025,#39026,#39027,#39028,
#39029,#39030,#39031,#39032,#39033,#39034,#39035,#39036,#39037,#39038,#39039,
#39040,#39041,#39042,#39043,#39044,#39045,#39046,#39047,#39048,#39049,#39050,
#39051,#39052,#39053,#39054,#39055,#39056,#39057,#39058,#39059,#39060,#39061,
#39062,#39063,#39064,#39065,#39066,#39067,#39068,#39069,#39070,#39071,#39072,
#39073,#39074,#39075,#39076,#39077,#39078,#39079,#39080,#39081,#39082,#39083),
(#39084,#39085,#39086,#39087,#39088,#39089,#39090,#39091,#39092,#39093,
#39094,#39095,#39096,#39097,#39098,#39099,#39100,#39101,#39102,#39103,#39104,
#39105,#39106,#39107,#39108,#39109,#39110,#39111,#39112,#39113,#39114,#39115,
#39116,#39117,#39118,#39119,#39120,#39121,#39122,#39123,#39124,#39125,#39126,
#39127,#39128,#39129,#39130,#39131,#39132,#39133,#39134,#39135,#39136,#39137,
#39138,#39139,#39140,#39141,#39142,#39143,#39144,#39145,#39146,#39147,#39148,
#39149,#39150,#39151,#39152,#39153,#39154,#39155,#39156,#39157,#39158,#39159,
#39160,#39161,#39162,#39163,#39164,#39165,#39166,#39167,#39168,#39169),
(#39170,#39171,#39172,#39173,#39174,#39175,#39176,#39177,#39178,#39179,
#39180,#39181,#39182,#39183,#39184,#39185,#39186,#39187,#39188,#39189,#39190,
#39191,#39192,#39193,#39194,#39195,#39196,#39197,#39198,#39199,#39200,#39201,
#39202,#39203,#39204,#39205,#39206,#39207,#39208,#39209,#39210,#39211,#39212,
#39213,#39214,#39215,#39216,#39217,#39218,#39219,#39220,#39221,#39222,#39223,
#39224,#39225,#39226,#39227,#39228,#39229,#39230,#39231,#39232,#39233,#39234,
#39235,#39236,#39237,#39238,#39239,#39240,#39241,#39242,#39243,#39244,#39245,
#39246,#39247,#39248,#39249,#39250,#39251,#39252,#39253,#39254,#39255),
(#39256,#39257,#39258,#39259,#39260,#39261,#39262,#39263,#39264,#39265,
#39266,#39267,#39268,#39269,#39270,#39271,#39272,#39273,#39274,#39275,#39276,
#39277,#39278,#39279,#39280,#39281,#39282,#39283,#39284,#39285,#39286,#39287,
#39288,#39289,#39290,#39291,#39292,#39293,#39294,#39295,#39296,#39297,#39298,
#39299,#39300,#39301,#39302,#39303,#39304,#39305,#39306,#39307,#39308,#39309,
#39310,#39311,#39312,#39313,#39314,#39315,#39316,#39317,#39318,#39319,#39320,
#39321,#39322,#39323,#39324,#39325,#39326,#39327,#39328,#39329,#39330,#39331,
#39332,#39333,#39334,#39335,#39336,#39337,#39338,#39339,#39340,#39341),
(#39342,#39343,#39344,#39345,#39346,#39347,#39348,#39349,#39350,#39351,
#39352,#39353,#39354,#39355,#39356,#39357,#39358,#39359,#39360,#39361,#39362,
#39363,#39364,#39365,#39366,#39367,#39368,#39369,#39370,#39371,#39372,#39373,
#39374,#39375,#39376,#39377,#39378,#39379,#39380,#39381,#39382,#39383,#39384,
#39385,#39386,#39387,#39388,#39389,#39390,#39391,#39392,#39393,#39394,#39395,
#39396,#39397,#39398,#39399,#39400,#39401,#39402,#39403,#39404,#39405,#39406,
#39407,#39408,#39409,#39410,#39411,#39412,#39413,#39414,#39415,#39416,#39417,
#39418,#39419,#39420,#39421,#39422,#39423,#39424,#39425,#39426,#39427)),
 .UNSPECIFIED.,.F.,.F.,.F.)
B_SPLINE_SURFACE_WITH_KNOTS((4,3,4),(4,3,2,2,2,2,2,2,2,2,2,2,2,2,2,2,2,
2,2,2,2,2,2,2,2,2,2,2,2,2,2,2,2,2,2,2,2,2,2,2,3,4),(0.768207327186719,1.,
1.23184820212984),(-0.00600749857863525,0.,0.0175438596491217,0.0438596491228064,
0.0701754385964912,0.0964912280701754,0.12280701754386,0.149122807017537,
0.175438596491214,0.201754385964905,0.228070175438597,0.25438596491228,
0.280701754385965,0.307017543859649,0.333333333333333,0.359649122807017,
0.385964912280702,0.412280701754386,0.43859649122807,0.464912280701754,
0.491228070175438,0.517543859649124,0.54385964912281,0.570175438596493,
0.596491228070175,0.62280701754386,0.649122807017544,0.675438596491228,
0.701754385964912,0.728070175438596,0.754385964912281,0.780701754385965,
0.807017543859649,0.833333333333333,0.859649122807018,0.885964912280702,
0.912280701754386,0.93859649122807,0.964912280701754,0.982456140350877,
1.,1.00600726704965),.UNSPECIFIED.)
GEOMETRIC_REPRESENTATION_ITEM()
RATIONAL_B_SPLINE_SURFACE(((0.502652054106274,0.502652054106274,0.502652054106274,
0.502652054106274,0.502652054106274,0.502652054106274,0.502652054106274,
0.502652054106274,0.502652054106274,0.502652054106274,0.502652054106274,
0.502652054106274,0.502652054106274,0.502652054106274,0.502652054106274,
0.502652054106274,0.502652054106274,0.502652054106274,0.502652054106274,
0.502652054106274,0.502652054106274,0.502652054106274,0.502652054106274,
0.502652054106274,0.502652054106274,0.502652054106274,0.502652054106274,
0.502652054106274,0.502652054106274,0.502652054106274,0.502652054106274,
0.502652054106274,0.502652054106274,0.502652054106274,0.502652054106274,
0.502652054106274,0.502652054106274,0.502652054106274,0.502652054106274,
0.502652054106274,0.502652054106274,0.502652054106274,0.502652054106274,
0.502652054106274,0.502652054106274,0.502652054106274,0.502652054106274,
0.502652054106274,0.502652054106274,0.502652054106274,0.502652054106274,
0.502652054106274,0.502652054106274,0.502652054106274,0.502652054106274,
0.502652054106274,0.502652054106274,0.502652054106274,0.502652054106274,
0.502652054106274,0.502652054106274,0.502652054106274,0.502652054106274,
0.502652054106274,0.502652054106274,0.502652054106274,0.502652054106274,
0.502652054106274,0.502652054106274,0.502652054106274,0.502652054106274,
0.502652054106274,0.502652054106274,0.502652054106274,0.502652054106274,
0.502652054106274,0.502652054106274,0.502652054106274,0.502652054106274,
0.502652054106274,0.502652054106274,0.502652054106274,0.502652054106274,
0.502652054106274,0.502652054106274,0.502652054106274),(0.525160454284383,
0.525160454284383,0.525160454284383,0.525160454284383,0.525160454284383,
0.525160454284383,0.525160454284383,0.525160454284383,0.525160454284383,
0.525160454284383,0.525160454284383,0.525160454284383,0.525160454284383,
0.525160454284383,0.525160454284383,0.525160454284383,0.525160454284383,
0.525160454284383,0.525160454284383,0.525160454284383,0.525160454284383,
0.525160454284383,0.525160454284383,0.525160454284383,0.525160454284383,
0.525160454284383,0.525160454284383,0.525160454284383,0.525160454284383,
0.525160454284383,0.525160454284383,0.525160454284383,0.525160454284383,
0.525160454284383,0.525160454284383,0.525160454284383,0.525160454284383,
0.525160454284383,0.525160454284383,0.525160454284383,0.525160454284383,
0.525160454284383,0.525160454284383,0.525160454284383,0.525160454284383,
0.525160454284383,0.525160454284383,0.525160454284383,0.525160454284383,
0.525160454284383,0.525160454284383,0.525160454284383,0.525160454284383,
0.525160454284383,0.525160454284383,0.525160454284383,0.525160454284383,
0.525160454284383,0.525160454284383,0.525160454284383,0.525160454284383,
0.525160454284383,0.525160454284383,0.525160454284383,0.525160454284383,
0.525160454284383,0.525160454284383,0.525160454284383,0.525160454284383,
0.525160454284383,0.525160454284383,0.525160454284383,0.525160454284383,
0.525160454284383,0.525160454284383,0.525160454284383,0.525160454284383,
0.525160454284383,0.525160454284383,0.525160454284383,0.525160454284383,
0.525160454284383,0.525160454284383,0.525160454284383,0.525160454284383,
0.525160454284383),(0.690943102915625,0.690943102915625,0.690943102915625,
0.690943102915625,0.690943102915625,0.690943102915625,0.690943102915625,
0.690943102915625,0.690943102915625,0.690943102915625,0.690943102915625,
0.690943102915625,0.690943102915625,0.690943102915625,0.690943102915625,
0.690943102915625,0.690943102915625,0.690943102915625,0.690943102915625,
0.690943102915625,0.690943102915625,0.690943102915625,0.690943102915625,
0.690943102915625,0.690943102915625,0.690943102915625,0.690943102915625,
0.690943102915625,0.690943102915625,0.690943102915625,0.690943102915625,
0.690943102915625,0.690943102915625,0.690943102915625,0.690943102915625,
0.690943102915625,0.690943102915625,0.690943102915625,0.690943102915625,
0.690943102915625,0.690943102915625,0.690943102915625,0.690943102915625,
0.690943102915625,0.690943102915625,0.690943102915625,0.690943102915625,
0.690943102915625,0.690943102915625,0.690943102915625,0.690943102915625,
0.690943102915625,0.690943102915625,0.690943102915625,0.690943102915625,
0.690943102915625,0.690943102915625,0.690943102915625,0.690943102915625,
0.690943102915625,0.690943102915625,0.690943102915625,0.690943102915625,
0.690943102915625,0.690943102915625,0.690943102915625,0.690943102915625,
0.690943102915625,0.690943102915625,0.690943102915625,0.690943102915625,
0.690943102915625,0.690943102915625,0.690943102915625,0.690943102915625,
0.690943102915625,0.690943102915625,0.690943102915625,0.690943102915625,
0.690943102915625,0.690943102915625,0.690943102915625,0.690943102915625,
0.690943102915625,0.690943102915625,0.690943102915625),(1.,1.,1.,1.,1.,
1.,1.,1.,1.,1.,1.,1.,1.,1.,1.,1.,1.,1.,1.,1.,1.,1.,1.,1.,1.,1.,1.,1.,1.,
1.,1.,1.,1.,1.,1.,1.,1.,1.,1.,1.,1.,1.,1.,1.,1.,1.,1.,1.,1.,1.,1.,1.,1.,
1.,1.,1.,1.,1.,1.,1.,1.,1.,1.,1.,1.,1.,1.,1.,1.,1.,1.,1.,1.,1.,1.,1.,1.,
1.,1.,1.,1.,1.,1.,1.,1.,1.),(0.690869063826886,0.690869063826886,0.690869063826886,
0.690869063826886,0.690869063826886,0.690869063826886,0.690869063826886,
0.690869063826886,0.690869063826886,0.690869063826886,0.690869063826886,
0.690869063826886,0.690869063826886,0.690869063826886,0.690869063826886,
0.690869063826886,0.690869063826886,0.690869063826886,0.690869063826886,
0.690869063826886,0.690869063826886,0.690869063826886,0.690869063826886,
0.690869063826886,0.690869063826886,0.690869063826886,0.690869063826886,
0.690869063826886,0.690869063826886,0.690869063826886,0.690869063826886,
0.690869063826886,0.690869063826886,0.690869063826886,0.690869063826886,
0.690869063826886,0.690869063826886,0.690869063826886,0.690869063826886,
0.690869063826886,0.690869063826886,0.690869063826886,0.690869063826886,
0.690869063826886,0.690869063826886,0.690869063826886,0.690869063826886,
0.690869063826886,0.690869063826886,0.690869063826886,0.690869063826886,
0.690869063826886,0.690869063826886,0.690869063826886,0.690869063826886,
0.690869063826886,0.690869063826886,0.690869063826886,0.690869063826886,
0.690869063826886,0.690869063826886,0.690869063826886,0.690869063826886,
0.690869063826886,0.690869063826886,0.690869063826886,0.690869063826886,
0.690869063826886,0.690869063826886,0.690869063826886,0.690869063826886,
0.690869063826886,0.690869063826886,0.690869063826886,0.690869063826886,
0.690869063826886,0.690869063826886,0.690869063826886,0.690869063826886,
0.690869063826886,0.690869063826886,0.690869063826886,0.690869063826886,
0.690869063826886,0.690869063826886,0.690869063826886),(0.525081031202671,
0.525081031202671,0.525081031202671,0.525081031202671,0.525081031202671,
0.525081031202671,0.525081031202671,0.525081031202671,0.525081031202671,
0.525081031202671,0.525081031202671,0.525081031202671,0.525081031202671,
0.525081031202671,0.525081031202671,0.525081031202671,0.525081031202671,
0.525081031202671,0.525081031202671,0.525081031202671,0.525081031202671,
0.525081031202671,0.525081031202671,0.525081031202671,0.525081031202671,
0.525081031202671,0.525081031202671,0.525081031202671,0.525081031202671,
0.525081031202671,0.525081031202671,0.525081031202671,0.525081031202671,
0.525081031202671,0.525081031202671,0.525081031202671,0.525081031202671,
0.525081031202671,0.525081031202671,0.525081031202671,0.525081031202671,
0.525081031202671,0.525081031202671,0.525081031202671,0.525081031202671,
0.525081031202671,0.525081031202671,0.525081031202671,0.525081031202671,
0.525081031202671,0.525081031202671,0.525081031202671,0.525081031202671,
0.525081031202671,0.525081031202671,0.525081031202671,0.525081031202671,
0.525081031202671,0.525081031202671,0.525081031202671,0.525081031202671,
0.525081031202671,0.525081031202671,0.525081031202671,0.525081031202671,
0.525081031202671,0.525081031202671,0.525081031202671,0.525081031202671,
0.525081031202671,0.525081031202671,0.525081031202671,0.525081031202671,
0.525081031202671,0.525081031202671,0.525081031202671,0.525081031202671,
0.525081031202671,0.525081031202671,0.525081031202671,0.525081031202671,
0.525081031202671,0.525081031202671,0.525081031202671,0.525081031202671,
0.525081031202671),(0.502635902127355,0.502635902127355,0.502635902127355,
0.502635902127355,0.502635902127355,0.502635902127355,0.502635902127355,
0.502635902127355,0.502635902127355,0.502635902127355,0.502635902127355,
0.502635902127355,0.502635902127355,0.502635902127355,0.502635902127355,
0.502635902127355,0.502635902127355,0.502635902127355,0.502635902127355,
0.502635902127355,0.502635902127355,0.502635902127355,0.502635902127355,
0.502635902127355,0.502635902127355,0.502635902127355,0.502635902127355,
0.502635902127355,0.502635902127355,0.502635902127355,0.502635902127355,
0.502635902127355,0.502635902127355,0.502635902127355,0.502635902127355,
0.502635902127355,0.502635902127355,0.502635902127355,0.502635902127355,
0.502635902127355,0.502635902127355,0.502635902127355,0.502635902127355,
0.502635902127355,0.502635902127355,0.502635902127355,0.502635902127355,
0.502635902127355,0.502635902127355,0.502635902127355,0.502635902127355,
0.502635902127355,0.502635902127355,0.502635902127355,0.502635902127355,
0.502635902127355,0.502635902127355,0.502635902127355,0.502635902127355,
0.502635902127355,0.502635902127355,0.502635902127355,0.502635902127355,
0.502635902127355,0.502635902127355,0.502635902127355,0.502635902127355,
0.502635902127355,0.502635902127355,0.502635902127355,0.502635902127355,
0.502635902127355,0.502635902127355,0.502635902127355,0.502635902127355,
0.502635902127355,0.502635902127355,0.502635902127355,0.502635902127355,
0.502635902127355,0.502635902127355,0.502635902127355,0.502635902127355,
0.502635902127355,0.502635902127355,0.502635902127355)))
REPRESENTATION_ITEM('')
SURFACE()
);
#12693=(
BOUNDED_SURFACE()
B_SPLINE_SURFACE(1,2,((#39571,#39572,#39573,#39574,#39575,#39576,#39577,
#39578,#39579,#39580,#39581,#39582,#39583,#39584,#39585,#39586,#39587,#39588,
#39589,#39590,#39591,#39592,#39593,#39594,#39595,#39596,#39597,#39598,#39599,
#39600,#39601,#39602,#39603,#39604,#39605,#39606,#39607,#39608,#39609,#39610,
#39611,#39612,#39613,#39614,#39615,#39616,#39617,#39618,#39619,#39620,#39621,
#39622,#39623,#39624,#39625,#39626,#39627,#39628,#39629,#39630,#39631,#39632,
#39633,#39634,#39635,#39636,#39637,#39638,#39639,#39640,#39641,#39642,#39643,
#39644,#39645,#39646,#39647,#39648,#39649),(#39650,#39651,#39652,#39653,
#39654,#39655,#39656,#39657,#39658,#39659,#39660,#39661,#39662,#39663,#39664,
#39665,#39666,#39667,#39668,#39669,#39670,#39671,#39672,#39673,#39674,#39675,
#39676,#39677,#39678,#39679,#39680,#39681,#39682,#39683,#39684,#39685,#39686,
#39687,#39688,#39689,#39690,#39691,#39692,#39693,#39694,#39695,#39696,#39697,
#39698,#39699,#39700,#39701,#39702,#39703,#39704,#39705,#39706,#39707,#39708,
#39709,#39710,#39711,#39712,#39713,#39714,#39715,#39716,#39717,#39718,#39719,
#39720,#39721,#39722,#39723,#39724,#39725,#39726,#39727,#39728)),
 .RULED_SURF.,.F.,.F.,.F.)
B_SPLINE_SURFACE_WITH_KNOTS((2,2),(3,2,2,2,2,2,2,2,2,2,2,2,2,2,2,2,2,2,
2,2,2,2,2,2,2,2,2,2,2,2,2,2,2,2,2,2,2,2,2,3),(0.,1.),(0.,0.025,0.05,0.075,
0.1,0.125,0.15,0.175,0.2,0.225,0.25,0.275,0.3,0.325,0.35,0.375,0.4,0.425,
0.45,0.475,0.5,0.525,0.55,0.575,0.6,0.625,0.65,0.675,0.7,0.725,0.75,0.775,
0.8,0.825,0.85,0.875,0.9,0.925,0.95,0.9645502840563),.UNSPECIFIED.)
GEOMETRIC_REPRESENTATION_ITEM()
RATIONAL_B_SPLINE_SURFACE(((1.,0.951056516295154,1.,0.951056516295154,1.,
0.951056516295154,1.,0.951056516295154,1.,0.951056516295154,1.,0.951056516295154,
1.,0.951056516295154,1.,0.951056516295154,1.,0.951056516295154,1.,0.951056516295154,
1.,0.951056516295154,1.,0.951056516295154,1.,0.951056516295154,1.,0.951056516295154,
1.,0.951056516295154,1.,0.951056516295154,1.,0.951056516295154,1.,0.951056516295154,
1.,0.951056516295154,1.,0.951056516295154,1.,0.951056516295154,1.,0.951056516295154,
1.,0.951056516295154,1.,0.951056516295154,1.,0.951056516295154,1.,0.951056516295154,
1.,0.951056516295154,1.,0.951056516295154,1.,0.951056516295154,1.,0.951056516295154,
1.,0.951056516295154,1.,0.951056516295154,1.,0.951056516295154,1.,0.951056516295154,
1.,0.951056516295154,1.,0.951056516295154,1.,0.951056516295154,1.,0.951056516295154,
1.,0.971514336375583,0.976186632532565),(1.,0.951056516295154,1.,0.951056516295154,
1.,0.951056516295154,1.,0.951056516295154,1.,0.951056516295154,1.,0.951056516295154,
1.,0.951056516295154,1.,0.951056516295154,1.,0.951056516295154,1.,0.951056516295154,
1.,0.951056516295154,1.,0.951056516295154,1.,0.951056516295154,1.,0.951056516295154,
1.,0.951056516295154,1.,0.951056516295154,1.,0.951056516295154,1.,0.951056516295154,
1.,0.951056516295154,1.,0.951056516295154,1.,0.951056516295154,1.,0.951056516295154,
1.,0.951056516295154,1.,0.951056516295154,1.,0.951056516295154,1.,0.951056516295154,
1.,0.951056516295154,1.,0.951056516295154,1.,0.951056516295154,1.,0.951056516295154,
1.,0.951056516295154,1.,0.951056516295154,1.,0.951056516295154,1.,0.951056516295154,
1.,0.951056516295154,1.,0.951056516295154,1.,0.951056516295154,1.,0.951056516295154,
1.,0.971514336375583,0.976186632532565)))
REPRESENTATION_ITEM('')
SURFACE()
);
#12694=(
BOUNDED_SURFACE()
B_SPLINE_SURFACE(1,2,((#39925,#39926,#39927,#39928,#39929,#39930,#39931,
#39932,#39933,#39934,#39935,#39936,#39937,#39938,#39939,#39940,#39941,#39942,
#39943,#39944,#39945,#39946,#39947,#39948,#39949,#39950,#39951,#39952,#39953,
#39954,#39955,#39956,#39957,#39958,#39959,#39960,#39961,#39962,#39963,#39964,
#39965,#39966,#39967,#39968,#39969,#39970,#39971,#39972,#39973,#39974,#39975,
#39976,#39977,#39978,#39979,#39980,#39981,#39982,#39983,#39984,#39985,#39986,
#39987,#39988,#39989,#39990,#39991,#39992,#39993,#39994,#39995,#39996,#39997,
#39998,#39999,#40000,#40001,#40002,#40003,#40004,#40005),(#40006,#40007,
#40008,#40009,#40010,#40011,#40012,#40013,#40014,#40015,#40016,#40017,#40018,
#40019,#40020,#40021,#40022,#40023,#40024,#40025,#40026,#40027,#40028,#40029,
#40030,#40031,#40032,#40033,#40034,#40035,#40036,#40037,#40038,#40039,#40040,
#40041,#40042,#40043,#40044,#40045,#40046,#40047,#40048,#40049,#40050,#40051,
#40052,#40053,#40054,#40055,#40056,#40057,#40058,#40059,#40060,#40061,#40062,
#40063,#40064,#40065,#40066,#40067,#40068,#40069,#40070,#40071,#40072,#40073,
#40074,#40075,#40076,#40077,#40078,#40079,#40080,#40081,#40082,#40083,#40084,
#40085,#40086),(#40087,#40088,#40089,#40090,#40091,#40092,#40093,#40094,
#40095,#40096,#40097,#40098,#40099,#40100,#40101,#40102,#40103,#40104,#40105,
#40106,#40107,#40108,#40109,#40110,#40111,#40112,#40113,#40114,#40115,#40116,
#40117,#40118,#40119,#40120,#40121,#40122,#40123,#40124,#40125,#40126,#40127,
#40128,#40129,#40130,#40131,#40132,#40133,#40134,#40135,#40136,#40137,#40138,
#40139,#40140,#40141,#40142,#40143,#40144,#40145,#40146,#40147,#40148,#40149,
#40150,#40151,#40152,#40153,#40154,#40155,#40156,#40157,#40158,#40159,#40160,
#40161,#40162,#40163,#40164,#40165,#40166,#40167)),.RULED_SURF.,.F.,.F.,
 .F.)
B_SPLINE_SURFACE_WITH_KNOTS((2,1,2),(3,2,2,2,2,2,2,2,2,2,2,2,2,2,2,2,2,
2,2,2,2,2,2,2,2,2,2,2,2,2,2,2,2,2,2,2,2,2,2,2,3),(0.,1.,1.00600024802407),
(0.,0.025,0.05,0.075,0.1,0.125,0.15,0.175,0.2,0.225,0.25,0.275,0.3,0.325,
0.35,0.375,0.4,0.425,0.45,0.475,0.5,0.525,0.55,0.575,0.6,0.625,0.65,0.675,
0.7,0.725,0.75,0.775,0.8,0.825,0.85,0.875,0.9,0.925,0.95,0.964550250376854,
0.970337664573057),.PIECEWISE_BEZIER_KNOTS.)
GEOMETRIC_REPRESENTATION_ITEM()
RATIONAL_B_SPLINE_SURFACE(((1.,0.951056516295154,1.,0.951056516295154,1.,
0.951056516295154,1.,0.951056516295154,1.,0.951056516295154,1.,0.951056516295154,
1.,0.951056516295154,1.,0.951056516295154,1.,0.951056516295154,1.,0.951056516295154,
1.,0.951056516295154,1.,0.951056516295154,1.,0.951056516295154,1.,0.951056516295154,
1.,0.951056516295154,1.,0.951056516295154,1.,0.951056516295154,1.,0.951056516295154,
1.,0.951056516295154,1.,0.951056516295154,1.,0.951056516295154,1.,0.951056516295154,
1.,0.951056516295154,1.,0.951056516295154,1.,0.951056516295154,1.,0.951056516295154,
1.,0.951056516295154,1.,0.951056516295154,1.,0.951056516295154,1.,0.951056516295154,
1.,0.951056516295154,1.,0.951056516295154,1.,0.951056516295154,1.,0.951056516295154,
1.,0.951056516295154,1.,0.951056516295154,1.,0.951056516295154,1.,0.951056516295154,
1.,0.971514402311161,0.976186610902877,0.976186610902877,0.976186610902877),
(1.,0.951056516295154,1.,0.951056516295154,1.,0.951056516295154,1.,0.951056516295154,
1.,0.951056516295154,1.,0.951056516295154,1.,0.951056516295154,1.,0.951056516295154,
1.,0.951056516295154,1.,0.951056516295154,1.,0.951056516295154,1.,0.951056516295154,
1.,0.951056516295154,1.,0.951056516295154,1.,0.951056516295154,1.,0.951056516295154,
1.,0.951056516295154,1.,0.951056516295154,1.,0.951056516295154,1.,0.951056516295154,
1.,0.951056516295154,1.,0.951056516295154,1.,0.951056516295154,1.,0.951056516295154,
1.,0.951056516295154,1.,0.951056516295154,1.,0.951056516295154,1.,0.951056516295154,
1.,0.951056516295154,1.,0.951056516295154,1.,0.951056516295154,1.,0.951056516295154,
1.,0.951056516295154,1.,0.951056516295154,1.,0.951056516295154,1.,0.951056516295154,
1.,0.951056516295154,1.,0.951056516295154,1.,0.971514402311161,0.976186610902877,
0.976186610902877,0.976186610902877),(1.,0.951056516295154,1.,0.951056516295154,
1.,0.951056516295154,1.,0.951056516295154,1.,0.951056516295154,1.,0.951056516295154,
1.,0.951056516295154,1.,0.951056516295154,1.,0.951056516295154,1.,0.951056516295154,
1.,0.951056516295154,1.,0.951056516295154,1.,0.951056516295154,1.,0.951056516295154,
1.,0.951056516295154,1.,0.951056516295154,1.,0.951056516295154,1.,0.951056516295154,
1.,0.951056516295154,1.,0.951056516295154,1.,0.951056516295154,1.,0.951056516295154,
1.,0.951056516295154,1.,0.951056516295154,1.,0.951056516295154,1.,0.951056516295154,
1.,0.951056516295154,1.,0.951056516295154,1.,0.951056516295154,1.,0.951056516295154,
1.,0.951056516295154,1.,0.951056516295154,1.,0.951056516295154,1.,0.951056516295154,
1.,0.951056516295154,1.,0.951056516295154,1.,0.951056516295154,1.,0.951056516295154,
1.,0.971514402311161,0.976186610902877,0.976186610902877,0.976186610902877)))
REPRESENTATION_ITEM('')
SURFACE()
);
#12695=(
BOUNDED_SURFACE()
B_SPLINE_SURFACE(1,2,((#41158,#41159,#41160,#41161,#41162,#41163,#41164,
#41165,#41166,#41167,#41168,#41169,#41170,#41171,#41172,#41173,#41174,#41175,
#41176,#41177,#41178,#41179,#41180,#41181,#41182,#41183,#41184,#41185,#41186,
#41187,#41188,#41189,#41190,#41191,#41192,#41193,#41194,#41195,#41196,#41197,
#41198,#41199,#41200,#41201,#41202,#41203,#41204,#41205,#41206,#41207,#41208,
#41209,#41210,#41211,#41212,#41213,#41214,#41215,#41216,#41217,#41218,#41219,
#41220,#41221,#41222),(#41223,#41224,#41225,#41226,#41227,#41228,#41229,
#41230,#41231,#41232,#41233,#41234,#41235,#41236,#41237,#41238,#41239,#41240,
#41241,#41242,#41243,#41244,#41245,#41246,#41247,#41248,#41249,#41250,#41251,
#41252,#41253,#41254,#41255,#41256,#41257,#41258,#41259,#41260,#41261,#41262,
#41263,#41264,#41265,#41266,#41267,#41268,#41269,#41270,#41271,#41272,#41273,
#41274,#41275,#41276,#41277,#41278,#41279,#41280,#41281,#41282,#41283,#41284,
#41285,#41286,#41287)),.RULED_SURF.,.F.,.F.,.F.)
B_SPLINE_SURFACE_WITH_KNOTS((2,2),(3,2,2,2,2,2,2,2,2,2,2,2,2,2,2,2,2,2,
2,2,2,2,2,2,2,2,2,2,2,2,2,2,3),(0.,1.),(0.,0.03125,0.0625,0.09375,0.125,
0.15625,0.1875,0.21875,0.25,0.28125,0.3125,0.34375,0.375,0.40625,0.4375,
0.46875,0.5,0.53125,0.5625,0.59375,0.625,0.65625,0.6875,0.71875,0.75,0.78125,
0.8125,0.84375,0.875,0.90625,0.9375,0.96875,1.),.UNSPECIFIED.)
GEOMETRIC_REPRESENTATION_ITEM()
RATIONAL_B_SPLINE_SURFACE(((1.,0.923879532511287,1.,0.923879532511287,1.,
0.923879532511287,1.,0.923879532511287,1.,0.923879532511287,1.,0.923879532511287,
1.,0.923879532511287,1.,0.923879532511287,1.,0.923879532511287,1.,0.923879532511287,
1.,0.923879532511287,1.,0.923879532511287,1.,0.923879532511287,1.,0.923879532511287,
1.,0.923879532511287,1.,0.923879532511287,1.,0.923879532511287,1.,0.923879532511287,
1.,0.923879532511287,1.,0.923879532511287,1.,0.923879532511287,1.,0.923879532511287,
1.,0.923879532511287,1.,0.923879532511287,1.,0.923879532511287,1.,0.923879532511287,
1.,0.923879532511287,1.,0.923879532511287,1.,0.923879532511287,1.,0.923879532511287,
1.,0.923879532511287,1.,0.923879532511287,1.),(1.,0.923879532511287,1.,
0.923879532511287,1.,0.923879532511287,1.,0.923879532511287,1.,0.923879532511287,
1.,0.923879532511287,1.,0.923879532511287,1.,0.923879532511287,1.,0.923879532511287,
1.,0.923879532511287,1.,0.923879532511287,1.,0.923879532511287,1.,0.923879532511287,
1.,0.923879532511287,1.,0.923879532511287,1.,0.923879532511287,1.,0.923879532511287,
1.,0.923879532511287,1.,0.923879532511287,1.,0.923879532511287,1.,0.923879532511287,
1.,0.923879532511287,1.,0.923879532511287,1.,0.923879532511287,1.,0.923879532511287,
1.,0.923879532511287,1.,0.923879532511287,1.,0.923879532511287,1.,0.923879532511287,
1.,0.923879532511287,1.,0.923879532511287,1.,0.923879532511287,1.)))
REPRESENTATION_ITEM('')
SURFACE()
);
#12696=(
BOUNDED_SURFACE()
B_SPLINE_SURFACE(1,2,((#41438,#41439,#41440,#41441,#41442,#41443,#41444,
#41445,#41446,#41447,#41448,#41449,#41450,#41451,#41452,#41453,#41454,#41455,
#41456,#41457,#41458,#41459,#41460,#41461,#41462,#41463,#41464,#41465,#41466,
#41467,#41468,#41469,#41470,#41471,#41472,#41473,#41474,#41475,#41476,#41477,
#41478,#41479,#41480,#41481,#41482,#41483,#41484,#41485,#41486,#41487,#41488,
#41489,#41490,#41491,#41492,#41493,#41494,#41495,#41496,#41497,#41498,#41499,
#41500,#41501,#41502),(#41503,#41504,#41505,#41506,#41507,#41508,#41509,
#41510,#41511,#41512,#41513,#41514,#41515,#41516,#41517,#41518,#41519,#41520,
#41521,#41522,#41523,#41524,#41525,#41526,#41527,#41528,#41529,#41530,#41531,
#41532,#41533,#41534,#41535,#41536,#41537,#41538,#41539,#41540,#41541,#41542,
#41543,#41544,#41545,#41546,#41547,#41548,#41549,#41550,#41551,#41552,#41553,
#41554,#41555,#41556,#41557,#41558,#41559,#41560,#41561,#41562,#41563,#41564,
#41565,#41566,#41567)),.RULED_SURF.,.F.,.F.,.F.)
B_SPLINE_SURFACE_WITH_KNOTS((2,2),(3,2,2,2,2,2,2,2,2,2,2,2,2,2,2,2,2,2,
2,2,2,2,2,2,2,2,2,2,2,2,2,2,3),(0.,1.),(0.,0.03125,0.0625,0.09375,0.125,
0.15625,0.1875,0.21875,0.25,0.28125,0.3125,0.34375,0.375,0.40625,0.4375,
0.46875,0.5,0.53125,0.5625,0.59375,0.625,0.65625,0.6875,0.71875,0.75,0.78125,
0.8125,0.84375,0.875,0.90625,0.9375,0.96875,1.),.UNSPECIFIED.)
GEOMETRIC_REPRESENTATION_ITEM()
RATIONAL_B_SPLINE_SURFACE(((1.,0.923879532511287,1.,0.923879532511287,1.,
0.923879532511287,1.,0.923879532511287,1.,0.923879532511287,1.,0.923879532511287,
1.,0.923879532511287,1.,0.923879532511287,1.,0.923879532511287,1.,0.923879532511287,
1.,0.923879532511287,1.,0.923879532511287,1.,0.923879532511287,1.,0.923879532511287,
1.,0.923879532511287,1.,0.923879532511287,1.,0.923879532511287,1.,0.923879532511287,
1.,0.923879532511287,1.,0.923879532511287,1.,0.923879532511287,1.,0.923879532511287,
1.,0.923879532511287,1.,0.923879532511287,1.,0.923879532511287,1.,0.923879532511287,
1.,0.923879532511287,1.,0.923879532511287,1.,0.923879532511287,1.,0.923879532511287,
1.,0.923879532511287,1.,0.923879532511287,1.),(1.,0.923879532511287,1.,
0.923879532511287,1.,0.923879532511287,1.,0.923879532511287,1.,0.923879532511287,
1.,0.923879532511287,1.,0.923879532511287,1.,0.923879532511287,1.,0.923879532511287,
1.,0.923879532511287,1.,0.923879532511287,1.,0.923879532511287,1.,0.923879532511287,
1.,0.923879532511287,1.,0.923879532511287,1.,0.923879532511287,1.,0.923879532511287,
1.,0.923879532511287,1.,0.923879532511287,1.,0.923879532511287,1.,0.923879532511287,
1.,0.923879532511287,1.,0.923879532511287,1.,0.923879532511287,1.,0.923879532511287,
1.,0.923879532511287,1.,0.923879532511287,1.,0.923879532511287,1.,0.923879532511287,
1.,0.923879532511287,1.,0.923879532511287,1.,0.923879532511287,1.)))
REPRESENTATION_ITEM('')
SURFACE()
);
#12697=(
BOUNDED_SURFACE()
B_SPLINE_SURFACE(2,3,((#41945,#41946,#41947,#41948,#41949,#41950,#41951,
#41952),(#41953,#41954,#41955,#41956,#41957,#41958,#41959,#41960),(#41961,
#41962,#41963,#41964,#41965,#41966,#41967,#41968)),.UNSPECIFIED.,.F.,.F.,
 .F.)
B_SPLINE_SURFACE_WITH_KNOTS((3,3),(4,2,2,4),(0.,1.),(5.64528975859604,6.035253330946,
6.23023511712098,6.42521690329596),.UNSPECIFIED.)
GEOMETRIC_REPRESENTATION_ITEM()
RATIONAL_B_SPLINE_SURFACE(((1.,1.,1.,1.,1.,1.,1.,1.),(0.942691264760503,
0.928068462055693,0.9086240744066,0.860023699971551,0.8404696873878,0.79362173087887,
0.766309763902536,0.736695531754573),(1.,1.,1.,1.,1.,1.,1.,1.)))
REPRESENTATION_ITEM('')
SURFACE()
);
#12698=(
BOUNDED_SURFACE()
B_SPLINE_SURFACE(2,3,((#42113,#42114,#42115,#42116,#42117,#42118,#42119,
#42120),(#42121,#42122,#42123,#42124,#42125,#42126,#42127,#42128),(#42129,
#42130,#42131,#42132,#42133,#42134,#42135,#42136)),.UNSPECIFIED.,.F.,.F.,
 .F.)
B_SPLINE_SURFACE_WITH_KNOTS((3,3),(4,2,2,4),(0.,1.),(5.6742522838321,6.06152855173275,
6.25516668568308,6.4488048196334),.UNSPECIFIED.)
GEOMETRIC_REPRESENTATION_ITEM()
RATIONAL_B_SPLINE_SURFACE(((1.,1.,1.,1.,1.,1.,1.,1.),(0.942182847766815,
0.927521546778884,0.908040805109983,0.859614915545788,0.840162397176485,
0.793600157760153,0.766477590108873,0.736968386371289),(1.,1.,1.,1.,1.,
1.,1.,1.)))
REPRESENTATION_ITEM('')
SURFACE()
);
#12699=(
BOUNDED_SURFACE()
B_SPLINE_SURFACE(2,3,((#42149,#42150,#42151,#42152,#42153,#42154,#42155,
#42156),(#42157,#42158,#42159,#42160,#42161,#42162,#42163,#42164),(#42165,
#42166,#42167,#42168,#42169,#42170,#42171,#42172)),.UNSPECIFIED.,.F.,.F.,
 .F.)
B_SPLINE_SURFACE_WITH_KNOTS((3,3),(4,2,2,4),(0.,1.),(5.6738139462659,6.06124835213276,
6.2549655550662,6.44868275799963),.UNSPECIFIED.)
GEOMETRIC_REPRESENTATION_ITEM()
RATIONAL_B_SPLINE_SURFACE(((1.,1.,1.,1.,1.,1.,1.,1.),(0.942306493740219,
0.927647470996889,0.908169604074547,0.859723335117858,0.840259633125994,
0.793659840617052,0.766511109665431,0.736965071389808),(1.,1.,1.,1.,1.,
1.,1.,1.)))
REPRESENTATION_ITEM('')
SURFACE()
);
#12700=(
BOUNDED_SURFACE()
B_SPLINE_SURFACE(2,3,((#42289,#42290,#42291,#42292,#42293,#42294,#42295,
#42296),(#42297,#42298,#42299,#42300,#42301,#42302,#42303,#42304),(#42305,
#42306,#42307,#42308,#42309,#42310,#42311,#42312)),.UNSPECIFIED.,.F.,.F.,
 .F.)
B_SPLINE_SURFACE_WITH_KNOTS((3,3),(4,2,2,4),(0.,1.),(5.64530724788913,6.03520062826121,
6.23014731844725,6.42509400863329),.UNSPECIFIED.)
GEOMETRIC_REPRESENTATION_ITEM()
RATIONAL_B_SPLINE_SURFACE(((1.,1.,1.,1.,1.,1.,1.,1.),(0.942681470688419,
0.928057129687536,0.90861120034166,0.860012856248506,0.840460372376393,
0.793616444798703,0.766307120509746,0.73669216706025),(1.,1.,1.,1.,1.,1.,
1.,1.)))
REPRESENTATION_ITEM('')
SURFACE()
);
#12701=(
BOUNDED_SURFACE()
B_SPLINE_SURFACE(3,2,((#44818,#44819,#44820),(#44821,#44822,#44823),(#44824,
#44825,#44826),(#44827,#44828,#44829)),.UNSPECIFIED.,.F.,.F.,.F.)
B_SPLINE_SURFACE_WITH_KNOTS((4,4),(3,3),(0.0010803423654197,0.00187374355164022),
(0.,1.),.PIECEWISE_BEZIER_KNOTS.)
GEOMETRIC_REPRESENTATION_ITEM()
RATIONAL_B_SPLINE_SURFACE(((1.,0.942306493778178,1.),(1.,0.979942913916364,
1.),(1.,1.00003953052366,1.),(1.,1.,1.)))
REPRESENTATION_ITEM('')
SURFACE()
);
#12702=(
BOUNDED_SURFACE()
B_SPLINE_SURFACE(3,2,((#44830,#44831,#44832),(#44833,#44834,#44835),(#44836,
#44837,#44838),(#44839,#44840,#44841)),.UNSPECIFIED.,.F.,.F.,.F.)
B_SPLINE_SURFACE_WITH_KNOTS((4,4),(3,3),(0.00108592744242376,0.00187664954092587),
(0.,1.),.PIECEWISE_BEZIER_KNOTS.)
GEOMETRIC_REPRESENTATION_ITEM()
RATIONAL_B_SPLINE_SURFACE(((1.,0.942681470709034,1.),(1.,0.980061484884565,
1.),(1.,1.00004724548358,1.),(1.,1.,1.)))
REPRESENTATION_ITEM('')
SURFACE()
);
#12703=(
BOUNDED_SURFACE()
B_SPLINE_SURFACE(3,2,((#44842,#44843,#44844),(#44845,#44846,#44847),(#44848,
#44849,#44850),(#44851,#44852,#44853)),.UNSPECIFIED.,.F.,.F.,.F.)
B_SPLINE_SURFACE_WITH_KNOTS((4,4),(3,3),(0.00108607226657091,0.00187673136426867),
(0.,1.),.PIECEWISE_BEZIER_KNOTS.)
GEOMETRIC_REPRESENTATION_ITEM()
RATIONAL_B_SPLINE_SURFACE(((1.,0.942691264781529,1.),(1.,0.980064039746506,
1.),(1.,1.00004742170994,1.),(1.,1.,1.)))
REPRESENTATION_ITEM('')
SURFACE()
);
#12704=(
BOUNDED_SURFACE()
B_SPLINE_SURFACE(3,2,((#44854,#44855,#44856),(#44857,#44858,#44859),(#44860,
#44861,#44862),(#44863,#44864,#44865)),.UNSPECIFIED.,.F.,.F.,.F.)
B_SPLINE_SURFACE_WITH_KNOTS((4,4),(3,3),(0.00108339687485018,0.00187989260341564),
(0.,1.),.PIECEWISE_BEZIER_KNOTS.)
GEOMETRIC_REPRESENTATION_ITEM()
RATIONAL_B_SPLINE_SURFACE(((1.,0.942182847767366,1.),(1.,0.979809074317455,
1.),(1.,1.00013954302122,1.),(1.,1.,1.)))
REPRESENTATION_ITEM('')
SURFACE()
);
#12705=(
BOUNDED_SURFACE()
B_SPLINE_SURFACE(3,3,((#44877,#44878,#44879,#44880,#44881,#44882,#44883,
#44884,#44885,#44886,#44887,#44888,#44889,#44890,#44891,#44892,#44893,#44894,
#44895,#44896,#44897,#44898,#44899,#44900,#44901,#44902,#44903,#44904,#44905,
#44906,#44907,#44908,#44909,#44910,#44911,#44912,#44913,#44914,#44915,#44916,
#44917,#44918,#44919,#44920,#44921,#44922,#44923,#44924,#44925,#44926,#44927,
#44928,#44929,#44930,#44931,#44932,#44933,#44934,#44935,#44936,#44937,#44938,
#44939,#44940,#44941,#44942,#44943,#44944,#44945,#44946,#44947,#44948,#44949,
#44950,#44951,#44952,#44953,#44954,#44955,#44956,#44957,#44958),(#44959,
#44960,#44961,#44962,#44963,#44964,#44965,#44966,#44967,#44968,#44969,#44970,
#44971,#44972,#44973,#44974,#44975,#44976,#44977,#44978,#44979,#44980,#44981,
#44982,#44983,#44984,#44985,#44986,#44987,#44988,#44989,#44990,#44991,#44992,
#44993,#44994,#44995,#44996,#44997,#44998,#44999,#45000,#45001,#45002,#45003,
#45004,#45005,#45006,#45007,#45008,#45009,#45010,#45011,#45012,#45013,#45014,
#45015,#45016,#45017,#45018,#45019,#45020,#45021,#45022,#45023,#45024,#45025,
#45026,#45027,#45028,#45029,#45030,#45031,#45032,#45033,#45034,#45035,#45036,
#45037,#45038,#45039,#45040),(#45041,#45042,#45043,#45044,#45045,#45046,
#45047,#45048,#45049,#45050,#45051,#45052,#45053,#45054,#45055,#45056,#45057,
#45058,#45059,#45060,#45061,#45062,#45063,#45064,#45065,#45066,#45067,#45068,
#45069,#45070,#45071,#45072,#45073,#45074,#45075,#45076,#45077,#45078,#45079,
#45080,#45081,#45082,#45083,#45084,#45085,#45086,#45087,#45088,#45089,#45090,
#45091,#45092,#45093,#45094,#45095,#45096,#45097,#45098,#45099,#45100,#45101,
#45102,#45103,#45104,#45105,#45106,#45107,#45108,#45109,#45110,#45111,#45112,
#45113,#45114,#45115,#45116,#45117,#45118,#45119,#45120,#45121,#45122),
(#45123,#45124,#45125,#45126,#45127,#45128,#45129,#45130,#45131,#45132,
#45133,#45134,#45135,#45136,#45137,#45138,#45139,#45140,#45141,#45142,#45143,
#45144,#45145,#45146,#45147,#45148,#45149,#45150,#45151,#45152,#45153,#45154,
#45155,#45156,#45157,#45158,#45159,#45160,#45161,#45162,#45163,#45164,#45165,
#45166,#45167,#45168,#45169,#45170,#45171,#45172,#45173,#45174,#45175,#45176,
#45177,#45178,#45179,#45180,#45181,#45182,#45183,#45184,#45185,#45186,#45187,
#45188,#45189,#45190,#45191,#45192,#45193,#45194,#45195,#45196,#45197,#45198,
#45199,#45200,#45201,#45202,#45203,#45204),(#45205,#45206,#45207,#45208,
#45209,#45210,#45211,#45212,#45213,#45214,#45215,#45216,#45217,#45218,#45219,
#45220,#45221,#45222,#45223,#45224,#45225,#45226,#45227,#45228,#45229,#45230,
#45231,#45232,#45233,#45234,#45235,#45236,#45237,#45238,#45239,#45240,#45241,
#45242,#45243,#45244,#45245,#45246,#45247,#45248,#45249,#45250,#45251,#45252,
#45253,#45254,#45255,#45256,#45257,#45258,#45259,#45260,#45261,#45262,#45263,
#45264,#45265,#45266,#45267,#45268,#45269,#45270,#45271,#45272,#45273,#45274,
#45275,#45276,#45277,#45278,#45279,#45280,#45281,#45282,#45283,#45284,#45285,
#45286),(#45287,#45288,#45289,#45290,#45291,#45292,#45293,#45294,#45295,
#45296,#45297,#45298,#45299,#45300,#45301,#45302,#45303,#45304,#45305,#45306,
#45307,#45308,#45309,#45310,#45311,#45312,#45313,#45314,#45315,#45316,#45317,
#45318,#45319,#45320,#45321,#45322,#45323,#45324,#45325,#45326,#45327,#45328,
#45329,#45330,#45331,#45332,#45333,#45334,#45335,#45336,#45337,#45338,#45339,
#45340,#45341,#45342,#45343,#45344,#45345,#45346,#45347,#45348,#45349,#45350,
#45351,#45352,#45353,#45354,#45355,#45356,#45357,#45358,#45359,#45360,#45361,
#45362,#45363,#45364,#45365,#45366,#45367,#45368),(#45369,#45370,#45371,
#45372,#45373,#45374,#45375,#45376,#45377,#45378,#45379,#45380,#45381,#45382,
#45383,#45384,#45385,#45386,#45387,#45388,#45389,#45390,#45391,#45392,#45393,
#45394,#45395,#45396,#45397,#45398,#45399,#45400,#45401,#45402,#45403,#45404,
#45405,#45406,#45407,#45408,#45409,#45410,#45411,#45412,#45413,#45414,#45415,
#45416,#45417,#45418,#45419,#45420,#45421,#45422,#45423,#45424,#45425,#45426,
#45427,#45428,#45429,#45430,#45431,#45432,#45433,#45434,#45435,#45436,#45437,
#45438,#45439,#45440,#45441,#45442,#45443,#45444,#45445,#45446,#45447,#45448,
#45449,#45450)),.UNSPECIFIED.,.F.,.F.,.F.)
B_SPLINE_SURFACE_WITH_KNOTS((4,3,4),(4,2,2,2,2,2,2,2,2,2,2,2,2,2,2,2,2,
2,2,2,2,2,2,2,2,2,2,2,2,2,2,2,2,2,2,2,2,2,2,2,4),(0.786869258805392,1.,
1.21306714374991),(0.,0.00290159839858374,0.0290642712719717,0.0552269441453597,
0.0813896170215754,0.107552289897791,0.133714962774007,0.159877635650223,
0.186040308526438,0.212202981402654,0.23836565427887,0.264528327155085,
0.290691000031301,0.316853672907516,0.343016345783732,0.369179018659948,
0.395341691536163,0.42150436441238,0.447667037288595,0.473829710164811,
0.499992383041026,0.526155055917242,0.552317728793458,0.578480401669673,
0.604643074545889,0.630805747422105,0.656968420298321,0.683131093174536,
0.709293766050752,0.735456438926968,0.761619111803183,0.787781784679399,
0.813944457555615,0.840107130431831,0.866269803308046,0.892432476184262,
0.918595149060478,0.944757821936694,0.970920494812909,0.997083167689125,
1.),.UNSPECIFIED.)
GEOMETRIC_REPRESENTATION_ITEM()
RATIONAL_B_SPLINE_SURFACE(((0.510874737958872,0.510874737958872,0.510874737958872,
0.510874737958872,0.510874737958872,0.510874737958872,0.510874737958872,
0.510874737958872,0.510874737958872,0.510874737958872,0.510874737958872,
0.510874737958872,0.510874737958872,0.510874737958872,0.510874737958872,
0.510874737958872,0.510874737958872,0.510874737958872,0.510874737958872,
0.510874737958872,0.510874737958872,0.510874737958872,0.510874737958872,
0.510874737958872,0.510874737958872,0.510874737958872,0.510874737958872,
0.510874737958872,0.510874737958872,0.510874737958872,0.510874737958872,
0.510874737958872,0.510874737958872,0.510874737958872,0.510874737958872,
0.510874737958872,0.510874737958872,0.510874737958872,0.510874737958872,
0.510874737958872,0.510874737958872,0.510874737958872,0.510874737958872,
0.510874737958872,0.510874737958872,0.510874737958872,0.510874737958872,
0.510874737958872,0.510874737958872,0.510874737958872,0.510874737958872,
0.510874737958872,0.510874737958872,0.510874737958872,0.510874737958872,
0.510874737958872,0.510874737958872,0.510874737958872,0.510874737958872,
0.510874737958872,0.510874737958872,0.510874737958872,0.510874737958872,
0.510874737958872,0.510874737958872,0.510874737958872,0.510874737958872,
0.510874737958872,0.510874737958872,0.510874737958872,0.510874737958872,
0.510874737958872,0.510874737958872,0.510874737958872,0.510874737958872,
0.510874737958872,0.510874737958872,0.510874737958872,0.510874737958872,
0.510874737958872,0.510874737958872,0.510874737958872),(0.552783924393481,
0.552783924393481,0.552783924393481,0.552783924393481,0.552783924393481,
0.552783924393481,0.552783924393481,0.552783924393481,0.552783924393481,
0.552783924393481,0.552783924393481,0.552783924393481,0.552783924393481,
0.552783924393481,0.552783924393481,0.552783924393481,0.552783924393481,
0.552783924393481,0.552783924393481,0.552783924393481,0.552783924393481,
0.552783924393481,0.552783924393481,0.552783924393481,0.552783924393481,
0.552783924393481,0.552783924393481,0.552783924393481,0.552783924393481,
0.552783924393481,0.552783924393481,0.552783924393481,0.552783924393481,
0.552783924393481,0.552783924393481,0.552783924393481,0.552783924393481,
0.552783924393481,0.552783924393481,0.552783924393481,0.552783924393481,
0.552783924393481,0.552783924393481,0.552783924393481,0.552783924393481,
0.552783924393481,0.552783924393481,0.552783924393481,0.552783924393481,
0.552783924393481,0.552783924393481,0.552783924393481,0.552783924393481,
0.552783924393481,0.552783924393481,0.552783924393481,0.552783924393481,
0.552783924393481,0.552783924393481,0.552783924393481,0.552783924393481,
0.552783924393481,0.552783924393481,0.552783924393481,0.552783924393481,
0.552783924393481,0.552783924393481,0.552783924393481,0.552783924393481,
0.552783924393481,0.552783924393481,0.552783924393481,0.552783924393481,
0.552783924393481,0.552783924393481,0.552783924393481,0.552783924393481,
0.552783924393481,0.552783924393481,0.552783924393481,0.552783924393481,
0.552783924393481),(0.71582567840719,0.71582567840719,0.71582567840719,
0.71582567840719,0.71582567840719,0.71582567840719,0.71582567840719,0.71582567840719,
0.71582567840719,0.71582567840719,0.71582567840719,0.71582567840719,0.71582567840719,
0.71582567840719,0.71582567840719,0.71582567840719,0.71582567840719,0.71582567840719,
0.71582567840719,0.71582567840719,0.71582567840719,0.71582567840719,0.71582567840719,
0.71582567840719,0.71582567840719,0.71582567840719,0.71582567840719,0.71582567840719,
0.71582567840719,0.71582567840719,0.71582567840719,0.71582567840719,0.71582567840719,
0.71582567840719,0.71582567840719,0.71582567840719,0.71582567840719,0.71582567840719,
0.71582567840719,0.71582567840719,0.71582567840719,0.71582567840719,0.71582567840719,
0.71582567840719,0.71582567840719,0.71582567840719,0.71582567840719,0.71582567840719,
0.71582567840719,0.71582567840719,0.71582567840719,0.71582567840719,0.71582567840719,
0.71582567840719,0.71582567840719,0.71582567840719,0.71582567840719,0.71582567840719,
0.71582567840719,0.71582567840719,0.71582567840719,0.71582567840719,0.71582567840719,
0.71582567840719,0.71582567840719,0.71582567840719,0.71582567840719,0.71582567840719,
0.71582567840719,0.71582567840719,0.71582567840719,0.71582567840719,0.71582567840719,
0.71582567840719,0.71582567840719,0.71582567840719,0.71582567840719,0.71582567840719,
0.71582567840719,0.71582567840719,0.71582567840719,0.71582567840719),(1.,
1.,1.,1.,1.,1.,1.,1.,1.,1.,1.,1.,1.,1.,1.,1.,1.,1.,1.,1.,1.,1.,1.,1.,1.,
1.,1.,1.,1.,1.,1.,1.,1.,1.,1.,1.,1.,1.,1.,1.,1.,1.,1.,1.,1.,1.,1.,1.,1.,
1.,1.,1.,1.,1.,1.,1.,1.,1.,1.,1.,1.,1.,1.,1.,1.,1.,1.,1.,1.,1.,1.,1.,1.,
1.,1.,1.,1.,1.,1.,1.,1.,1.),(0.715910475000114,0.715910475000114,0.715910475000114,
0.715910475000114,0.715910475000114,0.715910475000114,0.715910475000114,
0.715910475000114,0.715910475000114,0.715910475000114,0.715910475000114,
0.715910475000114,0.715910475000114,0.715910475000114,0.715910475000114,
0.715910475000114,0.715910475000114,0.715910475000114,0.715910475000114,
0.715910475000114,0.715910475000114,0.715910475000114,0.715910475000114,
0.715910475000114,0.715910475000114,0.715910475000114,0.715910475000114,
0.715910475000114,0.715910475000114,0.715910475000114,0.715910475000114,
0.715910475000114,0.715910475000114,0.715910475000114,0.715910475000114,
0.715910475000114,0.715910475000114,0.715910475000114,0.715910475000114,
0.715910475000114,0.715910475000114,0.715910475000114,0.715910475000114,
0.715910475000114,0.715910475000114,0.715910475000114,0.715910475000114,
0.715910475000114,0.715910475000114,0.715910475000114,0.715910475000114,
0.715910475000114,0.715910475000114,0.715910475000114,0.715910475000114,
0.715910475000114,0.715910475000114,0.715910475000114,0.715910475000114,
0.715910475000114,0.715910475000114,0.715910475000114,0.715910475000114,
0.715910475000114,0.715910475000114,0.715910475000114,0.715910475000114,
0.715910475000114,0.715910475000114,0.715910475000114,0.715910475000114,
0.715910475000114,0.715910475000114,0.715910475000114,0.715910475000114,
0.715910475000114,0.715910475000114,0.715910475000114,0.715910475000114,
0.715910475000114,0.715910475000114,0.715910475000114),(0.552881237322219,
0.552881237322219,0.552881237322219,0.552881237322219,0.552881237322219,
0.552881237322219,0.552881237322219,0.552881237322219,0.552881237322219,
0.552881237322219,0.552881237322219,0.552881237322219,0.552881237322219,
0.552881237322219,0.552881237322219,0.552881237322219,0.552881237322219,
0.552881237322219,0.552881237322219,0.552881237322219,0.552881237322219,
0.552881237322219,0.552881237322219,0.552881237322219,0.552881237322219,
0.552881237322219,0.552881237322219,0.552881237322219,0.552881237322219,
0.552881237322219,0.552881237322219,0.552881237322219,0.552881237322219,
0.552881237322219,0.552881237322219,0.552881237322219,0.552881237322219,
0.552881237322219,0.552881237322219,0.552881237322219,0.552881237322219,
0.552881237322219,0.552881237322219,0.552881237322219,0.552881237322219,
0.552881237322219,0.552881237322219,0.552881237322219,0.552881237322219,
0.552881237322219,0.552881237322219,0.552881237322219,0.552881237322219,
0.552881237322219,0.552881237322219,0.552881237322219,0.552881237322219,
0.552881237322219,0.552881237322219,0.552881237322219,0.552881237322219,
0.552881237322219,0.552881237322219,0.552881237322219,0.552881237322219,
0.552881237322219,0.552881237322219,0.552881237322219,0.552881237322219,
0.552881237322219,0.552881237322219,0.552881237322219,0.552881237322219,
0.552881237322219,0.552881237322219,0.552881237322219,0.552881237322219,
0.552881237322219,0.552881237322219,0.552881237322219,0.552881237322219,
0.552881237322219),(0.510912286966316,0.510912286966316,0.510912286966316,
0.510912286966316,0.510912286966316,0.510912286966316,0.510912286966316,
0.510912286966316,0.510912286966316,0.510912286966316,0.510912286966316,
0.510912286966316,0.510912286966316,0.510912286966316,0.510912286966316,
0.510912286966316,0.510912286966316,0.510912286966316,0.510912286966316,
0.510912286966316,0.510912286966316,0.510912286966316,0.510912286966316,
0.510912286966316,0.510912286966316,0.510912286966316,0.510912286966316,
0.510912286966316,0.510912286966316,0.510912286966316,0.510912286966316,
0.510912286966316,0.510912286966316,0.510912286966316,0.510912286966316,
0.510912286966316,0.510912286966316,0.510912286966316,0.510912286966316,
0.510912286966316,0.510912286966316,0.510912286966316,0.510912286966316,
0.510912286966316,0.510912286966316,0.510912286966316,0.510912286966316,
0.510912286966316,0.510912286966316,0.510912286966316,0.510912286966316,
0.510912286966316,0.510912286966316,0.510912286966316,0.510912286966316,
0.510912286966316,0.510912286966316,0.510912286966316,0.510912286966316,
0.510912286966316,0.510912286966316,0.510912286966316,0.510912286966316,
0.510912286966316,0.510912286966316,0.510912286966316,0.510912286966316,
0.510912286966316,0.510912286966316,0.510912286966316,0.510912286966316,
0.510912286966316,0.510912286966316,0.510912286966316,0.510912286966316,
0.510912286966316,0.510912286966316,0.510912286966316,0.510912286966316,
0.510912286966316,0.510912286966316,0.510912286966316)))
REPRESENTATION_ITEM('')
SURFACE()
);
#12706=ADVANCED_FACE('',(#11544),#12663,.T.);
#12707=ADVANCED_FACE('',(#11545),#1538,.F.);
#12708=ADVANCED_FACE('',(#11546),#1201,.T.);
#12709=ADVANCED_FACE('',(#11547),#12664,.T.);
#12710=ADVANCED_FACE('',(#11548),#1202,.T.);
#12711=ADVANCED_FACE('',(#11549,#11550),#1203,.F.);
#12712=ADVANCED_FACE('',(#11551),#12665,.F.);
#12713=ADVANCED_FACE('',(#11552,#11553),#1204,.F.);
#12714=ADVANCED_FACE('',(#11554,#11555),#1205,.T.);
#12715=ADVANCED_FACE('',(#11556),#1206,.F.);
#12716=ADVANCED_FACE('',(#11557),#1207,.F.);
#12717=ADVANCED_FACE('',(#11558),#1539,.F.);
#12718=ADVANCED_FACE('',(#11559),#1208,.F.);
#12719=ADVANCED_FACE('',(#11560),#1209,.F.);
#12720=ADVANCED_FACE('',(#11561),#1540,.F.);
#12721=ADVANCED_FACE('',(#11562),#1210,.F.);
#12722=ADVANCED_FACE('',(#11563),#1211,.F.);
#12723=ADVANCED_FACE('',(#11564),#1541,.F.);
#12724=ADVANCED_FACE('',(#11565,#11566),#1212,.F.);
#12725=ADVANCED_FACE('',(#11567,#11568),#1213,.F.);
#12726=ADVANCED_FACE('',(#11569,#11570),#1214,.F.);
#12727=ADVANCED_FACE('',(#11571,#11572),#1215,.F.);
#12728=ADVANCED_FACE('',(#11573,#11574,#11575,#11576,#11577,#11578,#11579,
#11580,#11581,#11582,#11583,#11584,#11585),#1216,.F.);
#12729=ADVANCED_FACE('',(#11586,#11587,#11588,#11589,#11590,#11591,#11592,
#11593,#11594,#11595,#11596,#11597,#11598),#1217,.T.);
#12730=ADVANCED_FACE('',(#11599,#11600),#1218,.T.);
#12731=ADVANCED_FACE('',(#11601,#11602),#1219,.F.);
#12732=ADVANCED_FACE('',(#11603,#11604),#1542,.F.);
#12733=ADVANCED_FACE('',(#11605,#11606),#1543,.F.);
#12734=ADVANCED_FACE('',(#11607,#11608),#1544,.T.);
#12735=ADVANCED_FACE('',(#11609,#11610),#1545,.T.);
#12736=ADVANCED_FACE('',(#11611,#11612),#1546,.T.);
#12737=ADVANCED_FACE('',(#11613,#11614),#1547,.F.);
#12738=ADVANCED_FACE('',(#11615,#11616),#1548,.F.);
#12739=ADVANCED_FACE('',(#11617,#11618),#1549,.F.);
#12740=ADVANCED_FACE('',(#11619,#11620),#1550,.F.);
#12741=ADVANCED_FACE('',(#11621,#11622),#1551,.F.);
#12742=ADVANCED_FACE('',(#11623,#11624),#1552,.F.);
#12743=ADVANCED_FACE('',(#11625,#11626),#1553,.F.);
#12744=ADVANCED_FACE('',(#11627,#11628),#1554,.F.);
#12745=ADVANCED_FACE('',(#11629,#11630),#1555,.F.);
#12746=ADVANCED_FACE('',(#11631,#11632),#1556,.F.);
#12747=ADVANCED_FACE('',(#11633,#11634),#1557,.F.);
#12748=ADVANCED_FACE('',(#11635),#1558,.F.);
#12749=ADVANCED_FACE('',(#11636),#1559,.F.);
#12750=ADVANCED_FACE('',(#11637),#1560,.F.);
#12751=ADVANCED_FACE('',(#11638,#11639),#1561,.F.);
#12752=ADVANCED_FACE('',(#11640,#11641),#1562,.F.);
#12753=ADVANCED_FACE('',(#11642,#11643),#1563,.F.);
#12754=ADVANCED_FACE('',(#11644,#11645),#255,.T.);
#12755=ADVANCED_FACE('',(#11646),#12666,.F.);
#12756=ADVANCED_FACE('',(#11647,#11648),#1220,.F.);
#12757=ADVANCED_FACE('',(#11649,#11650),#1221,.F.);
#12758=ADVANCED_FACE('',(#11651),#12667,.F.);
#12759=ADVANCED_FACE('',(#11652),#40,.F.);
#12760=ADVANCED_FACE('',(#11653),#1564,.T.);
#12761=ADVANCED_FACE('',(#11654),#1222,.F.);
#12762=ADVANCED_FACE('',(#11655),#1223,.T.);
#12763=ADVANCED_FACE('',(#11656,#11657),#1224,.F.);
#12764=ADVANCED_FACE('',(#11658,#11659),#1225,.F.);
#12765=ADVANCED_FACE('',(#11660,#11661),#1226,.F.);
#12766=ADVANCED_FACE('',(#11662,#11663),#1227,.F.);
#12767=ADVANCED_FACE('',(#11664,#11665),#1228,.F.);
#12768=ADVANCED_FACE('',(#11666,#11667),#1229,.F.);
#12769=ADVANCED_FACE('',(#11668,#11669),#1230,.F.);
#12770=ADVANCED_FACE('',(#11670,#11671),#1231,.F.);
#12771=ADVANCED_FACE('',(#11672,#11673),#1232,.F.);
#12772=ADVANCED_FACE('',(#11674,#11675),#1565,.T.);
#12773=ADVANCED_FACE('',(#11676,#11677),#1566,.T.);
#12774=ADVANCED_FACE('',(#11678,#11679),#1567,.F.);
#12775=ADVANCED_FACE('',(#11680,#11681),#256,.T.);
#12776=ADVANCED_FACE('',(#11682,#11683),#1568,.F.);
#12777=ADVANCED_FACE('',(#11684,#11685),#1569,.F.);
#12778=ADVANCED_FACE('',(#11686,#11687),#21,.F.);
#12779=ADVANCED_FACE('',(#11688,#11689),#1570,.T.);
#12780=ADVANCED_FACE('',(#11690,#11691),#1571,.T.);
#12781=ADVANCED_FACE('',(#11692,#11693),#257,.F.);
#12782=ADVANCED_FACE('',(#11694,#11695),#1572,.T.);
#12783=ADVANCED_FACE('',(#11696,#11697),#1573,.T.);
#12784=ADVANCED_FACE('',(#11698,#11699),#1574,.T.);
#12785=ADVANCED_FACE('',(#11700,#11701),#258,.F.);
#12786=ADVANCED_FACE('',(#11702,#11703),#259,.F.);
#12787=ADVANCED_FACE('',(#11704,#11705),#260,.F.);
#12788=ADVANCED_FACE('',(#11706,#11707),#261,.T.);
#12789=ADVANCED_FACE('',(#11708,#11709),#262,.F.);
#12790=ADVANCED_FACE('',(#11710,#11711),#263,.F.);
#12791=ADVANCED_FACE('',(#11712,#11713),#264,.T.);
#12792=ADVANCED_FACE('',(#11714,#11715),#265,.T.);
#12793=ADVANCED_FACE('',(#11716,#11717),#266,.T.);
#12794=ADVANCED_FACE('',(#11718,#11719),#267,.T.);
#12795=ADVANCED_FACE('',(#11720,#11721),#268,.T.);
#12796=ADVANCED_FACE('',(#11722,#11723),#1575,.T.);
#12797=ADVANCED_FACE('',(#11724,#11725),#269,.F.);
#12798=ADVANCED_FACE('',(#11726,#11727),#270,.F.);
#12799=ADVANCED_FACE('',(#11728),#1233,.F.);
#12800=ADVANCED_FACE('',(#11729),#1234,.T.);
#12801=ADVANCED_FACE('',(#11730),#1235,.T.);
#12802=ADVANCED_FACE('',(#11731),#41,.T.);
#12803=ADVANCED_FACE('',(#11732),#42,.T.);
#12804=ADVANCED_FACE('',(#11733),#1236,.F.);
#12805=ADVANCED_FACE('',(#11734),#43,.T.);
#12806=ADVANCED_FACE('',(#11735),#44,.T.);
#12807=ADVANCED_FACE('',(#11736),#45,.T.);
#12808=ADVANCED_FACE('',(#11737),#46,.T.);
#12809=ADVANCED_FACE('',(#11738),#47,.T.);
#12810=ADVANCED_FACE('',(#11739),#48,.T.);
#12811=ADVANCED_FACE('',(#11740),#49,.T.);
#12812=ADVANCED_FACE('',(#11741),#50,.T.);
#12813=ADVANCED_FACE('',(#11742),#51,.T.);
#12814=ADVANCED_FACE('',(#11743),#52,.T.);
#12815=ADVANCED_FACE('',(#11744),#12668,.T.);
#12816=ADVANCED_FACE('',(#11745),#12669,.T.);
#12817=ADVANCED_FACE('',(#11746),#12670,.T.);
#12818=ADVANCED_FACE('',(#11747),#1576,.T.);
#12819=ADVANCED_FACE('',(#11748),#12671,.T.);
#12820=ADVANCED_FACE('',(#11749),#12672,.T.);
#12821=ADVANCED_FACE('',(#11750),#12673,.T.);
#12822=ADVANCED_FACE('',(#11751),#1237,.T.);
#12823=ADVANCED_FACE('',(#11752),#1238,.T.);
#12824=ADVANCED_FACE('',(#11753),#1239,.F.);
#12825=ADVANCED_FACE('',(#11754,#11755),#1577,.T.);
#12826=ADVANCED_FACE('',(#11756),#1240,.F.);
#12827=ADVANCED_FACE('',(#11757),#1241,.T.);
#12828=ADVANCED_FACE('',(#11758,#11759),#12674,.T.);
#12829=ADVANCED_FACE('',(#11760),#1578,.T.);
#12830=ADVANCED_FACE('',(#11761),#271,.T.);
#12831=ADVANCED_FACE('',(#11762),#272,.T.);
#12832=ADVANCED_FACE('',(#11763),#273,.T.);
#12833=ADVANCED_FACE('',(#11764),#1579,.F.);
#12834=ADVANCED_FACE('',(#11765),#1580,.T.);
#12835=ADVANCED_FACE('',(#11766),#1581,.F.);
#12836=ADVANCED_FACE('',(#11767),#274,.T.);
#12837=ADVANCED_FACE('',(#11768),#275,.T.);
#12838=ADVANCED_FACE('',(#11769),#276,.T.);
#12839=ADVANCED_FACE('',(#11770),#277,.T.);
#12840=ADVANCED_FACE('',(#11771),#1582,.T.);
#12841=ADVANCED_FACE('',(#11772),#1583,.F.);
#12842=ADVANCED_FACE('',(#11773),#1584,.T.);
#12843=ADVANCED_FACE('',(#11774),#278,.T.);
#12844=ADVANCED_FACE('',(#11775),#1585,.F.);
#12845=ADVANCED_FACE('',(#11776),#1586,.T.);
#12846=ADVANCED_FACE('',(#11777),#279,.T.);
#12847=ADVANCED_FACE('',(#11778),#280,.T.);
#12848=ADVANCED_FACE('',(#11779),#281,.T.);
#12849=ADVANCED_FACE('',(#11780),#282,.T.);
#12850=ADVANCED_FACE('',(#11781),#283,.T.);
#12851=ADVANCED_FACE('',(#11782),#1587,.T.);
#12852=ADVANCED_FACE('',(#11783),#1588,.F.);
#12853=ADVANCED_FACE('',(#11784),#284,.T.);
#12854=ADVANCED_FACE('',(#11785),#1589,.T.);
#12855=ADVANCED_FACE('',(#11786),#1590,.F.);
#12856=ADVANCED_FACE('',(#11787),#285,.T.);
#12857=ADVANCED_FACE('',(#11788),#286,.T.);
#12858=ADVANCED_FACE('',(#11789),#287,.T.);
#12859=ADVANCED_FACE('',(#11790),#288,.T.);
#12860=ADVANCED_FACE('',(#11791),#289,.T.);
#12861=ADVANCED_FACE('',(#11792),#290,.T.);
#12862=ADVANCED_FACE('',(#11793),#1591,.F.);
#12863=ADVANCED_FACE('',(#11794),#1592,.T.);
#12864=ADVANCED_FACE('',(#11795),#291,.T.);
#12865=ADVANCED_FACE('',(#11796),#1593,.F.);
#12866=ADVANCED_FACE('',(#11797),#1594,.T.);
#12867=ADVANCED_FACE('',(#11798),#292,.T.);
#12868=ADVANCED_FACE('',(#11799),#293,.T.);
#12869=ADVANCED_FACE('',(#11800),#294,.T.);
#12870=ADVANCED_FACE('',(#11801),#295,.T.);
#12871=ADVANCED_FACE('',(#11802),#1595,.T.);
#12872=ADVANCED_FACE('',(#11803),#1596,.F.);
#12873=ADVANCED_FACE('',(#11804),#296,.T.);
#12874=ADVANCED_FACE('',(#11805),#1597,.T.);
#12875=ADVANCED_FACE('',(#11806),#1598,.F.);
#12876=ADVANCED_FACE('',(#11807),#297,.T.);
#12877=ADVANCED_FACE('',(#11808),#298,.T.);
#12878=ADVANCED_FACE('',(#11809),#299,.T.);
#12879=ADVANCED_FACE('',(#11810),#300,.T.);
#12880=ADVANCED_FACE('',(#11811),#301,.T.);
#12881=ADVANCED_FACE('',(#11812),#1599,.F.);
#12882=ADVANCED_FACE('',(#11813),#1600,.T.);
#12883=ADVANCED_FACE('',(#11814),#302,.T.);
#12884=ADVANCED_FACE('',(#11815,#11816),#1242,.F.);
#12885=ADVANCED_FACE('',(#11817,#11818),#1243,.F.);
#12886=ADVANCED_FACE('',(#11819,#11820),#1244,.F.);
#12887=ADVANCED_FACE('',(#11821),#12675,.T.);
#12888=ADVANCED_FACE('',(#11822),#53,.T.);
#12889=ADVANCED_FACE('',(#11823),#1601,.F.);
#12890=ADVANCED_FACE('',(#11824),#1245,.T.);
#12891=ADVANCED_FACE('',(#11825),#1246,.F.);
#12892=ADVANCED_FACE('',(#11826,#11827),#1247,.F.);
#12893=ADVANCED_FACE('',(#11828,#11829,#11830,#11831,#11832),#1248,.T.);
#12894=ADVANCED_FACE('',(#11833),#1602,.T.);
#12895=ADVANCED_FACE('',(#11834),#1249,.F.);
#12896=ADVANCED_FACE('',(#11835),#1603,.T.);
#12897=ADVANCED_FACE('',(#11836),#1250,.T.);
#12898=ADVANCED_FACE('',(#11837),#1604,.T.);
#12899=ADVANCED_FACE('',(#11838),#1251,.F.);
#12900=ADVANCED_FACE('',(#11839),#1252,.T.);
#12901=ADVANCED_FACE('',(#11840),#1605,.T.);
#12902=ADVANCED_FACE('',(#11841),#1253,.F.);
#12903=ADVANCED_FACE('',(#11842),#1606,.T.);
#12904=ADVANCED_FACE('',(#11843),#1254,.T.);
#12905=ADVANCED_FACE('',(#11844,#11845,#11846,#11847,#11848),#1255,.F.);
#12906=ADVANCED_FACE('',(#11849,#11850),#1607,.F.);
#12907=ADVANCED_FACE('',(#11851),#1608,.T.);
#12908=ADVANCED_FACE('',(#11852,#11853),#1609,.F.);
#12909=ADVANCED_FACE('',(#11854,#11855),#1610,.F.);
#12910=ADVANCED_FACE('',(#11856,#11857),#1611,.F.);
#12911=ADVANCED_FACE('',(#11858,#11859),#1612,.F.);
#12912=ADVANCED_FACE('',(#11860,#11861),#1613,.F.);
#12913=ADVANCED_FACE('',(#11862,#11863),#1614,.F.);
#12914=ADVANCED_FACE('',(#11864),#303,.T.);
#12915=ADVANCED_FACE('',(#11865),#304,.T.);
#12916=ADVANCED_FACE('',(#11866,#11867),#305,.F.);
#12917=ADVANCED_FACE('',(#11868,#11869),#306,.T.);
#12918=ADVANCED_FACE('',(#11870),#1256,.F.);
#12919=ADVANCED_FACE('',(#11871),#1257,.T.);
#12920=ADVANCED_FACE('',(#11872),#1258,.T.);
#12921=ADVANCED_FACE('',(#11873),#1259,.F.);
#12922=ADVANCED_FACE('',(#11874),#1260,.T.);
#12923=ADVANCED_FACE('',(#11875),#1261,.T.);
#12924=ADVANCED_FACE('',(#11876),#1262,.F.);
#12925=ADVANCED_FACE('',(#11877),#1263,.F.);
#12926=ADVANCED_FACE('',(#11878),#1264,.T.);
#12927=ADVANCED_FACE('',(#11879,#11880),#1265,.F.);
#12928=ADVANCED_FACE('',(#11881),#1266,.T.);
#12929=ADVANCED_FACE('',(#11882),#1267,.T.);
#12930=ADVANCED_FACE('',(#11883),#1268,.T.);
#12931=ADVANCED_FACE('',(#11884),#1269,.T.);
#12932=ADVANCED_FACE('',(#11885),#1270,.T.);
#12933=ADVANCED_FACE('',(#11886,#11887),#14,.T.);
#12934=ADVANCED_FACE('',(#11888,#11889),#1615,.T.);
#12935=ADVANCED_FACE('',(#11890,#11891),#22,.T.);
#12936=ADVANCED_FACE('',(#11892,#11893),#1271,.F.);
#12937=ADVANCED_FACE('',(#11894,#11895),#1272,.T.);
#12938=ADVANCED_FACE('',(#11896,#11897),#1616,.T.);
#12939=ADVANCED_FACE('',(#11898,#11899),#1617,.F.);
#12940=ADVANCED_FACE('',(#11900,#11901),#23,.F.);
#12941=ADVANCED_FACE('',(#11902,#11903),#24,.F.);
#12942=ADVANCED_FACE('',(#11904,#11905),#1618,.F.);
#12943=ADVANCED_FACE('',(#11906,#11907),#1273,.T.);
#12944=ADVANCED_FACE('',(#11908,#11909),#1274,.T.);
#12945=ADVANCED_FACE('',(#11910,#11911),#1275,.T.);
#12946=ADVANCED_FACE('',(#11912,#11913),#1276,.T.);
#12947=ADVANCED_FACE('',(#11914,#11915),#1277,.T.);
#12948=ADVANCED_FACE('',(#11916,#11917),#25,.T.);
#12949=ADVANCED_FACE('',(#11918,#11919),#1619,.T.);
#12950=ADVANCED_FACE('',(#11920,#11921),#1620,.F.);
#12951=ADVANCED_FACE('',(#11922,#11923),#1621,.T.);
#12952=ADVANCED_FACE('',(#11924,#11925),#1622,.F.);
#12953=ADVANCED_FACE('',(#11926,#11927),#1623,.F.);
#12954=ADVANCED_FACE('',(#11928),#12676,.T.);
#12955=ADVANCED_FACE('',(#11929),#12677,.T.);
#12956=ADVANCED_FACE('',(#11930),#12678,.T.);
#12957=ADVANCED_FACE('',(#11931),#1624,.F.);
#12958=ADVANCED_FACE('',(#11932),#1278,.F.);
#12959=ADVANCED_FACE('',(#11933),#1625,.T.);
#12960=ADVANCED_FACE('',(#11934),#12679,.T.);
#12961=ADVANCED_FACE('',(#11935),#12680,.T.);
#12962=ADVANCED_FACE('',(#11936),#12681,.T.);
#12963=ADVANCED_FACE('',(#11937),#1279,.F.);
#12964=ADVANCED_FACE('',(#11938),#1280,.F.);
#12965=ADVANCED_FACE('',(#11939),#12682,.T.);
#12966=ADVANCED_FACE('',(#11940),#54,.T.);
#12967=ADVANCED_FACE('',(#11941),#12683,.T.);
#12968=ADVANCED_FACE('',(#11942),#1626,.T.);
#12969=ADVANCED_FACE('',(#11943,#11944),#1281,.F.);
#12970=ADVANCED_FACE('',(#11945,#11946),#1282,.T.);
#12971=ADVANCED_FACE('',(#11947,#11948),#1283,.T.);
#12972=ADVANCED_FACE('',(#11949),#1284,.F.);
#12973=ADVANCED_FACE('',(#11950,#11951,#11952),#1285,.T.);
#12974=ADVANCED_FACE('',(#11953,#11954),#1627,.F.);
#12975=ADVANCED_FACE('',(#11955,#11956),#1628,.T.);
#12976=ADVANCED_FACE('',(#11957),#1629,.F.);
#12977=ADVANCED_FACE('',(#11958,#11959),#1630,.T.);
#12978=ADVANCED_FACE('',(#11960,#11961),#1286,.T.);
#12979=ADVANCED_FACE('',(#11962,#11963),#1287,.T.);
#12980=ADVANCED_FACE('',(#11964,#11965),#1288,.T.);
#12981=ADVANCED_FACE('',(#11966,#11967),#1289,.T.);
#12982=ADVANCED_FACE('',(#11968,#11969),#1631,.T.);
#12983=ADVANCED_FACE('',(#11970,#11971),#1632,.T.);
#12984=ADVANCED_FACE('',(#11972,#11973),#1633,.T.);
#12985=ADVANCED_FACE('',(#11974,#11975),#307,.T.);
#12986=ADVANCED_FACE('',(#11976,#11977),#26,.T.);
#12987=ADVANCED_FACE('',(#11978,#11979),#27,.T.);
#12988=ADVANCED_FACE('',(#11980,#11981),#1634,.T.);
#12989=ADVANCED_FACE('',(#11982,#11983),#1635,.F.);
#12990=ADVANCED_FACE('',(#11984,#11985),#28,.F.);
#12991=ADVANCED_FACE('',(#11986,#11987),#29,.F.);
#12992=ADVANCED_FACE('',(#11988,#11989),#308,.F.);
#12993=ADVANCED_FACE('',(#11990,#11991),#1636,.F.);
#12994=ADVANCED_FACE('',(#11992,#11993),#309,.F.);
#12995=ADVANCED_FACE('',(#11994,#11995),#310,.T.);
#12996=ADVANCED_FACE('',(#11996,#11997),#311,.T.);
#12997=ADVANCED_FACE('',(#11998,#11999),#312,.T.);
#12998=ADVANCED_FACE('',(#12000,#12001),#313,.T.);
#12999=ADVANCED_FACE('',(#12002,#12003),#314,.T.);
#13000=ADVANCED_FACE('',(#12004,#12005),#15,.F.);
#13001=ADVANCED_FACE('',(#12006),#12684,.F.);
#13002=ADVANCED_FACE('',(#12007),#12685,.F.);
#13003=ADVANCED_FACE('',(#12008),#1637,.T.);
#13004=ADVANCED_FACE('',(#12009),#1290,.T.);
#13005=ADVANCED_FACE('',(#12010),#1291,.T.);
#13006=ADVANCED_FACE('',(#12011,#12012),#1292,.T.);
#13007=ADVANCED_FACE('',(#12013,#12014),#1293,.F.);
#13008=ADVANCED_FACE('',(#12015,#12016),#1294,.T.);
#13009=ADVANCED_FACE('',(#12017),#1638,.T.);
#13010=ADVANCED_FACE('',(#12018),#1295,.F.);
#13011=ADVANCED_FACE('',(#12019),#1296,.F.);
#13012=ADVANCED_FACE('',(#12020),#1639,.T.);
#13013=ADVANCED_FACE('',(#12021),#1297,.F.);
#13014=ADVANCED_FACE('',(#12022),#1298,.F.);
#13015=ADVANCED_FACE('',(#12023),#1640,.T.);
#13016=ADVANCED_FACE('',(#12024),#1299,.F.);
#13017=ADVANCED_FACE('',(#12025),#1300,.F.);
#13018=ADVANCED_FACE('',(#12026),#1641,.T.);
#13019=ADVANCED_FACE('',(#12027),#1301,.F.);
#13020=ADVANCED_FACE('',(#12028),#1302,.F.);
#13021=ADVANCED_FACE('',(#12029),#1642,.T.);
#13022=ADVANCED_FACE('',(#12030),#1303,.F.);
#13023=ADVANCED_FACE('',(#12031),#1304,.F.);
#13024=ADVANCED_FACE('',(#12032),#1643,.T.);
#13025=ADVANCED_FACE('',(#12033),#1305,.F.);
#13026=ADVANCED_FACE('',(#12034),#1306,.F.);
#13027=ADVANCED_FACE('',(#12035),#1644,.T.);
#13028=ADVANCED_FACE('',(#12036),#1307,.F.);
#13029=ADVANCED_FACE('',(#12037),#1308,.F.);
#13030=ADVANCED_FACE('',(#12038),#1645,.T.);
#13031=ADVANCED_FACE('',(#12039),#1309,.F.);
#13032=ADVANCED_FACE('',(#12040),#1310,.F.);
#13033=ADVANCED_FACE('',(#12041),#1646,.T.);
#13034=ADVANCED_FACE('',(#12042),#1311,.F.);
#13035=ADVANCED_FACE('',(#12043),#1312,.F.);
#13036=ADVANCED_FACE('',(#12044),#1647,.T.);
#13037=ADVANCED_FACE('',(#12045),#1313,.F.);
#13038=ADVANCED_FACE('',(#12046),#1314,.F.);
#13039=ADVANCED_FACE('',(#12047),#1648,.T.);
#13040=ADVANCED_FACE('',(#12048),#1315,.F.);
#13041=ADVANCED_FACE('',(#12049),#1316,.F.);
#13042=ADVANCED_FACE('',(#12050),#1649,.T.);
#13043=ADVANCED_FACE('',(#12051),#1317,.F.);
#13044=ADVANCED_FACE('',(#12052),#1318,.F.);
#13045=ADVANCED_FACE('',(#12053),#1650,.T.);
#13046=ADVANCED_FACE('',(#12054),#1319,.F.);
#13047=ADVANCED_FACE('',(#12055),#1320,.F.);
#13048=ADVANCED_FACE('',(#12056),#1651,.T.);
#13049=ADVANCED_FACE('',(#12057),#1321,.F.);
#13050=ADVANCED_FACE('',(#12058),#1322,.F.);
#13051=ADVANCED_FACE('',(#12059),#1652,.T.);
#13052=ADVANCED_FACE('',(#12060),#1323,.F.);
#13053=ADVANCED_FACE('',(#12061),#1324,.F.);
#13054=ADVANCED_FACE('',(#12062),#1653,.T.);
#13055=ADVANCED_FACE('',(#12063),#1325,.F.);
#13056=ADVANCED_FACE('',(#12064),#1326,.F.);
#13057=ADVANCED_FACE('',(#12065),#1654,.T.);
#13058=ADVANCED_FACE('',(#12066),#1327,.F.);
#13059=ADVANCED_FACE('',(#12067),#1328,.F.);
#13060=ADVANCED_FACE('',(#12068),#1655,.T.);
#13061=ADVANCED_FACE('',(#12069),#1329,.F.);
#13062=ADVANCED_FACE('',(#12070),#1330,.F.);
#13063=ADVANCED_FACE('',(#12071),#1656,.T.);
#13064=ADVANCED_FACE('',(#12072),#1331,.F.);
#13065=ADVANCED_FACE('',(#12073),#1332,.F.);
#13066=ADVANCED_FACE('',(#12074),#1657,.T.);
#13067=ADVANCED_FACE('',(#12075),#1333,.F.);
#13068=ADVANCED_FACE('',(#12076),#1334,.F.);
#13069=ADVANCED_FACE('',(#12077),#1658,.T.);
#13070=ADVANCED_FACE('',(#12078),#1335,.F.);
#13071=ADVANCED_FACE('',(#12079),#1336,.F.);
#13072=ADVANCED_FACE('',(#12080),#1659,.T.);
#13073=ADVANCED_FACE('',(#12081),#1337,.F.);
#13074=ADVANCED_FACE('',(#12082),#1338,.F.);
#13075=ADVANCED_FACE('',(#12083),#1660,.T.);
#13076=ADVANCED_FACE('',(#12084),#1339,.F.);
#13077=ADVANCED_FACE('',(#12085),#1340,.F.);
#13078=ADVANCED_FACE('',(#12086),#1661,.T.);
#13079=ADVANCED_FACE('',(#12087),#1341,.F.);
#13080=ADVANCED_FACE('',(#12088),#1342,.F.);
#13081=ADVANCED_FACE('',(#12089),#1662,.T.);
#13082=ADVANCED_FACE('',(#12090),#1343,.F.);
#13083=ADVANCED_FACE('',(#12091),#1344,.F.);
#13084=ADVANCED_FACE('',(#12092),#1663,.T.);
#13085=ADVANCED_FACE('',(#12093),#1345,.F.);
#13086=ADVANCED_FACE('',(#12094),#1346,.F.);
#13087=ADVANCED_FACE('',(#12095),#1664,.T.);
#13088=ADVANCED_FACE('',(#12096),#1347,.F.);
#13089=ADVANCED_FACE('',(#12097),#1348,.F.);
#13090=ADVANCED_FACE('',(#12098),#1665,.T.);
#13091=ADVANCED_FACE('',(#12099),#1349,.F.);
#13092=ADVANCED_FACE('',(#12100),#1350,.F.);
#13093=ADVANCED_FACE('',(#12101),#1666,.T.);
#13094=ADVANCED_FACE('',(#12102),#1351,.F.);
#13095=ADVANCED_FACE('',(#12103),#1352,.F.);
#13096=ADVANCED_FACE('',(#12104),#1667,.T.);
#13097=ADVANCED_FACE('',(#12105),#1353,.F.);
#13098=ADVANCED_FACE('',(#12106),#1354,.F.);
#13099=ADVANCED_FACE('',(#12107),#1668,.T.);
#13100=ADVANCED_FACE('',(#12108),#1355,.F.);
#13101=ADVANCED_FACE('',(#12109),#1356,.F.);
#13102=ADVANCED_FACE('',(#12110),#1669,.T.);
#13103=ADVANCED_FACE('',(#12111),#1357,.F.);
#13104=ADVANCED_FACE('',(#12112),#1358,.F.);
#13105=ADVANCED_FACE('',(#12113),#1670,.T.);
#13106=ADVANCED_FACE('',(#12114),#1359,.F.);
#13107=ADVANCED_FACE('',(#12115),#1360,.F.);
#13108=ADVANCED_FACE('',(#12116),#1671,.T.);
#13109=ADVANCED_FACE('',(#12117),#1361,.F.);
#13110=ADVANCED_FACE('',(#12118),#1362,.F.);
#13111=ADVANCED_FACE('',(#12119),#1672,.T.);
#13112=ADVANCED_FACE('',(#12120),#1363,.F.);
#13113=ADVANCED_FACE('',(#12121),#1364,.F.);
#13114=ADVANCED_FACE('',(#12122),#1673,.T.);
#13115=ADVANCED_FACE('',(#12123),#1365,.F.);
#13116=ADVANCED_FACE('',(#12124),#1366,.F.);
#13117=ADVANCED_FACE('',(#12125),#1674,.T.);
#13118=ADVANCED_FACE('',(#12126),#1367,.F.);
#13119=ADVANCED_FACE('',(#12127),#1368,.F.);
#13120=ADVANCED_FACE('',(#12128),#1675,.T.);
#13121=ADVANCED_FACE('',(#12129),#1369,.F.);
#13122=ADVANCED_FACE('',(#12130),#1370,.F.);
#13123=ADVANCED_FACE('',(#12131),#1676,.T.);
#13124=ADVANCED_FACE('',(#12132),#1371,.F.);
#13125=ADVANCED_FACE('',(#12133),#1372,.F.);
#13126=ADVANCED_FACE('',(#12134),#1677,.T.);
#13127=ADVANCED_FACE('',(#12135),#1373,.F.);
#13128=ADVANCED_FACE('',(#12136),#1374,.F.);
#13129=ADVANCED_FACE('',(#12137),#1678,.T.);
#13130=ADVANCED_FACE('',(#12138),#1375,.F.);
#13131=ADVANCED_FACE('',(#12139),#1376,.F.);
#13132=ADVANCED_FACE('',(#12140),#1679,.T.);
#13133=ADVANCED_FACE('',(#12141),#1377,.F.);
#13134=ADVANCED_FACE('',(#12142),#1378,.F.);
#13135=ADVANCED_FACE('',(#12143),#1680,.T.);
#13136=ADVANCED_FACE('',(#12144),#1379,.F.);
#13137=ADVANCED_FACE('',(#12145),#1380,.F.);
#13138=ADVANCED_FACE('',(#12146),#1381,.F.);
#13139=ADVANCED_FACE('',(#12147),#1382,.F.);
#13140=ADVANCED_FACE('',(#12148),#1681,.T.);
#13141=ADVANCED_FACE('',(#12149),#1383,.F.);
#13142=ADVANCED_FACE('',(#12150),#1384,.F.);
#13143=ADVANCED_FACE('',(#12151),#1682,.T.);
#13144=ADVANCED_FACE('',(#12152),#1385,.F.);
#13145=ADVANCED_FACE('',(#12153),#1386,.F.);
#13146=ADVANCED_FACE('',(#12154),#1683,.T.);
#13147=ADVANCED_FACE('',(#12155),#1387,.F.);
#13148=ADVANCED_FACE('',(#12156),#1388,.F.);
#13149=ADVANCED_FACE('',(#12157),#1684,.T.);
#13150=ADVANCED_FACE('',(#12158),#1389,.F.);
#13151=ADVANCED_FACE('',(#12159),#1390,.F.);
#13152=ADVANCED_FACE('',(#12160,#12161),#1391,.T.);
#13153=ADVANCED_FACE('',(#12162),#1685,.T.);
#13154=ADVANCED_FACE('',(#12163,#12164),#1686,.T.);
#13155=ADVANCED_FACE('',(#12165,#12166),#1687,.F.);
#13156=ADVANCED_FACE('',(#12167,#12168),#1688,.F.);
#13157=ADVANCED_FACE('',(#12169,#12170),#315,.T.);
#13158=ADVANCED_FACE('',(#12171,#12172),#316,.T.);
#13159=ADVANCED_FACE('',(#12173,#12174),#1392,.T.);
#13160=ADVANCED_FACE('',(#12175,#12176),#1393,.F.);
#13161=ADVANCED_FACE('',(#12177,#12178),#1689,.T.);
#13162=ADVANCED_FACE('',(#12179,#12180),#1690,.F.);
#13163=ADVANCED_FACE('',(#12181,#12182),#1394,.F.);
#13164=ADVANCED_FACE('',(#12183,#12184),#1395,.T.);
#13165=ADVANCED_FACE('',(#12185,#12186),#1691,.T.);
#13166=ADVANCED_FACE('',(#12187,#12188),#1692,.F.);
#13167=ADVANCED_FACE('',(#12189),#1396,.T.);
#13168=ADVANCED_FACE('',(#12190),#1693,.T.);
#13169=ADVANCED_FACE('',(#12191),#1694,.T.);
#13170=ADVANCED_FACE('',(#12192),#1397,.T.);
#13171=ADVANCED_FACE('',(#12193),#1695,.T.);
#13172=ADVANCED_FACE('',(#12194),#1696,.F.);
#13173=ADVANCED_FACE('',(#12195),#1398,.T.);
#13174=ADVANCED_FACE('',(#12196),#1399,.F.);
#13175=ADVANCED_FACE('',(#12197,#12198,#12199,#12200),#1400,.F.);
#13176=ADVANCED_FACE('',(#12201,#12202),#1697,.T.);
#13177=ADVANCED_FACE('',(#12203,#12204),#1698,.T.);
#13178=ADVANCED_FACE('',(#12205),#1699,.T.);
#13179=ADVANCED_FACE('',(#12206),#1700,.T.);
#13180=ADVANCED_FACE('',(#12207),#1701,.T.);
#13181=ADVANCED_FACE('',(#12208),#1702,.F.);
#13182=ADVANCED_FACE('',(#12209),#16,.T.);
#13183=ADVANCED_FACE('',(#12210),#1401,.F.);
#13184=ADVANCED_FACE('',(#12211),#1703,.F.);
#13185=ADVANCED_FACE('',(#12212),#1402,.F.);
#13186=ADVANCED_FACE('',(#12213),#1403,.F.);
#13187=ADVANCED_FACE('',(#12214),#1404,.F.);
#13188=ADVANCED_FACE('',(#12215),#1704,.F.);
#13189=ADVANCED_FACE('',(#12216),#1405,.F.);
#13190=ADVANCED_FACE('',(#12217),#1406,.F.);
#13191=ADVANCED_FACE('',(#12218),#1705,.F.);
#13192=ADVANCED_FACE('',(#12219,#12220),#1407,.F.);
#13193=ADVANCED_FACE('',(#12221,#12222),#1408,.F.);
#13194=ADVANCED_FACE('',(#12223,#12224),#1409,.F.);
#13195=ADVANCED_FACE('',(#12225,#12226,#12227,#12228,#12229,#12230,#12231,
#12232),#1410,.T.);
#13196=ADVANCED_FACE('',(#12233,#12234,#12235,#12236,#12237,#12238,#12239,
#12240),#1411,.F.);
#13197=ADVANCED_FACE('',(#12241,#12242),#1706,.T.);
#13198=ADVANCED_FACE('',(#12243,#12244),#1707,.F.);
#13199=ADVANCED_FACE('',(#12245,#12246),#1708,.F.);
#13200=ADVANCED_FACE('',(#12247,#12248),#1709,.F.);
#13201=ADVANCED_FACE('',(#12249,#12250),#1710,.F.);
#13202=ADVANCED_FACE('',(#12251,#12252),#1711,.F.);
#13203=ADVANCED_FACE('',(#12253,#12254),#1712,.F.);
#13204=ADVANCED_FACE('',(#12255,#12256),#1713,.F.);
#13205=ADVANCED_FACE('',(#12257),#1714,.F.);
#13206=ADVANCED_FACE('',(#12258),#1715,.F.);
#13207=ADVANCED_FACE('',(#12259),#1716,.F.);
#13208=ADVANCED_FACE('',(#12260,#12261),#317,.T.);
#13209=ADVANCED_FACE('',(#12262,#12263),#318,.T.);
#13210=ADVANCED_FACE('',(#12264,#12265),#319,.T.);
#13211=ADVANCED_FACE('',(#12266,#12267),#320,.T.);
#13212=ADVANCED_FACE('',(#12268),#17,.T.);
#13213=ADVANCED_FACE('',(#12269),#1412,.F.);
#13214=ADVANCED_FACE('',(#12270),#1413,.T.);
#13215=ADVANCED_FACE('',(#12271),#1414,.T.);
#13216=ADVANCED_FACE('',(#12272),#1717,.T.);
#13217=ADVANCED_FACE('',(#12273),#1415,.F.);
#13218=ADVANCED_FACE('',(#12274),#1416,.T.);
#13219=ADVANCED_FACE('',(#12275),#1417,.T.);
#13220=ADVANCED_FACE('',(#12276),#1718,.T.);
#13221=ADVANCED_FACE('',(#12277),#1418,.F.);
#13222=ADVANCED_FACE('',(#12278),#1419,.T.);
#13223=ADVANCED_FACE('',(#12279),#1420,.T.);
#13224=ADVANCED_FACE('',(#12280),#1719,.T.);
#13225=ADVANCED_FACE('',(#12281,#12282,#12283,#12284,#12285),#1421,.F.);
#13226=ADVANCED_FACE('',(#12286,#12287),#1422,.T.);
#13227=ADVANCED_FACE('',(#12288,#12289),#1720,.T.);
#13228=ADVANCED_FACE('',(#12290,#12291),#1721,.F.);
#13229=ADVANCED_FACE('',(#12292),#1722,.T.);
#13230=ADVANCED_FACE('',(#12293),#1723,.T.);
#13231=ADVANCED_FACE('',(#12294),#1724,.T.);
#13232=ADVANCED_FACE('',(#12295),#1423,.T.);
#13233=ADVANCED_FACE('',(#12296),#1424,.T.);
#13234=ADVANCED_FACE('',(#12297),#1425,.F.);
#13235=ADVANCED_FACE('',(#12298),#1426,.F.);
#13236=ADVANCED_FACE('',(#12299),#1427,.T.);
#13237=ADVANCED_FACE('',(#12300),#1725,.T.);
#13238=ADVANCED_FACE('',(#12301),#1726,.T.);
#13239=ADVANCED_FACE('',(#12302),#1428,.T.);
#13240=ADVANCED_FACE('',(#12303),#1727,.T.);
#13241=ADVANCED_FACE('',(#12304),#1728,.F.);
#13242=ADVANCED_FACE('',(#12305),#1429,.T.);
#13243=ADVANCED_FACE('',(#12306),#1430,.F.);
#13244=ADVANCED_FACE('',(#12307,#12308),#1431,.F.);
#13245=ADVANCED_FACE('',(#12309),#1729,.T.);
#13246=ADVANCED_FACE('',(#12310,#12311),#1432,.F.);
#13247=ADVANCED_FACE('',(#12312,#12313),#1730,.T.);
#13248=ADVANCED_FACE('',(#12314),#1731,.T.);
#13249=ADVANCED_FACE('',(#12315),#1732,.T.);
#13250=ADVANCED_FACE('',(#12316),#1733,.T.);
#13251=ADVANCED_FACE('',(#12317),#1734,.T.);
#13252=ADVANCED_FACE('',(#12318),#1735,.F.);
#13253=ADVANCED_FACE('',(#12319,#12320),#1433,.T.);
#13254=ADVANCED_FACE('',(#12321),#1736,.F.);
#13255=ADVANCED_FACE('',(#12322,#12323),#1434,.F.);
#13256=ADVANCED_FACE('',(#12324),#1737,.F.);
#13257=ADVANCED_FACE('',(#12325,#12326),#1435,.T.);
#13258=ADVANCED_FACE('',(#12327,#12328),#1436,.F.);
#13259=ADVANCED_FACE('',(#12329),#1738,.F.);
#13260=ADVANCED_FACE('',(#12330,#12331),#1437,.T.);
#13261=ADVANCED_FACE('',(#12332),#1739,.F.);
#13262=ADVANCED_FACE('',(#12333,#12334),#1438,.F.);
#13263=ADVANCED_FACE('',(#12335,#12336),#1439,.T.);
#13264=ADVANCED_FACE('',(#12337,#12338),#1440,.F.);
#13265=ADVANCED_FACE('',(#12339),#1740,.F.);
#13266=ADVANCED_FACE('',(#12340,#12341),#1441,.T.);
#13267=ADVANCED_FACE('',(#12342),#1741,.F.);
#13268=ADVANCED_FACE('',(#12343),#1442,.T.);
#13269=ADVANCED_FACE('',(#12344),#1742,.T.);
#13270=ADVANCED_FACE('',(#12345),#1443,.T.);
#13271=ADVANCED_FACE('',(#12346),#1743,.T.);
#13272=ADVANCED_FACE('',(#12347),#1444,.F.);
#13273=ADVANCED_FACE('',(#12348),#1744,.T.);
#13274=ADVANCED_FACE('',(#12349),#1445,.T.);
#13275=ADVANCED_FACE('',(#12350),#1745,.T.);
#13276=ADVANCED_FACE('',(#12351),#1446,.F.);
#13277=ADVANCED_FACE('',(#12352),#1447,.T.);
#13278=ADVANCED_FACE('',(#12353),#1746,.T.);
#13279=ADVANCED_FACE('',(#12354),#1448,.T.);
#13280=ADVANCED_FACE('',(#12355),#1747,.T.);
#13281=ADVANCED_FACE('',(#12356),#1449,.F.);
#13282=ADVANCED_FACE('',(#12357),#1450,.T.);
#13283=ADVANCED_FACE('',(#12358),#1748,.T.);
#13284=ADVANCED_FACE('',(#12359),#1451,.T.);
#13285=ADVANCED_FACE('',(#12360),#1749,.T.);
#13286=ADVANCED_FACE('',(#12361),#1452,.F.);
#13287=ADVANCED_FACE('',(#12362),#1453,.T.);
#13288=ADVANCED_FACE('',(#12363),#1454,.T.);
#13289=ADVANCED_FACE('',(#12364),#12686,.T.);
#13290=ADVANCED_FACE('',(#12365),#12687,.T.);
#13291=ADVANCED_FACE('',(#12366),#1750,.F.);
#13292=ADVANCED_FACE('',(#12367),#1455,.F.);
#13293=ADVANCED_FACE('',(#12368),#1456,.T.);
#13294=ADVANCED_FACE('',(#12369,#12370),#1457,.T.);
#13295=ADVANCED_FACE('',(#12371),#12688,.F.);
#13296=ADVANCED_FACE('',(#12372),#1751,.F.);
#13297=ADVANCED_FACE('',(#12373),#1752,.F.);
#13298=ADVANCED_FACE('',(#12374),#12689,.F.);
#13299=ADVANCED_FACE('',(#12375),#12690,.F.);
#13300=ADVANCED_FACE('',(#12376),#12691,.F.);
#13301=ADVANCED_FACE('',(#12377),#1458,.F.);
#13302=ADVANCED_FACE('',(#12378),#1459,.T.);
#13303=ADVANCED_FACE('',(#12379),#1460,.T.);
#13304=ADVANCED_FACE('',(#12380,#12381),#1461,.T.);
#13305=ADVANCED_FACE('',(#12382,#12383),#1462,.T.);
#13306=ADVANCED_FACE('',(#12384,#12385),#1463,.T.);
#13307=ADVANCED_FACE('',(#12386,#12387),#30,.F.);
#13308=ADVANCED_FACE('',(#12388,#12389),#1753,.F.);
#13309=ADVANCED_FACE('',(#12390,#12391),#1754,.T.);
#13310=ADVANCED_FACE('',(#12392,#12393),#1755,.F.);
#13311=ADVANCED_FACE('',(#12394,#12395),#1756,.F.);
#13312=ADVANCED_FACE('',(#12396,#12397),#1757,.F.);
#13313=ADVANCED_FACE('',(#12398,#12399),#321,.F.);
#13314=ADVANCED_FACE('',(#12400),#12692,.T.);
#13315=ADVANCED_FACE('',(#12401,#12402),#322,.F.);
#13316=ADVANCED_FACE('',(#12403,#12404),#323,.T.);
#13317=ADVANCED_FACE('',(#12405,#12406),#324,.T.);
#13318=ADVANCED_FACE('',(#12407,#12408),#325,.T.);
#13319=ADVANCED_FACE('',(#12409,#12410),#1758,.T.);
#13320=ADVANCED_FACE('',(#12411,#12412),#326,.T.);
#13321=ADVANCED_FACE('',(#12413,#12414),#327,.F.);
#13322=ADVANCED_FACE('',(#12415,#12416),#328,.T.);
#13323=ADVANCED_FACE('',(#12417,#12418),#329,.F.);
#13324=ADVANCED_FACE('',(#12419,#12420),#330,.T.);
#13325=ADVANCED_FACE('',(#12421,#12422),#1759,.F.);
#13326=ADVANCED_FACE('',(#12423,#12424),#1760,.F.);
#13327=ADVANCED_FACE('',(#12425,#12426),#1761,.F.);
#13328=ADVANCED_FACE('',(#12427,#12428),#1762,.F.);
#13329=ADVANCED_FACE('',(#12429,#12430),#1763,.T.);
#13330=ADVANCED_FACE('',(#12431),#1764,.F.);
#13331=ADVANCED_FACE('',(#12432),#1765,.F.);
#13332=ADVANCED_FACE('',(#12433,#12434,#12435,#12436,#12437,#12438),#1766,
 .F.);
#13333=ADVANCED_FACE('',(#12439),#1464,.F.);
#13334=ADVANCED_FACE('',(#12440),#1465,.T.);
#13335=ADVANCED_FACE('',(#12441),#1466,.T.);
#13336=ADVANCED_FACE('',(#12442),#1767,.T.);
#13337=ADVANCED_FACE('',(#12443),#1467,.F.);
#13338=ADVANCED_FACE('',(#12444),#1468,.T.);
#13339=ADVANCED_FACE('',(#12445),#1469,.T.);
#13340=ADVANCED_FACE('',(#12446),#1768,.T.);
#13341=ADVANCED_FACE('',(#12447),#1470,.F.);
#13342=ADVANCED_FACE('',(#12448),#1471,.T.);
#13343=ADVANCED_FACE('',(#12449),#1472,.T.);
#13344=ADVANCED_FACE('',(#12450),#1769,.T.);
#13345=ADVANCED_FACE('',(#12451,#12452,#12453,#12454,#12455,#12456,#12457,
#12458,#12459),#1473,.F.);
#13346=ADVANCED_FACE('',(#12460,#12461,#12462,#12463,#12464,#12465),#1474,
 .T.);
#13347=ADVANCED_FACE('',(#12466,#12467),#1770,.T.);
#13348=ADVANCED_FACE('',(#12468,#12469),#1771,.F.);
#13349=ADVANCED_FACE('',(#12470,#12471),#1772,.F.);
#13350=ADVANCED_FACE('',(#12472,#12473),#1773,.F.);
#13351=ADVANCED_FACE('',(#12474,#12475),#1774,.F.);
#13352=ADVANCED_FACE('',(#12476),#1775,.T.);
#13353=ADVANCED_FACE('',(#12477),#1776,.T.);
#13354=ADVANCED_FACE('',(#12478),#1777,.T.);
#13355=ADVANCED_FACE('',(#12479,#12480),#1778,.F.);
#13356=ADVANCED_FACE('',(#12481),#12693,.F.);
#13357=ADVANCED_FACE('',(#12482),#12694,.F.);
#13358=ADVANCED_FACE('',(#12483),#55,.F.);
#13359=ADVANCED_FACE('',(#12484),#1475,.F.);
#13360=ADVANCED_FACE('',(#12485),#1476,.T.);
#13361=ADVANCED_FACE('',(#12486),#1477,.F.);
#13362=ADVANCED_FACE('',(#12487),#1478,.F.);
#13363=ADVANCED_FACE('',(#12488),#1479,.F.);
#13364=ADVANCED_FACE('',(#12489),#1480,.F.);
#13365=ADVANCED_FACE('',(#12490),#1481,.F.);
#13366=ADVANCED_FACE('',(#12491),#1482,.F.);
#13367=ADVANCED_FACE('',(#12492),#1483,.F.);
#13368=ADVANCED_FACE('',(#12493),#1484,.F.);
#13369=ADVANCED_FACE('',(#12494),#1485,.F.);
#13370=ADVANCED_FACE('',(#12495),#1486,.F.);
#13371=ADVANCED_FACE('',(#12496),#1487,.F.);
#13372=ADVANCED_FACE('',(#12497),#1488,.F.);
#13373=ADVANCED_FACE('',(#12498),#1489,.F.);
#13374=ADVANCED_FACE('',(#12499),#1490,.F.);
#13375=ADVANCED_FACE('',(#12500),#1491,.F.);
#13376=ADVANCED_FACE('',(#12501),#1492,.F.);
#13377=ADVANCED_FACE('',(#12502),#1493,.F.);
#13378=ADVANCED_FACE('',(#12503),#1494,.F.);
#13379=ADVANCED_FACE('',(#12504),#1495,.F.);
#13380=ADVANCED_FACE('',(#12505),#1496,.F.);
#13381=ADVANCED_FACE('',(#12506),#1497,.F.);
#13382=ADVANCED_FACE('',(#12507),#1498,.F.);
#13383=ADVANCED_FACE('',(#12508),#1499,.F.);
#13384=ADVANCED_FACE('',(#12509),#1500,.F.);
#13385=ADVANCED_FACE('',(#12510),#1501,.F.);
#13386=ADVANCED_FACE('',(#12511),#1502,.F.);
#13387=ADVANCED_FACE('',(#12512),#1503,.F.);
#13388=ADVANCED_FACE('',(#12513),#1504,.F.);
#13389=ADVANCED_FACE('',(#12514),#1505,.F.);
#13390=ADVANCED_FACE('',(#12515),#1506,.F.);
#13391=ADVANCED_FACE('',(#12516),#1507,.F.);
#13392=ADVANCED_FACE('',(#12517),#1508,.F.);
#13393=ADVANCED_FACE('',(#12518),#1509,.F.);
#13394=ADVANCED_FACE('',(#12519,#12520),#1510,.T.);
#13395=ADVANCED_FACE('',(#12521,#12522),#1511,.F.);
#13396=ADVANCED_FACE('',(#12523),#1779,.T.);
#13397=ADVANCED_FACE('',(#12524,#12525),#1512,.F.);
#13398=ADVANCED_FACE('',(#12526),#1780,.T.);
#13399=ADVANCED_FACE('',(#12527),#1781,.T.);
#13400=ADVANCED_FACE('',(#12528),#1782,.T.);
#13401=ADVANCED_FACE('',(#12529),#1783,.T.);
#13402=ADVANCED_FACE('',(#12530),#1784,.T.);
#13403=ADVANCED_FACE('',(#12531),#1785,.T.);
#13404=ADVANCED_FACE('',(#12532),#1786,.T.);
#13405=ADVANCED_FACE('',(#12533),#1787,.T.);
#13406=ADVANCED_FACE('',(#12534),#1788,.T.);
#13407=ADVANCED_FACE('',(#12535),#1789,.T.);
#13408=ADVANCED_FACE('',(#12536,#12537),#1790,.T.);
#13409=ADVANCED_FACE('',(#12538,#12539),#1791,.F.);
#13410=ADVANCED_FACE('',(#12540),#1513,.F.);
#13411=ADVANCED_FACE('',(#12541),#1792,.F.);
#13412=ADVANCED_FACE('',(#12542),#1793,.T.);
#13413=ADVANCED_FACE('',(#12543),#1514,.F.);
#13414=ADVANCED_FACE('',(#12544),#1794,.F.);
#13415=ADVANCED_FACE('',(#12545),#1795,.F.);
#13416=ADVANCED_FACE('',(#12546),#1515,.F.);
#13417=ADVANCED_FACE('',(#12547),#12695,.F.);
#13418=ADVANCED_FACE('',(#12548),#12696,.F.);
#13419=ADVANCED_FACE('',(#12549),#1796,.T.);
#13420=ADVANCED_FACE('',(#12550),#1516,.T.);
#13421=ADVANCED_FACE('',(#12551),#1517,.F.);
#13422=ADVANCED_FACE('',(#12552),#1797,.F.);
#13423=ADVANCED_FACE('',(#12553,#12554),#1518,.F.);
#13424=ADVANCED_FACE('',(#12555),#1798,.F.);
#13425=ADVANCED_FACE('',(#12556,#12557,#12558),#1519,.F.);
#13426=ADVANCED_FACE('',(#12559),#1520,.T.);
#13427=ADVANCED_FACE('',(#12560),#1521,.T.);
#13428=ADVANCED_FACE('',(#12561),#1799,.T.);
#13429=ADVANCED_FACE('',(#12562,#12563,#12564,#12565,#12566),#1522,.T.);
#13430=ADVANCED_FACE('',(#12567,#12568),#1800,.T.);
#13431=ADVANCED_FACE('',(#12569),#1801,.F.);
#13432=ADVANCED_FACE('',(#12570,#12571),#1802,.F.);
#13433=ADVANCED_FACE('',(#12572,#12573),#1803,.F.);
#13434=ADVANCED_FACE('',(#12574,#12575),#31,.F.);
#13435=ADVANCED_FACE('',(#12576),#1804,.T.);
#13436=ADVANCED_FACE('',(#12577),#1805,.F.);
#13437=ADVANCED_FACE('',(#12578),#1806,.T.);
#13438=ADVANCED_FACE('',(#12579),#1807,.F.);
#13439=ADVANCED_FACE('',(#12580),#1808,.F.);
#13440=ADVANCED_FACE('',(#12581),#1523,.F.);
#13441=ADVANCED_FACE('',(#12582),#1809,.F.);
#13442=ADVANCED_FACE('',(#12583),#1524,.F.);
#13443=ADVANCED_FACE('',(#12584),#1810,.T.);
#13444=ADVANCED_FACE('',(#12585),#1525,.T.);
#13445=ADVANCED_FACE('',(#12586),#1811,.F.);
#13446=ADVANCED_FACE('',(#12587),#1526,.T.);
#13447=ADVANCED_FACE('',(#12588),#1812,.T.);
#13448=ADVANCED_FACE('',(#12589),#1527,.F.);
#13449=ADVANCED_FACE('',(#12590),#1813,.F.);
#13450=ADVANCED_FACE('',(#12591),#1528,.T.);
#13451=ADVANCED_FACE('',(#12592),#1814,.T.);
#13452=ADVANCED_FACE('',(#12593),#1529,.T.);
#13453=ADVANCED_FACE('',(#12594),#1815,.F.);
#13454=ADVANCED_FACE('',(#12595),#1530,.F.);
#13455=ADVANCED_FACE('',(#12596),#1816,.T.);
#13456=ADVANCED_FACE('',(#12597,#12598),#1531,.T.);
#13457=ADVANCED_FACE('',(#12599,#12600),#1532,.T.);
#13458=ADVANCED_FACE('',(#12601,#12602),#1533,.T.);
#13459=ADVANCED_FACE('',(#12603,#12604),#1534,.T.);
#13460=ADVANCED_FACE('',(#12605),#32,.F.);
#13461=ADVANCED_FACE('',(#12606),#33,.F.);
#13462=ADVANCED_FACE('',(#12607),#34,.F.);
#13463=ADVANCED_FACE('',(#12608),#35,.T.);
#13464=ADVANCED_FACE('',(#12609),#36,.T.);
#13465=ADVANCED_FACE('',(#12610),#37,.T.);
#13466=ADVANCED_FACE('',(#12611,#12612),#1817,.F.);
#13467=ADVANCED_FACE('',(#12613),#38,.T.);
#13468=ADVANCED_FACE('',(#12614,#12615),#1818,.T.);
#13469=ADVANCED_FACE('',(#12616,#12617),#331,.T.);
#13470=ADVANCED_FACE('',(#12618),#39,.F.);
#13471=ADVANCED_FACE('',(#12619),#12697,.F.);
#13472=ADVANCED_FACE('',(#12620),#18,.F.);
#13473=ADVANCED_FACE('',(#12621),#56,.F.);
#13474=ADVANCED_FACE('',(#12622),#19,.F.);
#13475=ADVANCED_FACE('',(#12623),#12698,.F.);
#13476=ADVANCED_FACE('',(#12624),#12699,.F.);
#13477=ADVANCED_FACE('',(#12625),#1819,.F.);
#13478=ADVANCED_FACE('',(#12626),#57,.F.);
#13479=ADVANCED_FACE('',(#12627),#20,.F.);
#13480=ADVANCED_FACE('',(#12628),#12700,.F.);
#13481=ADVANCED_FACE('',(#12629),#58,.T.);
#13482=ADVANCED_FACE('',(#12630),#1820,.T.);
#13483=ADVANCED_FACE('',(#12631),#1821,.T.);
#13484=ADVANCED_FACE('',(#12632),#59,.T.);
#13485=ADVANCED_FACE('',(#12633,#12634),#1535,.F.);
#13486=ADVANCED_FACE('',(#12635,#12636),#1536,.F.);
#13487=ADVANCED_FACE('',(#12637,#12638),#1537,.F.);
#13488=ADVANCED_FACE('',(#12639),#12701,.F.);
#13489=ADVANCED_FACE('',(#12640),#12702,.F.);
#13490=ADVANCED_FACE('',(#12641),#12703,.F.);
#13491=ADVANCED_FACE('',(#12642),#12704,.F.);
#13492=ADVANCED_FACE('',(#12643,#12644,#12645),#1822,.F.);
#13493=ADVANCED_FACE('',(#12646,#12647),#1823,.F.);
#13494=ADVANCED_FACE('',(#12648,#12649),#1824,.T.);
#13495=ADVANCED_FACE('',(#12650),#12705,.F.);
#13496=ADVANCED_FACE('',(#12651,#12652),#332,.T.);
#13497=ADVANCED_FACE('',(#12653,#12654),#333,.F.);
#13498=ADVANCED_FACE('',(#12655,#12656),#334,.T.);
#13499=ADVANCED_FACE('',(#12657,#12658),#335,.T.);
#13500=ADVANCED_FACE('',(#12659,#12660),#1825,.T.);
#13501=ADVANCED_FACE('',(#12661,#12662),#336,.T.);
#13502=CLOSED_SHELL('',(#12706,#12707,#12708,#12709,#12710,#12711,#12712,
#12713,#12714,#12715,#12716,#12717,#12718,#12719,#12720,#12721,#12722,#12723,
#12724,#12725,#12726,#12727,#12728,#12729,#12730,#12731,#12732,#12733,#12734,
#12735,#12736,#12737,#12738,#12739,#12740,#12741,#12742,#12743,#12744,#12745,
#12746,#12747,#12748,#12749,#12750,#12751,#12752,#12753,#12754,#12755));
#13503=CLOSED_SHELL('',(#12756,#12757,#12758,#12759,#12760,#12761,#12762,
#12763,#12764,#12765,#12766,#12767,#12768,#12769,#12770,#12771,#12772,#12773,
#12774,#12775,#12776,#12777,#12778,#12779,#12780,#12781,#12782,#12783,#12784,
#12785,#12786,#12787,#12788,#12789,#12790,#12791,#12792,#12793,#12794,#12795,
#12796,#12797,#12798));
#13504=CLOSED_SHELL('',(#12799,#12800,#12801,#12802,#12803,#12804,#12805,
#12806,#12807,#12808,#12809,#12810,#12811,#12812,#12813,#12814));
#13505=CLOSED_SHELL('',(#12815,#12816,#12817,#12818,#12819,#12820,#12821,
#12822,#12823,#12824,#12825));
#13506=CLOSED_SHELL('',(#12826,#12827,#12828));
#13507=CLOSED_SHELL('',(#12829,#12830,#12831,#12832,#12833,#12834,#12835,
#12836,#12837,#12838,#12839,#12840,#12841,#12842,#12843,#12844,#12845,#12846,
#12847,#12848,#12849,#12850,#12851,#12852,#12853,#12854,#12855,#12856,#12857,
#12858,#12859,#12860,#12861,#12862,#12863,#12864,#12865,#12866,#12867,#12868,
#12869,#12870,#12871,#12872,#12873,#12874,#12875,#12876,#12877,#12878,#12879,
#12880,#12881,#12882,#12883,#12884,#12885,#12886,#12887,#12888,#12889,#12890,
#12891,#12892,#12893,#12894,#12895,#12896,#12897,#12898,#12899,#12900,#12901,
#12902,#12903,#12904,#12905,#12906,#12907,#12908,#12909,#12910,#12911,#12912,
#12913,#12914,#12915,#12916,#12917));
#13508=CLOSED_SHELL('',(#12918,#12919,#12920,#12921,#12922,#12923,#12924,
#12925,#12926,#12927,#12928,#12929,#12930,#12931,#12932,#12933,#12934,#12935));
#13509=CLOSED_SHELL('',(#12936,#12937,#12938,#12939,#12940,#12941,#12942));
#13510=CLOSED_SHELL('',(#12943,#12944,#12945,#12946,#12947,#12948,#12949,
#12950,#12951,#12952,#12953));
#13511=CLOSED_SHELL('',(#12954,#12955,#12956,#12957,#12958,#12959,#12960,
#12961,#12962,#12963,#12964,#12965,#12966,#12967,#12968,#12969,#12970,#12971,
#12972,#12973,#12974,#12975,#12976,#12977));
#13512=CLOSED_SHELL('',(#12978,#12979,#12980,#12981,#12982,#12983,#12984,
#12985,#12986,#12987,#12988,#12989,#12990,#12991,#12992,#12993,#12994,#12995,
#12996,#12997,#12998,#12999));
#13513=CLOSED_SHELL('',(#13000,#13001,#13002,#13003,#13004,#13005,#13006,
#13007,#13008,#13009,#13010,#13011,#13012,#13013,#13014,#13015,#13016,#13017,
#13018,#13019,#13020,#13021,#13022,#13023,#13024,#13025,#13026,#13027,#13028,
#13029,#13030,#13031,#13032,#13033,#13034,#13035,#13036,#13037,#13038,#13039,
#13040,#13041,#13042,#13043,#13044,#13045,#13046,#13047,#13048,#13049,#13050,
#13051,#13052,#13053,#13054,#13055,#13056,#13057,#13058,#13059,#13060,#13061,
#13062,#13063,#13064,#13065,#13066,#13067,#13068,#13069,#13070,#13071,#13072,
#13073,#13074,#13075,#13076,#13077,#13078,#13079,#13080,#13081,#13082,#13083,
#13084,#13085,#13086,#13087,#13088,#13089,#13090,#13091,#13092,#13093,#13094,
#13095,#13096,#13097,#13098,#13099,#13100,#13101,#13102,#13103,#13104,#13105,
#13106,#13107,#13108,#13109,#13110,#13111,#13112,#13113,#13114,#13115,#13116,
#13117,#13118,#13119,#13120,#13121,#13122,#13123,#13124,#13125,#13126,#13127,
#13128,#13129,#13130,#13131,#13132,#13133,#13134,#13135,#13136,#13137,#13138,
#13139,#13140,#13141,#13142,#13143,#13144,#13145,#13146,#13147,#13148,#13149,
#13150,#13151,#13152,#13153,#13154,#13155,#13156,#13157,#13158));
#13514=CLOSED_SHELL('',(#13159,#13160,#13161,#13162));
#13515=CLOSED_SHELL('',(#13163,#13164,#13165,#13166));
#13516=CLOSED_SHELL('',(#13167,#13168,#13169,#13170,#13171,#13172,#13173,
#13174,#13175,#13176,#13177,#13178,#13179,#13180,#13181));
#13517=CLOSED_SHELL('',(#13182));
#13518=CLOSED_SHELL('',(#13183,#13184,#13185,#13186,#13187,#13188,#13189,
#13190,#13191,#13192,#13193,#13194,#13195,#13196,#13197,#13198,#13199,#13200,
#13201,#13202,#13203,#13204,#13205,#13206,#13207,#13208,#13209,#13210,#13211));
#13519=CLOSED_SHELL('',(#13212));
#13520=CLOSED_SHELL('',(#13213,#13214,#13215,#13216,#13217,#13218,#13219,
#13220,#13221,#13222,#13223,#13224,#13225,#13226,#13227,#13228,#13229,#13230,
#13231));
#13521=CLOSED_SHELL('',(#13232,#13233,#13234,#13235,#13236,#13237,#13238,
#13239,#13240,#13241,#13242,#13243,#13244,#13245,#13246,#13247,#13248,#13249,
#13250,#13251,#13252));
#13522=CLOSED_SHELL('',(#13253,#13254,#13255,#13256,#13257,#13258,#13259,
#13260,#13261,#13262,#13263,#13264,#13265,#13266,#13267,#13268,#13269,#13270,
#13271,#13272,#13273,#13274,#13275,#13276,#13277,#13278,#13279,#13280,#13281,
#13282,#13283,#13284,#13285,#13286,#13287,#13288,#13289,#13290,#13291,#13292,
#13293,#13294,#13295,#13296,#13297,#13298,#13299,#13300,#13301,#13302,#13303,
#13304,#13305,#13306,#13307,#13308,#13309,#13310,#13311,#13312,#13313,#13314,
#13315,#13316,#13317,#13318,#13319,#13320,#13321,#13322,#13323,#13324,#13325,
#13326,#13327,#13328,#13329,#13330,#13331,#13332));
#13523=CLOSED_SHELL('',(#13333,#13334,#13335,#13336,#13337,#13338,#13339,
#13340,#13341,#13342,#13343,#13344,#13345,#13346,#13347,#13348,#13349,#13350,
#13351,#13352,#13353,#13354,#13355));
#13524=CLOSED_SHELL('',(#13356,#13357,#13358,#13359,#13360,#13361,#13362,
#13363,#13364,#13365,#13366,#13367,#13368,#13369,#13370,#13371,#13372,#13373,
#13374,#13375,#13376,#13377,#13378,#13379,#13380,#13381,#13382,#13383,#13384,
#13385,#13386,#13387,#13388,#13389,#13390,#13391,#13392,#13393,#13394,#13395,
#13396,#13397,#13398,#13399,#13400,#13401,#13402,#13403,#13404,#13405,#13406,
#13407,#13408,#13409));
#13525=CLOSED_SHELL('',(#13410,#13411,#13412,#13413,#13414,#13415,#13416,
#13417,#13418,#13419,#13420,#13421,#13422,#13423,#13424,#13425,#13426,#13427,
#13428,#13429,#13430,#13431,#13432,#13433,#13434,#13435,#13436,#13437,#13438,
#13439));
#13526=CLOSED_SHELL('',(#13440,#13441,#13442,#13443,#13444,#13445,#13446,
#13447,#13448,#13449,#13450,#13451,#13452,#13453,#13454,#13455,#13456,#13457,
#13458,#13459,#13460,#13461,#13462,#13463,#13464,#13465,#13466,#13467,#13468,
#13469,#13470));
#13527=CLOSED_SHELL('',(#13471,#13472,#13473,#13474,#13475,#13476,#13477,
#13478,#13479,#13480,#13481,#13482,#13483,#13484,#13485,#13486,#13487,#13488,
#13489,#13490,#13491,#13492,#13493,#13494,#13495,#13496,#13497,#13498,#13499));
#13528=CLOSED_SHELL('',(#13500,#13501));
#13529=STYLED_ITEM('',(#13556),#13719);
#13530=STYLED_ITEM('',(#13557),#13720);
#13531=STYLED_ITEM('',(#13558),#13721);
#13532=STYLED_ITEM('',(#13559),#13722);
#13533=STYLED_ITEM('',(#13560),#13723);
#13534=STYLED_ITEM('',(#13561),#13724);
#13535=STYLED_ITEM('',(#13562),#13725);
#13536=STYLED_ITEM('',(#13563),#13726);
#13537=STYLED_ITEM('',(#13564),#13727);
#13538=STYLED_ITEM('',(#13565),#13728);
#13539=STYLED_ITEM('',(#13566),#13729);
#13540=STYLED_ITEM('',(#13567),#13730);
#13541=STYLED_ITEM('',(#13568),#13731);
#13542=STYLED_ITEM('',(#13569),#13732);
#13543=STYLED_ITEM('',(#13570),#13733);
#13544=STYLED_ITEM('',(#13571),#13734);
#13545=STYLED_ITEM('',(#13572),#13735);
#13546=STYLED_ITEM('',(#13573),#13736);
#13547=STYLED_ITEM('',(#13574),#13737);
#13548=STYLED_ITEM('',(#13575),#13738);
#13549=STYLED_ITEM('',(#13576),#13739);
#13550=STYLED_ITEM('',(#13577),#13740);
#13551=STYLED_ITEM('',(#13578),#13741);
#13552=STYLED_ITEM('',(#13579),#13742);
#13553=STYLED_ITEM('',(#13580),#13743);
#13554=STYLED_ITEM('',(#13581),#13744);
#13555=STYLED_ITEM('',(#13582),#13745);
#13556=PRESENTATION_STYLE_ASSIGNMENT((#13583));
#13557=PRESENTATION_STYLE_ASSIGNMENT((#13584));
#13558=PRESENTATION_STYLE_ASSIGNMENT((#13585));
#13559=PRESENTATION_STYLE_ASSIGNMENT((#13586));
#13560=PRESENTATION_STYLE_ASSIGNMENT((#13587));
#13561=PRESENTATION_STYLE_ASSIGNMENT((#13588));
#13562=PRESENTATION_STYLE_ASSIGNMENT((#13589));
#13563=PRESENTATION_STYLE_ASSIGNMENT((#13590));
#13564=PRESENTATION_STYLE_ASSIGNMENT((#13591));
#13565=PRESENTATION_STYLE_ASSIGNMENT((#13592));
#13566=PRESENTATION_STYLE_ASSIGNMENT((#13593));
#13567=PRESENTATION_STYLE_ASSIGNMENT((#13594));
#13568=PRESENTATION_STYLE_ASSIGNMENT((#13595));
#13569=PRESENTATION_STYLE_ASSIGNMENT((#13596));
#13570=PRESENTATION_STYLE_ASSIGNMENT((#13597));
#13571=PRESENTATION_STYLE_ASSIGNMENT((#13598));
#13572=PRESENTATION_STYLE_ASSIGNMENT((#13599));
#13573=PRESENTATION_STYLE_ASSIGNMENT((#13600));
#13574=PRESENTATION_STYLE_ASSIGNMENT((#13601));
#13575=PRESENTATION_STYLE_ASSIGNMENT((#13602));
#13576=PRESENTATION_STYLE_ASSIGNMENT((#13603));
#13577=PRESENTATION_STYLE_ASSIGNMENT((#13604));
#13578=PRESENTATION_STYLE_ASSIGNMENT((#13605));
#13579=PRESENTATION_STYLE_ASSIGNMENT((#13606));
#13580=PRESENTATION_STYLE_ASSIGNMENT((#13607));
#13581=PRESENTATION_STYLE_ASSIGNMENT((#13608));
#13582=PRESENTATION_STYLE_ASSIGNMENT((#13609));
#13583=SURFACE_STYLE_USAGE(.BOTH.,#13610);
#13584=SURFACE_STYLE_USAGE(.BOTH.,#13611);
#13585=SURFACE_STYLE_USAGE(.BOTH.,#13612);
#13586=SURFACE_STYLE_USAGE(.BOTH.,#13613);
#13587=SURFACE_STYLE_USAGE(.BOTH.,#13614);
#13588=SURFACE_STYLE_USAGE(.BOTH.,#13615);
#13589=SURFACE_STYLE_USAGE(.BOTH.,#13616);
#13590=SURFACE_STYLE_USAGE(.BOTH.,#13617);
#13591=SURFACE_STYLE_USAGE(.BOTH.,#13618);
#13592=SURFACE_STYLE_USAGE(.BOTH.,#13619);
#13593=SURFACE_STYLE_USAGE(.BOTH.,#13620);
#13594=SURFACE_STYLE_USAGE(.BOTH.,#13621);
#13595=SURFACE_STYLE_USAGE(.BOTH.,#13622);
#13596=SURFACE_STYLE_USAGE(.BOTH.,#13623);
#13597=SURFACE_STYLE_USAGE(.BOTH.,#13624);
#13598=SURFACE_STYLE_USAGE(.BOTH.,#13625);
#13599=SURFACE_STYLE_USAGE(.BOTH.,#13626);
#13600=SURFACE_STYLE_USAGE(.BOTH.,#13627);
#13601=SURFACE_STYLE_USAGE(.BOTH.,#13628);
#13602=SURFACE_STYLE_USAGE(.BOTH.,#13629);
#13603=SURFACE_STYLE_USAGE(.BOTH.,#13630);
#13604=SURFACE_STYLE_USAGE(.BOTH.,#13631);
#13605=SURFACE_STYLE_USAGE(.BOTH.,#13632);
#13606=SURFACE_STYLE_USAGE(.BOTH.,#13633);
#13607=SURFACE_STYLE_USAGE(.BOTH.,#13634);
#13608=SURFACE_STYLE_USAGE(.BOTH.,#13635);
#13609=SURFACE_STYLE_USAGE(.BOTH.,#13636);
#13610=SURFACE_SIDE_STYLE('',(#13637));
#13611=SURFACE_SIDE_STYLE('',(#13638));
#13612=SURFACE_SIDE_STYLE('',(#13639));
#13613=SURFACE_SIDE_STYLE('',(#13640));
#13614=SURFACE_SIDE_STYLE('',(#13641));
#13615=SURFACE_SIDE_STYLE('',(#13642));
#13616=SURFACE_SIDE_STYLE('',(#13643));
#13617=SURFACE_SIDE_STYLE('',(#13644));
#13618=SURFACE_SIDE_STYLE('',(#13645));
#13619=SURFACE_SIDE_STYLE('',(#13646));
#13620=SURFACE_SIDE_STYLE('',(#13647));
#13621=SURFACE_SIDE_STYLE('',(#13648));
#13622=SURFACE_SIDE_STYLE('',(#13649));
#13623=SURFACE_SIDE_STYLE('',(#13650));
#13624=SURFACE_SIDE_STYLE('',(#13651));
#13625=SURFACE_SIDE_STYLE('',(#13652));
#13626=SURFACE_SIDE_STYLE('',(#13653));
#13627=SURFACE_SIDE_STYLE('',(#13654));
#13628=SURFACE_SIDE_STYLE('',(#13655));
#13629=SURFACE_SIDE_STYLE('',(#13656));
#13630=SURFACE_SIDE_STYLE('',(#13657));
#13631=SURFACE_SIDE_STYLE('',(#13658));
#13632=SURFACE_SIDE_STYLE('',(#13659));
#13633=SURFACE_SIDE_STYLE('',(#13660));
#13634=SURFACE_SIDE_STYLE('',(#13661));
#13635=SURFACE_SIDE_STYLE('',(#13662));
#13636=SURFACE_SIDE_STYLE('',(#13663));
#13637=SURFACE_STYLE_FILL_AREA(#13664);
#13638=SURFACE_STYLE_FILL_AREA(#13665);
#13639=SURFACE_STYLE_FILL_AREA(#13666);
#13640=SURFACE_STYLE_FILL_AREA(#13667);
#13641=SURFACE_STYLE_FILL_AREA(#13668);
#13642=SURFACE_STYLE_FILL_AREA(#13669);
#13643=SURFACE_STYLE_FILL_AREA(#13670);
#13644=SURFACE_STYLE_FILL_AREA(#13671);
#13645=SURFACE_STYLE_FILL_AREA(#13672);
#13646=SURFACE_STYLE_FILL_AREA(#13673);
#13647=SURFACE_STYLE_FILL_AREA(#13674);
#13648=SURFACE_STYLE_FILL_AREA(#13675);
#13649=SURFACE_STYLE_FILL_AREA(#13676);
#13650=SURFACE_STYLE_FILL_AREA(#13677);
#13651=SURFACE_STYLE_FILL_AREA(#13678);
#13652=SURFACE_STYLE_FILL_AREA(#13679);
#13653=SURFACE_STYLE_FILL_AREA(#13680);
#13654=SURFACE_STYLE_FILL_AREA(#13681);
#13655=SURFACE_STYLE_FILL_AREA(#13682);
#13656=SURFACE_STYLE_FILL_AREA(#13683);
#13657=SURFACE_STYLE_FILL_AREA(#13684);
#13658=SURFACE_STYLE_FILL_AREA(#13685);
#13659=SURFACE_STYLE_FILL_AREA(#13686);
#13660=SURFACE_STYLE_FILL_AREA(#13687);
#13661=SURFACE_STYLE_FILL_AREA(#13688);
#13662=SURFACE_STYLE_FILL_AREA(#13689);
#13663=SURFACE_STYLE_FILL_AREA(#13690);
#13664=FILL_AREA_STYLE('',(#13691));
#13665=FILL_AREA_STYLE('',(#13692));
#13666=FILL_AREA_STYLE('',(#13693));
#13667=FILL_AREA_STYLE('',(#13694));
#13668=FILL_AREA_STYLE('',(#13695));
#13669=FILL_AREA_STYLE('',(#13696));
#13670=FILL_AREA_STYLE('',(#13697));
#13671=FILL_AREA_STYLE('',(#13698));
#13672=FILL_AREA_STYLE('',(#13699));
#13673=FILL_AREA_STYLE('',(#13700));
#13674=FILL_AREA_STYLE('',(#13701));
#13675=FILL_AREA_STYLE('',(#13702));
#13676=FILL_AREA_STYLE('',(#13703));
#13677=FILL_AREA_STYLE('',(#13704));
#13678=FILL_AREA_STYLE('',(#13705));
#13679=FILL_AREA_STYLE('',(#13706));
#13680=FILL_AREA_STYLE('',(#13707));
#13681=FILL_AREA_STYLE('',(#13708));
#13682=FILL_AREA_STYLE('',(#13709));
#13683=FILL_AREA_STYLE('',(#13710));
#13684=FILL_AREA_STYLE('',(#13711));
#13685=FILL_AREA_STYLE('',(#13712));
#13686=FILL_AREA_STYLE('',(#13713));
#13687=FILL_AREA_STYLE('',(#13714));
#13688=FILL_AREA_STYLE('',(#13715));
#13689=FILL_AREA_STYLE('',(#13716));
#13690=FILL_AREA_STYLE('',(#13717));
#13691=FILL_AREA_STYLE_COLOUR('',#13718);
#13692=FILL_AREA_STYLE_COLOUR('',#60);
#13693=FILL_AREA_STYLE_COLOUR('',#61);
#13694=FILL_AREA_STYLE_COLOUR('',#60);
#13695=FILL_AREA_STYLE_COLOUR('',#60);
#13696=FILL_AREA_STYLE_COLOUR('',#60);
#13697=FILL_AREA_STYLE_COLOUR('',#62);
#13698=FILL_AREA_STYLE_COLOUR('',#60);
#13699=FILL_AREA_STYLE_COLOUR('',#60);
#13700=FILL_AREA_STYLE_COLOUR('',#60);
#13701=FILL_AREA_STYLE_COLOUR('',#60);
#13702=FILL_AREA_STYLE_COLOUR('',#63);
#13703=FILL_AREA_STYLE_COLOUR('',#60);
#13704=FILL_AREA_STYLE_COLOUR('',#60);
#13705=FILL_AREA_STYLE_COLOUR('',#60);
#13706=FILL_AREA_STYLE_COLOUR('',#60);
#13707=FILL_AREA_STYLE_COLOUR('',#60);
#13708=FILL_AREA_STYLE_COLOUR('',#60);
#13709=FILL_AREA_STYLE_COLOUR('',#60);
#13710=FILL_AREA_STYLE_COLOUR('',#60);
#13711=FILL_AREA_STYLE_COLOUR('',#13718);
#13712=FILL_AREA_STYLE_COLOUR('',#60);
#13713=FILL_AREA_STYLE_COLOUR('',#60);
#13714=FILL_AREA_STYLE_COLOUR('',#60);
#13715=FILL_AREA_STYLE_COLOUR('',#60);
#13716=FILL_AREA_STYLE_COLOUR('',#60);
#13717=FILL_AREA_STYLE_COLOUR('',#64);
#13718=COLOUR_RGB('', 0.09019608, 0.27058824, 0.51372549);
#13719=MANIFOLD_SOLID_BREP('Top_acces_nozzle_supporter',#13502);
#13720=MANIFOLD_SOLID_BREP('piston',#13503);
#13721=MANIFOLD_SOLID_BREP('75632s_.prt',#13504);
#13722=MANIFOLD_SOLID_BREP('refill_cap',#13505);
#13723=MANIFOLD_SOLID_BREP('spring',#13506);
#13724=MANIFOLD_SOLID_BREP('floating_ring_bottom_connector',#13507);
#13725=MANIFOLD_SOLID_BREP(
'binding head screw_ai_CR-BHMS 0.099-48x0.25x0.25-N',#13508);
#13726=MANIFOLD_SOLID_BREP('Floating_ring_guide',#13509);
#13727=MANIFOLD_SOLID_BREP('Bottle_Nech_Seal',#13510);
#13728=MANIFOLD_SOLID_BREP('refill_cap',#13511);
#13729=MANIFOLD_SOLID_BREP('main_housing',#13512);
#13730=MANIFOLD_SOLID_BREP('Nozzle cap',#13513);
#13731=MANIFOLD_SOLID_BREP('dip',#13514);
#13732=MANIFOLD_SOLID_BREP('Neck_flat_seal',#13515);
#13733=MANIFOLD_SOLID_BREP('refill_port',#13516);
#13734=MANIFOLD_SOLID_BREP('ball_outlet_valve',#13517);
#13735=MANIFOLD_SOLID_BREP('Floating_ring',#13518);
#13736=MANIFOLD_SOLID_BREP('ball',#13519);
#13737=MANIFOLD_SOLID_BREP('screw_cover',#13520);
#13738=MANIFOLD_SOLID_BREP('refill+port_air_seal',#13521);
#13739=MANIFOLD_SOLID_BREP('Bottle',#13522);
#13740=MANIFOLD_SOLID_BREP('bottle_premium_cover',#13523);
#13741=MANIFOLD_SOLID_BREP('refill_screw',#13524);
#13742=MANIFOLD_SOLID_BREP('refill_port',#13525);
#13743=MANIFOLD_SOLID_BREP('ball_retainer',#13526);
#13744=MANIFOLD_SOLID_BREP('Bottle_Cap',#13527);
#13745=MANIFOLD_SOLID_BREP('o_ring',#13528);
#13746=SHAPE_DEFINITION_REPRESENTATION(#45523,#13774);
#13747=SHAPE_DEFINITION_REPRESENTATION(#45524,#13775);
#13748=SHAPE_DEFINITION_REPRESENTATION(#45526,#13776);
#13749=SHAPE_DEFINITION_REPRESENTATION(#45528,#13777);
#13750=SHAPE_DEFINITION_REPRESENTATION(#45530,#13778);
#13751=SHAPE_DEFINITION_REPRESENTATION(#45532,#13779);
#13752=SHAPE_DEFINITION_REPRESENTATION(#45534,#13780);
#13753=SHAPE_DEFINITION_REPRESENTATION(#45536,#13781);
#13754=SHAPE_DEFINITION_REPRESENTATION(#45539,#13782);
#13755=SHAPE_DEFINITION_REPRESENTATION(#45542,#13783);
#13756=SHAPE_DEFINITION_REPRESENTATION(#45544,#13784);
#13757=SHAPE_DEFINITION_REPRESENTATION(#45546,#13785);
#13758=SHAPE_DEFINITION_REPRESENTATION(#45548,#13786);
#13759=SHAPE_DEFINITION_REPRESENTATION(#45550,#13787);
#13760=SHAPE_DEFINITION_REPRESENTATION(#45552,#13788);
#13761=SHAPE_DEFINITION_REPRESENTATION(#45555,#13789);
#13762=SHAPE_DEFINITION_REPRESENTATION(#45557,#13790);
#13763=SHAPE_DEFINITION_REPRESENTATION(#45559,#13791);
#13764=SHAPE_DEFINITION_REPRESENTATION(#45561,#13792);
#13765=SHAPE_DEFINITION_REPRESENTATION(#45565,#13793);
#13766=SHAPE_DEFINITION_REPRESENTATION(#45567,#13794);
#13767=SHAPE_DEFINITION_REPRESENTATION(#45569,#13795);
#13768=SHAPE_DEFINITION_REPRESENTATION(#45572,#13796);
#13769=SHAPE_DEFINITION_REPRESENTATION(#45574,#13797);
#13770=SHAPE_DEFINITION_REPRESENTATION(#45577,#13798);
#13771=SHAPE_DEFINITION_REPRESENTATION(#45579,#13799);
#13772=SHAPE_DEFINITION_REPRESENTATION(#45581,#13800);
#13773=SHAPE_DEFINITION_REPRESENTATION(#45583,#13801);
#13774=SHAPE_REPRESENTATION('MAS-690',(#13802,#13903,#13985,#13990,
#14003,#14008,#14225,#14260,#14261,#14275,#14276,#14299,#14334,#14379,#14641,
#14650,#14659,#14660,#14696,#14698,#14760,#14762,#14763,#14764,#14800,#14847,
#14999,#15000,#15048,#15126,#15127,#15189,#15258,#15289,#15294),#45464);
#13775=SHAPE_REPRESENTATION('Top_acces_nozzle_supporter',(#13802),#45465);
#13776=SHAPE_REPRESENTATION('piston',(#13802),#45466);
#13777=SHAPE_REPRESENTATION('75632s_.prt',(#13802),#45467);
#13778=SHAPE_REPRESENTATION('refill_cap',(#13802),#45468);
#13779=SHAPE_REPRESENTATION('spring',(#13802),#45469);
#13780=SHAPE_REPRESENTATION('floating_ring_bottom_connector',(#13802),#45470);
#13781=SHAPE_REPRESENTATION(
'binding head screw_ai_CR-BHMS 0.099-48x0.25x0.25-N',(#13802),#45471);
#13782=SHAPE_REPRESENTATION('Floating_ring_guide',(#13802),#45472);
#13783=SHAPE_REPRESENTATION('Bottle_Nech_Seal',(#13802),#45473);
#13784=SHAPE_REPRESENTATION('refill_cap',(#13802),#45474);
#13785=SHAPE_REPRESENTATION('main_housing',(#13802),#45475);
#13786=SHAPE_REPRESENTATION('Nozzle cap',(#13802),#45476);
#13787=SHAPE_REPRESENTATION('dip',(#13802),#45477);
#13788=SHAPE_REPRESENTATION('Neck_flat_seal',(#13802),#45478);
#13789=SHAPE_REPRESENTATION('refill_port',(#13802),#45479);
#13790=SHAPE_REPRESENTATION('ball_outlet_valve',(#13802),#45480);
#13791=SHAPE_REPRESENTATION('Floating_ring',(#13802),#45481);
#13792=SHAPE_REPRESENTATION('ball',(#13802),#45482);
#13793=SHAPE_REPRESENTATION('screw_cover',(#13802),#45483);
#13794=SHAPE_REPRESENTATION('refill+port_air_seal',(#13802),#45484);
#13795=SHAPE_REPRESENTATION('Bottle',(#13802),#45485);
#13796=SHAPE_REPRESENTATION('bottle_premium_cover',(#13802),#45486);
#13797=SHAPE_REPRESENTATION('refill_screw',(#13802),#45487);
#13798=SHAPE_REPRESENTATION('refill_port',(#13802),#45488);
#13799=SHAPE_REPRESENTATION('ball_retainer',(#13802),#45489);
#13800=SHAPE_REPRESENTATION('Bottle_Cap',(#13802),#45490);
#13801=SHAPE_REPRESENTATION('o_ring',(#13802),#45491);
#13802=AXIS2_PLACEMENT_3D('',#19109,#15295,#15296);
#13803=AXIS2_PLACEMENT_3D('',#19356,#15299,#15300);
#13804=AXIS2_PLACEMENT_3D('',#19418,#15303,#15304);
#13805=AXIS2_PLACEMENT_3D('',#19610,#15308,#15309);
#13806=AXIS2_PLACEMENT_3D('',#19614,#15312,#15313);
#13807=AXIS2_PLACEMENT_3D('',#19615,#15314,#15315);
#13808=AXIS2_PLACEMENT_3D('',#19617,#15316,#15317);
#13809=AXIS2_PLACEMENT_3D('',#19639,#15318,#15319);
#13810=AXIS2_PLACEMENT_3D('',#19645,#15320,#15321);
#13811=AXIS2_PLACEMENT_3D('',#19646,#15322,#15323);
#13812=AXIS2_PLACEMENT_3D('',#19647,#15324,#15325);
#13813=AXIS2_PLACEMENT_3D('',#19648,#15326,#15327);
#13814=AXIS2_PLACEMENT_3D('',#19650,#15328,#15329);
#13815=AXIS2_PLACEMENT_3D('',#19651,#15330,#15331);
#13816=AXIS2_PLACEMENT_3D('',#19653,#15332,#15333);
#13817=AXIS2_PLACEMENT_3D('',#19655,#15334,#15335);
#13818=AXIS2_PLACEMENT_3D('',#19664,#15340,#15341);
#13819=AXIS2_PLACEMENT_3D('',#19673,#15346,#15347);
#13820=AXIS2_PLACEMENT_3D('',#19674,#15348,#15349);
#13821=AXIS2_PLACEMENT_3D('',#19675,#15350,#15351);
#13822=AXIS2_PLACEMENT_3D('',#19676,#15352,#15353);
#13823=AXIS2_PLACEMENT_3D('',#19685,#15358,#15359);
#13824=AXIS2_PLACEMENT_3D('',#19694,#15364,#15365);
#13825=AXIS2_PLACEMENT_3D('',#19695,#15366,#15367);
#13826=AXIS2_PLACEMENT_3D('',#19696,#15368,#15369);
#13827=AXIS2_PLACEMENT_3D('',#19697,#15370,#15371);
#13828=AXIS2_PLACEMENT_3D('',#19706,#15376,#15377);
#13829=AXIS2_PLACEMENT_3D('',#19715,#15382,#15383);
#13830=AXIS2_PLACEMENT_3D('',#19716,#15384,#15385);
#13831=AXIS2_PLACEMENT_3D('',#19717,#15386,#15387);
#13832=AXIS2_PLACEMENT_3D('',#19718,#15388,#15389);
#13833=AXIS2_PLACEMENT_3D('',#19719,#15390,#15391);
#13834=AXIS2_PLACEMENT_3D('',#19721,#15392,#15393);
#13835=AXIS2_PLACEMENT_3D('',#19723,#15394,#15395);
#13836=AXIS2_PLACEMENT_3D('',#19724,#15396,#15397);
#13837=AXIS2_PLACEMENT_3D('',#19726,#15398,#15399);
#13838=AXIS2_PLACEMENT_3D('',#19728,#15400,#15401);
#13839=AXIS2_PLACEMENT_3D('',#19729,#15402,#15403);
#13840=AXIS2_PLACEMENT_3D('',#19731,#15404,#15405);
#13841=AXIS2_PLACEMENT_3D('',#19733,#15406,#15407);
#13842=AXIS2_PLACEMENT_3D('',#19734,#15408,#15409);
#13843=AXIS2_PLACEMENT_3D('',#19736,#15410,#15411);
#13844=AXIS2_PLACEMENT_3D('',#19738,#15412,#15413);
#13845=AXIS2_PLACEMENT_3D('',#19739,#15414,#15415);
#13846=AXIS2_PLACEMENT_3D('',#19741,#15416,#15417);
#13847=AXIS2_PLACEMENT_3D('',#19743,#15418,#15419);
#13848=AXIS2_PLACEMENT_3D('',#19745,#15420,#15421);
#13849=AXIS2_PLACEMENT_3D('',#19747,#15422,#15423);
#13850=AXIS2_PLACEMENT_3D('',#19749,#15424,#15425);
#13851=AXIS2_PLACEMENT_3D('',#19751,#15426,#15427);
#13852=AXIS2_PLACEMENT_3D('',#19753,#15428,#15429);
#13853=AXIS2_PLACEMENT_3D('',#19755,#15430,#15431);
#13854=AXIS2_PLACEMENT_3D('',#19757,#15432,#15433);
#13855=AXIS2_PLACEMENT_3D('',#19758,#15434,#15435);
#13856=AXIS2_PLACEMENT_3D('',#19759,#15436,#15437);
#13857=AXIS2_PLACEMENT_3D('',#19760,#15438,#15439);
#13858=AXIS2_PLACEMENT_3D('',#19762,#15440,#15441);
#13859=AXIS2_PLACEMENT_3D('',#19763,#15442,#15443);
#13860=AXIS2_PLACEMENT_3D('',#19765,#15444,#15445);
#13861=AXIS2_PLACEMENT_3D('',#19767,#15446,#15447);
#13862=AXIS2_PLACEMENT_3D('',#19769,#15448,#15449);
#13863=AXIS2_PLACEMENT_3D('',#19771,#15450,#15451);
#13864=AXIS2_PLACEMENT_3D('',#19773,#15452,#15453);
#13865=AXIS2_PLACEMENT_3D('',#19775,#15454,#15455);
#13866=AXIS2_PLACEMENT_3D('',#19777,#15456,#15457);
#13867=AXIS2_PLACEMENT_3D('',#19779,#15458,#15459);
#13868=AXIS2_PLACEMENT_3D('',#19781,#15460,#15461);
#13869=AXIS2_PLACEMENT_3D('',#19782,#15462,#15463);
#13870=AXIS2_PLACEMENT_3D('',#19783,#15464,#15465);
#13871=AXIS2_PLACEMENT_3D('',#19784,#15466,#15467);
#13872=AXIS2_PLACEMENT_3D('',#19786,#15468,#15469);
#13873=AXIS2_PLACEMENT_3D('',#19787,#15470,#15471);
#13874=AXIS2_PLACEMENT_3D('',#19789,#15472,#15473);
#13875=AXIS2_PLACEMENT_3D('',#19791,#15474,#15475);
#13876=AXIS2_PLACEMENT_3D('',#19792,#15476,#15477);
#13877=AXIS2_PLACEMENT_3D('',#19794,#15478,#15479);
#13878=AXIS2_PLACEMENT_3D('',#19796,#15480,#15481);
#13879=AXIS2_PLACEMENT_3D('',#19797,#15482,#15483);
#13880=AXIS2_PLACEMENT_3D('',#19799,#15484,#15485);
#13881=AXIS2_PLACEMENT_3D('',#19800,#15486,#15487);
#13882=AXIS2_PLACEMENT_3D('',#19801,#15488,#15489);
#13883=AXIS2_PLACEMENT_3D('',#19802,#15490,#15491);
#13884=AXIS2_PLACEMENT_3D('',#19803,#15492,#15493);
#13885=AXIS2_PLACEMENT_3D('',#19804,#15494,#15495);
#13886=AXIS2_PLACEMENT_3D('',#19805,#15496,#15497);
#13887=AXIS2_PLACEMENT_3D('',#19806,#15498,#15499);
#13888=AXIS2_PLACEMENT_3D('',#19807,#15500,#15501);
#13889=AXIS2_PLACEMENT_3D('',#19808,#15502,#15503);
#13890=AXIS2_PLACEMENT_3D('',#19809,#15504,#15505);
#13891=AXIS2_PLACEMENT_3D('',#19810,#15506,#15507);
#13892=AXIS2_PLACEMENT_3D('',#19811,#15508,#15509);
#13893=AXIS2_PLACEMENT_3D('',#19812,#15510,#15511);
#13894=AXIS2_PLACEMENT_3D('',#19813,#15512,#15513);
#13895=AXIS2_PLACEMENT_3D('',#19814,#15514,#15515);
#13896=AXIS2_PLACEMENT_3D('',#19815,#15516,#15517);
#13897=AXIS2_PLACEMENT_3D('',#19816,#15518,#15519);
#13898=AXIS2_PLACEMENT_3D('',#19817,#15520,#15521);
#13899=AXIS2_PLACEMENT_3D('',#19818,#15522,#15523);
#13900=AXIS2_PLACEMENT_3D('',#19819,#15524,#15525);
#13901=AXIS2_PLACEMENT_3D('',#19820,#15526,#15527);
#13902=AXIS2_PLACEMENT_3D('',#19821,#15528,#15529);
#13903=AXIS2_PLACEMENT_3D('',#19838,#15530,#15531);
#13904=AXIS2_PLACEMENT_3D('',#19839,#15532,#15533);
#13905=AXIS2_PLACEMENT_3D('',#19840,#15534,#15535);
#13906=AXIS2_PLACEMENT_3D('',#19842,#15536,#15537);
#13907=AXIS2_PLACEMENT_3D('',#19844,#15538,#15539);
#13908=AXIS2_PLACEMENT_3D('',#19845,#15540,#15541);
#13909=AXIS2_PLACEMENT_3D('',#19847,#15542,#15543);
#13910=AXIS2_PLACEMENT_3D('',#20003,#15547,#15548);
#13911=AXIS2_PLACEMENT_3D('',#20346,#15551,#15552);
#13912=AXIS2_PLACEMENT_3D('',#20349,#15555,#15556);
#13913=AXIS2_PLACEMENT_3D('',#20352,#15558,#15559);
#13914=AXIS2_PLACEMENT_3D('',#20353,#15560,#15561);
#13915=AXIS2_PLACEMENT_3D('',#20355,#15563,#15564);
#13916=AXIS2_PLACEMENT_3D('',#20356,#15565,#15566);
#13917=AXIS2_PLACEMENT_3D('',#20358,#15567,#15568);
#13918=AXIS2_PLACEMENT_3D('',#20360,#15569,#15570);
#13919=AXIS2_PLACEMENT_3D('',#20361,#15571,#15572);
#13920=AXIS2_PLACEMENT_3D('',#20363,#15573,#15574);
#13921=AXIS2_PLACEMENT_3D('',#20365,#15575,#15576);
#13922=AXIS2_PLACEMENT_3D('',#20366,#15577,#15578);
#13923=AXIS2_PLACEMENT_3D('',#20368,#15579,#15580);
#13924=AXIS2_PLACEMENT_3D('',#20370,#15581,#15582);
#13925=AXIS2_PLACEMENT_3D('',#20371,#15583,#15584);
#13926=AXIS2_PLACEMENT_3D('',#20373,#15585,#15586);
#13927=AXIS2_PLACEMENT_3D('',#20375,#15587,#15588);
#13928=AXIS2_PLACEMENT_3D('',#20376,#15589,#15590);
#13929=AXIS2_PLACEMENT_3D('',#20378,#15591,#15592);
#13930=AXIS2_PLACEMENT_3D('',#20380,#15593,#15594);
#13931=AXIS2_PLACEMENT_3D('',#20381,#15595,#15596);
#13932=AXIS2_PLACEMENT_3D('',#20383,#15597,#15598);
#13933=AXIS2_PLACEMENT_3D('',#20385,#15599,#15600);
#13934=AXIS2_PLACEMENT_3D('',#20386,#15601,#15602);
#13935=AXIS2_PLACEMENT_3D('',#20388,#15603,#15604);
#13936=AXIS2_PLACEMENT_3D('',#20390,#15605,#15606);
#13937=AXIS2_PLACEMENT_3D('',#20391,#15607,#15608);
#13938=AXIS2_PLACEMENT_3D('',#20393,#15609,#15610);
#13939=AXIS2_PLACEMENT_3D('',#20395,#15611,#15612);
#13940=AXIS2_PLACEMENT_3D('',#20396,#15613,#15614);
#13941=AXIS2_PLACEMENT_3D('',#20398,#15615,#15616);
#13942=AXIS2_PLACEMENT_3D('',#20400,#15617,#15618);
#13943=AXIS2_PLACEMENT_3D('',#20401,#15619,#15620);
#13944=AXIS2_PLACEMENT_3D('',#20403,#15621,#15622);
#13945=AXIS2_PLACEMENT_3D('',#20404,#15623,#15624);
#13946=AXIS2_PLACEMENT_3D('',#20405,#15625,#15626);
#13947=AXIS2_PLACEMENT_3D('',#20407,#15627,#15628);
#13948=AXIS2_PLACEMENT_3D('',#20408,#15629,#15630);
#13949=AXIS2_PLACEMENT_3D('',#20410,#15631,#15632);
#13950=AXIS2_PLACEMENT_3D('',#20411,#15633,#15634);
#13951=AXIS2_PLACEMENT_3D('',#20413,#15635,#15636);
#13952=AXIS2_PLACEMENT_3D('',#20414,#15637,#15638);
#13953=AXIS2_PLACEMENT_3D('',#20416,#15639,#15640);
#13954=AXIS2_PLACEMENT_3D('',#20417,#15641,#15642);
#13955=AXIS2_PLACEMENT_3D('',#20419,#15643,#15644);
#13956=AXIS2_PLACEMENT_3D('',#20421,#15645,#15646);
#13957=AXIS2_PLACEMENT_3D('',#20422,#15647,#15648);
#13958=AXIS2_PLACEMENT_3D('',#20423,#15649,#15650);
#13959=AXIS2_PLACEMENT_3D('',#20424,#15651,#15652);
#13960=AXIS2_PLACEMENT_3D('',#20426,#15653,#15654);
#13961=AXIS2_PLACEMENT_3D('',#20428,#15655,#15656);
#13962=AXIS2_PLACEMENT_3D('',#20429,#15657,#15658);
#13963=AXIS2_PLACEMENT_3D('',#20430,#15659,#15660);
#13964=AXIS2_PLACEMENT_3D('',#20432,#15661,#15662);
#13965=AXIS2_PLACEMENT_3D('',#20433,#15663,#15664);
#13966=AXIS2_PLACEMENT_3D('',#20435,#15665,#15666);
#13967=AXIS2_PLACEMENT_3D('',#20437,#15667,#15668);
#13968=AXIS2_PLACEMENT_3D('',#20438,#15669,#15670);
#13969=AXIS2_PLACEMENT_3D('',#20440,#15671,#15672);
#13970=AXIS2_PLACEMENT_3D('',#20441,#15673,#15674);
#13971=AXIS2_PLACEMENT_3D('',#20442,#15675,#15676);
#13972=AXIS2_PLACEMENT_3D('',#20443,#15677,#15678);
#13973=AXIS2_PLACEMENT_3D('',#20444,#15679,#15680);
#13974=AXIS2_PLACEMENT_3D('',#20445,#15681,#15682);
#13975=AXIS2_PLACEMENT_3D('',#20446,#15683,#15684);
#13976=AXIS2_PLACEMENT_3D('',#20447,#15685,#15686);
#13977=AXIS2_PLACEMENT_3D('',#20448,#15687,#15688);
#13978=AXIS2_PLACEMENT_3D('',#20449,#15689,#15690);
#13979=AXIS2_PLACEMENT_3D('',#20450,#15691,#15692);
#13980=AXIS2_PLACEMENT_3D('',#20451,#15693,#15694);
#13981=AXIS2_PLACEMENT_3D('',#20452,#15695,#15696);
#13982=AXIS2_PLACEMENT_3D('',#20454,#15697,#15698);
#13983=AXIS2_PLACEMENT_3D('',#20456,#15699,#15700);
#13984=AXIS2_PLACEMENT_3D('',#20457,#15701,#15702);
#13985=AXIS2_PLACEMENT_3D('',#20458,#15703,#15704);
#13986=AXIS2_PLACEMENT_3D('',#20459,#15705,#15706);
#13987=AXIS2_PLACEMENT_3D('',#20563,#15708,#15709);
#13988=AXIS2_PLACEMENT_3D('',#20571,#15710,#15711);
#13989=AXIS2_PLACEMENT_3D('',#21572,#15713,#15714);
#13990=AXIS2_PLACEMENT_3D('',#27050,#15715,#15716);
#13991=AXIS2_PLACEMENT_3D('',#27333,#15717,#15718);
#13992=AXIS2_PLACEMENT_3D('',#27721,#15720,#15721);
#13993=AXIS2_PLACEMENT_3D('',#27722,#15722,#15723);
#13994=AXIS2_PLACEMENT_3D('',#27774,#15724,#15725);
#13995=AXIS2_PLACEMENT_3D('',#28049,#15727,#15728);
#13996=AXIS2_PLACEMENT_3D('',#28498,#15730,#15731);
#13997=AXIS2_PLACEMENT_3D('',#28555,#15732,#15733);
#13998=AXIS2_PLACEMENT_3D('',#28557,#15735,#15736);
#13999=AXIS2_PLACEMENT_3D('',#28558,#15737,#15738);
#14000=AXIS2_PLACEMENT_3D('',#28559,#15739,#15740);
#14001=AXIS2_PLACEMENT_3D('',#28560,#15741,#15742);
#14002=AXIS2_PLACEMENT_3D('',#28562,#15743,#15744);
#14003=AXIS2_PLACEMENT_3D('',#28563,#15745,#15746);
#14004=AXIS2_PLACEMENT_3D('',#28564,#15747,#15748);
#14005=AXIS2_PLACEMENT_3D('',#28565,#15749,#15750);
#14006=AXIS2_PLACEMENT_3D('',#28567,#15751,#15752);
#14007=AXIS2_PLACEMENT_3D('',#28568,#15753,#15754);
#14008=AXIS2_PLACEMENT_3D('',#30740,#15755,#15756);
#14009=AXIS2_PLACEMENT_3D('',#30741,#15757,#15758);
#14010=AXIS2_PLACEMENT_3D('',#30742,#15759,#15760);
#14011=AXIS2_PLACEMENT_3D('',#30754,#15763,#15764);
#14012=AXIS2_PLACEMENT_3D('',#30755,#15765,#15766);
#14013=AXIS2_PLACEMENT_3D('',#30758,#15767,#15768);
#14014=AXIS2_PLACEMENT_3D('',#30759,#15769,#15770);
#14015=AXIS2_PLACEMENT_3D('',#30760,#15771,#15772);
#14016=AXIS2_PLACEMENT_3D('',#30761,#15773,#15774);
#14017=AXIS2_PLACEMENT_3D('',#30764,#15775,#15776);
#14018=AXIS2_PLACEMENT_3D('',#30765,#15777,#15778);
#14019=AXIS2_PLACEMENT_3D('',#30766,#15779,#15780);
#14020=AXIS2_PLACEMENT_3D('',#30767,#15781,#15782);
#14021=AXIS2_PLACEMENT_3D('',#30770,#15783,#15784);
#14022=AXIS2_PLACEMENT_3D('',#30771,#15785,#15786);
#14023=AXIS2_PLACEMENT_3D('',#30772,#15787,#15788);
#14024=AXIS2_PLACEMENT_3D('',#30773,#15789,#15790);
#14025=AXIS2_PLACEMENT_3D('',#30778,#15793,#15794);
#14026=AXIS2_PLACEMENT_3D('',#30779,#15795,#15796);
#14027=AXIS2_PLACEMENT_3D('',#30784,#15799,#15800);
#14028=AXIS2_PLACEMENT_3D('',#30785,#15801,#15802);
#14029=AXIS2_PLACEMENT_3D('',#30790,#15805,#15806);
#14030=AXIS2_PLACEMENT_3D('',#30791,#15807,#15808);
#14031=AXIS2_PLACEMENT_3D('',#30794,#15809,#15810);
#14032=AXIS2_PLACEMENT_3D('',#30795,#15811,#15812);
#14033=AXIS2_PLACEMENT_3D('',#30796,#15813,#15814);
#14034=AXIS2_PLACEMENT_3D('',#30797,#15815,#15816);
#14035=AXIS2_PLACEMENT_3D('',#30800,#15817,#15818);
#14036=AXIS2_PLACEMENT_3D('',#30802,#15819,#15820);
#14037=AXIS2_PLACEMENT_3D('',#30804,#15821,#15822);
#14038=AXIS2_PLACEMENT_3D('',#30805,#15823,#15824);
#14039=AXIS2_PLACEMENT_3D('',#30806,#15825,#15826);
#14040=AXIS2_PLACEMENT_3D('',#30809,#15827,#15828);
#14041=AXIS2_PLACEMENT_3D('',#30810,#15829,#15830);
#14042=AXIS2_PLACEMENT_3D('',#30811,#15831,#15832);
#14043=AXIS2_PLACEMENT_3D('',#30812,#15833,#15834);
#14044=AXIS2_PLACEMENT_3D('',#30815,#15835,#15836);
#14045=AXIS2_PLACEMENT_3D('',#30816,#15837,#15838);
#14046=AXIS2_PLACEMENT_3D('',#30817,#15839,#15840);
#14047=AXIS2_PLACEMENT_3D('',#30827,#15843,#15844);
#14048=AXIS2_PLACEMENT_3D('',#30828,#15845,#15846);
#14049=AXIS2_PLACEMENT_3D('',#30833,#15849,#15850);
#14050=AXIS2_PLACEMENT_3D('',#30834,#15851,#15852);
#14051=AXIS2_PLACEMENT_3D('',#30839,#15855,#15856);
#14052=AXIS2_PLACEMENT_3D('',#30840,#15857,#15858);
#14053=AXIS2_PLACEMENT_3D('',#30843,#15859,#15860);
#14054=AXIS2_PLACEMENT_3D('',#30844,#15861,#15862);
#14055=AXIS2_PLACEMENT_3D('',#30845,#15863,#15864);
#14056=AXIS2_PLACEMENT_3D('',#30846,#15865,#15866);
#14057=AXIS2_PLACEMENT_3D('',#30851,#15869,#15870);
#14058=AXIS2_PLACEMENT_3D('',#30852,#15871,#15872);
#14059=AXIS2_PLACEMENT_3D('',#30856,#15875,#15876);
#14060=AXIS2_PLACEMENT_3D('',#30857,#15877,#15878);
#14061=AXIS2_PLACEMENT_3D('',#30858,#15879,#15880);
#14062=AXIS2_PLACEMENT_3D('',#30859,#15881,#15882);
#14063=AXIS2_PLACEMENT_3D('',#30860,#15883,#15884);
#14064=AXIS2_PLACEMENT_3D('',#30863,#15885,#15886);
#14065=AXIS2_PLACEMENT_3D('',#30864,#15887,#15888);
#14066=AXIS2_PLACEMENT_3D('',#30865,#15889,#15890);
#14067=AXIS2_PLACEMENT_3D('',#30866,#15891,#15892);
#14068=AXIS2_PLACEMENT_3D('',#30869,#15893,#15894);
#14069=AXIS2_PLACEMENT_3D('',#30870,#15895,#15896);
#14070=AXIS2_PLACEMENT_3D('',#30871,#15897,#15898);
#14071=AXIS2_PLACEMENT_3D('',#30872,#15899,#15900);
#14072=AXIS2_PLACEMENT_3D('',#30875,#15901,#15902);
#14073=AXIS2_PLACEMENT_3D('',#30876,#15903,#15904);
#14074=AXIS2_PLACEMENT_3D('',#30877,#15905,#15906);
#14075=AXIS2_PLACEMENT_3D('',#30878,#15907,#15908);
#14076=AXIS2_PLACEMENT_3D('',#30880,#15909,#15910);
#14077=AXIS2_PLACEMENT_3D('',#30881,#15911,#15912);
#14078=AXIS2_PLACEMENT_3D('',#30882,#15913,#15914);
#14079=AXIS2_PLACEMENT_3D('',#30887,#15917,#15918);
#14080=AXIS2_PLACEMENT_3D('',#30888,#15919,#15920);
#14081=AXIS2_PLACEMENT_3D('',#30892,#15923,#15924);
#14082=AXIS2_PLACEMENT_3D('',#30893,#15925,#15926);
#14083=AXIS2_PLACEMENT_3D('',#30896,#15927,#15928);
#14084=AXIS2_PLACEMENT_3D('',#30897,#15929,#15930);
#14085=AXIS2_PLACEMENT_3D('',#30898,#15931,#15932);
#14086=AXIS2_PLACEMENT_3D('',#30899,#15933,#15934);
#14087=AXIS2_PLACEMENT_3D('',#30904,#15937,#15938);
#14088=AXIS2_PLACEMENT_3D('',#30905,#15939,#15940);
#14089=AXIS2_PLACEMENT_3D('',#30910,#15943,#15944);
#14090=AXIS2_PLACEMENT_3D('',#30911,#15945,#15946);
#14091=AXIS2_PLACEMENT_3D('',#30913,#15947,#15948);
#14092=AXIS2_PLACEMENT_3D('',#30914,#15949,#15950);
#14093=AXIS2_PLACEMENT_3D('',#30915,#15951,#15952);
#14094=AXIS2_PLACEMENT_3D('',#30916,#15953,#15954);
#14095=AXIS2_PLACEMENT_3D('',#30918,#15955,#15956);
#14096=AXIS2_PLACEMENT_3D('',#30919,#15957,#15958);
#14097=AXIS2_PLACEMENT_3D('',#30920,#15959,#15960);
#14098=AXIS2_PLACEMENT_3D('',#30923,#15961,#15962);
#14099=AXIS2_PLACEMENT_3D('',#30924,#15963,#15964);
#14100=AXIS2_PLACEMENT_3D('',#30925,#15965,#15966);
#14101=AXIS2_PLACEMENT_3D('',#30926,#15967,#15968);
#14102=AXIS2_PLACEMENT_3D('',#30929,#15969,#15970);
#14103=AXIS2_PLACEMENT_3D('',#30930,#15971,#15972);
#14104=AXIS2_PLACEMENT_3D('',#30931,#15973,#15974);
#14105=AXIS2_PLACEMENT_3D('',#30932,#15975,#15976);
#14106=AXIS2_PLACEMENT_3D('',#30934,#15977,#15978);
#14107=AXIS2_PLACEMENT_3D('',#30935,#15979,#15980);
#14108=AXIS2_PLACEMENT_3D('',#30936,#15981,#15982);
#14109=AXIS2_PLACEMENT_3D('',#30939,#15983,#15984);
#14110=AXIS2_PLACEMENT_3D('',#30940,#15985,#15986);
#14111=AXIS2_PLACEMENT_3D('',#30941,#15987,#15988);
#14112=AXIS2_PLACEMENT_3D('',#30942,#15989,#15990);
#14113=AXIS2_PLACEMENT_3D('',#30946,#15993,#15994);
#14114=AXIS2_PLACEMENT_3D('',#30947,#15995,#15996);
#14115=AXIS2_PLACEMENT_3D('',#30952,#15999,#16000);
#14116=AXIS2_PLACEMENT_3D('',#30953,#16001,#16002);
#14117=AXIS2_PLACEMENT_3D('',#30956,#16003,#16004);
#14118=AXIS2_PLACEMENT_3D('',#30957,#16005,#16006);
#14119=AXIS2_PLACEMENT_3D('',#30958,#16007,#16008);
#14120=AXIS2_PLACEMENT_3D('',#30959,#16009,#16010);
#14121=AXIS2_PLACEMENT_3D('',#30964,#16013,#16014);
#14122=AXIS2_PLACEMENT_3D('',#30965,#16015,#16016);
#14123=AXIS2_PLACEMENT_3D('',#30969,#16019,#16020);
#14124=AXIS2_PLACEMENT_3D('',#30970,#16021,#16022);
#14125=AXIS2_PLACEMENT_3D('',#30972,#16023,#16024);
#14126=AXIS2_PLACEMENT_3D('',#30973,#16025,#16026);
#14127=AXIS2_PLACEMENT_3D('',#30974,#16027,#16028);
#14128=AXIS2_PLACEMENT_3D('',#30977,#16029,#16030);
#14129=AXIS2_PLACEMENT_3D('',#30978,#16031,#16032);
#14130=AXIS2_PLACEMENT_3D('',#30979,#16033,#16034);
#14131=AXIS2_PLACEMENT_3D('',#30980,#16035,#16036);
#14132=AXIS2_PLACEMENT_3D('',#30983,#16037,#16038);
#14133=AXIS2_PLACEMENT_3D('',#30984,#16039,#16040);
#14134=AXIS2_PLACEMENT_3D('',#30985,#16041,#16042);
#14135=AXIS2_PLACEMENT_3D('',#30986,#16043,#16044);
#14136=AXIS2_PLACEMENT_3D('',#30988,#16045,#16046);
#14137=AXIS2_PLACEMENT_3D('',#30989,#16047,#16048);
#14138=AXIS2_PLACEMENT_3D('',#30990,#16049,#16050);
#14139=AXIS2_PLACEMENT_3D('',#30995,#16053,#16054);
#14140=AXIS2_PLACEMENT_3D('',#30996,#16055,#16056);
#14141=AXIS2_PLACEMENT_3D('',#31000,#16059,#16060);
#14142=AXIS2_PLACEMENT_3D('',#31001,#16061,#16062);
#14143=AXIS2_PLACEMENT_3D('',#31004,#16063,#16064);
#14144=AXIS2_PLACEMENT_3D('',#31005,#16065,#16066);
#14145=AXIS2_PLACEMENT_3D('',#31006,#16067,#16068);
#14146=AXIS2_PLACEMENT_3D('',#31007,#16069,#16070);
#14147=AXIS2_PLACEMENT_3D('',#31012,#16073,#16074);
#14148=AXIS2_PLACEMENT_3D('',#31013,#16075,#16076);
#14149=AXIS2_PLACEMENT_3D('',#31018,#16079,#16080);
#14150=AXIS2_PLACEMENT_3D('',#31019,#16081,#16082);
#14151=AXIS2_PLACEMENT_3D('',#31021,#16083,#16084);
#14152=AXIS2_PLACEMENT_3D('',#31022,#16085,#16086);
#14153=AXIS2_PLACEMENT_3D('',#31023,#16087,#16088);
#14154=AXIS2_PLACEMENT_3D('',#31024,#16089,#16090);
#14155=AXIS2_PLACEMENT_3D('',#31026,#16091,#16092);
#14156=AXIS2_PLACEMENT_3D('',#31027,#16093,#16094);
#14157=AXIS2_PLACEMENT_3D('',#31028,#16095,#16096);
#14158=AXIS2_PLACEMENT_3D('',#31029,#16097,#16098);
#14159=AXIS2_PLACEMENT_3D('',#31030,#16099,#16100);
#14160=AXIS2_PLACEMENT_3D('',#31031,#16101,#16102);
#14161=AXIS2_PLACEMENT_3D('',#31033,#16103,#16104);
#14162=AXIS2_PLACEMENT_3D('',#31034,#16105,#16106);
#14163=AXIS2_PLACEMENT_3D('',#31035,#16107,#16108);
#14164=AXIS2_PLACEMENT_3D('',#31038,#16109,#16110);
#14165=AXIS2_PLACEMENT_3D('',#31039,#16111,#16112);
#14166=AXIS2_PLACEMENT_3D('',#31040,#16113,#16114);
#14167=AXIS2_PLACEMENT_3D('',#31041,#16115,#16116);
#14168=AXIS2_PLACEMENT_3D('',#31045,#16119,#16120);
#14169=AXIS2_PLACEMENT_3D('',#31046,#16121,#16122);
#14170=AXIS2_PLACEMENT_3D('',#31050,#16125,#16126);
#14171=AXIS2_PLACEMENT_3D('',#31051,#16127,#16128);
#14172=AXIS2_PLACEMENT_3D('',#31052,#16129,#16130);
#14173=AXIS2_PLACEMENT_3D('',#31053,#16131,#16132);
#14174=AXIS2_PLACEMENT_3D('',#31055,#16133,#16134);
#14175=AXIS2_PLACEMENT_3D('',#31057,#16135,#16136);
#14176=AXIS2_PLACEMENT_3D('',#31058,#16137,#16138);
#14177=AXIS2_PLACEMENT_3D('',#31060,#16139,#16140);
#14178=AXIS2_PLACEMENT_3D('',#31062,#16141,#16142);
#14179=AXIS2_PLACEMENT_3D('',#31063,#16143,#16144);
#14180=AXIS2_PLACEMENT_3D('',#31065,#16145,#16146);
#14181=AXIS2_PLACEMENT_3D('',#31533,#16151,#16152);
#14182=AXIS2_PLACEMENT_3D('',#31536,#16155,#16156);
#14183=AXIS2_PLACEMENT_3D('',#31538,#16158,#16159);
#14184=AXIS2_PLACEMENT_3D('',#31540,#16161,#16162);
#14185=AXIS2_PLACEMENT_3D('',#31541,#16163,#16164);
#14186=AXIS2_PLACEMENT_3D('',#31543,#16165,#16166);
#14187=AXIS2_PLACEMENT_3D('',#31545,#16167,#16168);
#14188=AXIS2_PLACEMENT_3D('',#31546,#16169,#16170);
#14189=AXIS2_PLACEMENT_3D('',#31548,#16171,#16172);
#14190=AXIS2_PLACEMENT_3D('',#31550,#16173,#16174);
#14191=AXIS2_PLACEMENT_3D('',#31552,#16175,#16176);
#14192=AXIS2_PLACEMENT_3D('',#31553,#16177,#16178);
#14193=AXIS2_PLACEMENT_3D('',#31555,#16179,#16180);
#14194=AXIS2_PLACEMENT_3D('',#31556,#16181,#16182);
#14195=AXIS2_PLACEMENT_3D('',#31557,#16183,#16184);
#14196=AXIS2_PLACEMENT_3D('',#31558,#16185,#16186);
#14197=AXIS2_PLACEMENT_3D('',#31559,#16187,#16188);
#14198=AXIS2_PLACEMENT_3D('',#31560,#16189,#16190);
#14199=AXIS2_PLACEMENT_3D('',#31562,#16192,#16193);
#14200=AXIS2_PLACEMENT_3D('',#31563,#16194,#16195);
#14201=AXIS2_PLACEMENT_3D('',#31564,#16196,#16197);
#14202=AXIS2_PLACEMENT_3D('',#31565,#16198,#16199);
#14203=AXIS2_PLACEMENT_3D('',#31566,#16200,#16201);
#14204=AXIS2_PLACEMENT_3D('',#31567,#16202,#16203);
#14205=AXIS2_PLACEMENT_3D('',#31568,#16204,#16205);
#14206=AXIS2_PLACEMENT_3D('',#31569,#16206,#16207);
#14207=AXIS2_PLACEMENT_3D('',#31570,#16208,#16209);
#14208=AXIS2_PLACEMENT_3D('',#31571,#16210,#16211);
#14209=AXIS2_PLACEMENT_3D('',#31573,#16212,#16213);
#14210=AXIS2_PLACEMENT_3D('',#31575,#16214,#16215);
#14211=AXIS2_PLACEMENT_3D('',#31577,#16216,#16217);
#14212=AXIS2_PLACEMENT_3D('',#31578,#16218,#16219);
#14213=AXIS2_PLACEMENT_3D('',#31579,#16220,#16221);
#14214=AXIS2_PLACEMENT_3D('',#31580,#16222,#16223);
#14215=AXIS2_PLACEMENT_3D('',#31581,#16224,#16225);
#14216=AXIS2_PLACEMENT_3D('',#31582,#16226,#16227);
#14217=AXIS2_PLACEMENT_3D('',#31583,#16228,#16229);
#14218=AXIS2_PLACEMENT_3D('',#31584,#16230,#16231);
#14219=AXIS2_PLACEMENT_3D('',#31585,#16232,#16233);
#14220=AXIS2_PLACEMENT_3D('',#31586,#16234,#16235);
#14221=AXIS2_PLACEMENT_3D('',#31587,#16236,#16237);
#14222=AXIS2_PLACEMENT_3D('',#31588,#16238,#16239);
#14223=AXIS2_PLACEMENT_3D('',#31589,#16240,#16241);
#14224=AXIS2_PLACEMENT_3D('',#31591,#16242,#16243);
#14225=AXIS2_PLACEMENT_3D('',#31592,#16244,#16245);
#14226=AXIS2_PLACEMENT_3D('',#31593,#16246,#16247);
#14227=AXIS2_PLACEMENT_3D('',#31594,#16248,#16249);
#14228=AXIS2_PLACEMENT_3D('',#31602,#16253,#16254);
#14229=AXIS2_PLACEMENT_3D('',#31605,#16256,#16257);
#14230=AXIS2_PLACEMENT_3D('',#31606,#16258,#16259);
#14231=AXIS2_PLACEMENT_3D('',#31609,#16261,#16262);
#14232=AXIS2_PLACEMENT_3D('',#31610,#16263,#16264);
#14233=AXIS2_PLACEMENT_3D('',#31611,#16265,#16266);
#14234=AXIS2_PLACEMENT_3D('',#31619,#16270,#16271);
#14235=AXIS2_PLACEMENT_3D('',#31622,#16273,#16274);
#14236=AXIS2_PLACEMENT_3D('',#31623,#16275,#16276);
#14237=AXIS2_PLACEMENT_3D('',#31626,#16278,#16279);
#14238=AXIS2_PLACEMENT_3D('',#31627,#16280,#16281);
#14239=AXIS2_PLACEMENT_3D('',#31630,#16283,#16284);
#14240=AXIS2_PLACEMENT_3D('',#31634,#16287,#16288);
#14241=AXIS2_PLACEMENT_3D('',#31635,#16289,#16290);
#14242=AXIS2_PLACEMENT_3D('',#31641,#16294,#16295);
#14243=AXIS2_PLACEMENT_3D('',#31642,#16296,#16297);
#14244=AXIS2_PLACEMENT_3D('',#31643,#16298,#16299);
#14245=AXIS2_PLACEMENT_3D('',#31645,#16300,#16301);
#14246=AXIS2_PLACEMENT_3D('',#31647,#16302,#16303);
#14247=AXIS2_PLACEMENT_3D('',#31648,#16304,#16305);
#14248=AXIS2_PLACEMENT_3D('',#31650,#16306,#16307);
#14249=AXIS2_PLACEMENT_3D('',#31651,#16308,#16309);
#14250=AXIS2_PLACEMENT_3D('',#31652,#16310,#16311);
#14251=AXIS2_PLACEMENT_3D('',#31653,#16312,#16313);
#14252=AXIS2_PLACEMENT_3D('',#31654,#16314,#16315);
#14253=AXIS2_PLACEMENT_3D('',#31655,#16316,#16317);
#14254=AXIS2_PLACEMENT_3D('',#31656,#16318,#16319);
#14255=AXIS2_PLACEMENT_3D('',#31657,#16320,#16321);
#14256=AXIS2_PLACEMENT_3D('',#31658,#16322,#16323);
#14257=AXIS2_PLACEMENT_3D('',#31659,#16324,#16325);
#14258=AXIS2_PLACEMENT_3D('',#31661,#16326,#16327);
#14259=AXIS2_PLACEMENT_3D('',#31662,#16328,#16329);
#14260=AXIS2_PLACEMENT_3D('',#31663,#16330,#16331);
#14261=AXIS2_PLACEMENT_3D('',#31664,#16332,#16333);
#14262=AXIS2_PLACEMENT_3D('',#31665,#16334,#16335);
#14263=AXIS2_PLACEMENT_3D('',#31666,#16336,#16337);
#14264=AXIS2_PLACEMENT_3D('',#31668,#16338,#16339);
#14265=AXIS2_PLACEMENT_3D('',#31670,#16340,#16341);
#14266=AXIS2_PLACEMENT_3D('',#31671,#16342,#16343);
#14267=AXIS2_PLACEMENT_3D('',#31673,#16344,#16345);
#14268=AXIS2_PLACEMENT_3D('',#31675,#16346,#16347);
#14269=AXIS2_PLACEMENT_3D('',#31676,#16348,#16349);
#14270=AXIS2_PLACEMENT_3D('',#31677,#16350,#16351);
#14271=AXIS2_PLACEMENT_3D('',#31679,#16352,#16353);
#14272=AXIS2_PLACEMENT_3D('',#31681,#16354,#16355);
#14273=AXIS2_PLACEMENT_3D('',#31682,#16356,#16357);
#14274=AXIS2_PLACEMENT_3D('',#31685,#16358,#16359);
#14275=AXIS2_PLACEMENT_3D('',#31686,#16360,#16361);
#14276=AXIS2_PLACEMENT_3D('',#31687,#16362,#16363);
#14277=AXIS2_PLACEMENT_3D('',#31688,#16364,#16365);
#14278=AXIS2_PLACEMENT_3D('',#31689,#16366,#16367);
#14279=AXIS2_PLACEMENT_3D('',#31691,#16368,#16369);
#14280=AXIS2_PLACEMENT_3D('',#31693,#16370,#16371);
#14281=AXIS2_PLACEMENT_3D('',#31694,#16372,#16373);
#14282=AXIS2_PLACEMENT_3D('',#31696,#16374,#16375);
#14283=AXIS2_PLACEMENT_3D('',#31698,#16376,#16377);
#14284=AXIS2_PLACEMENT_3D('',#31699,#16378,#16379);
#14285=AXIS2_PLACEMENT_3D('',#31701,#16380,#16381);
#14286=AXIS2_PLACEMENT_3D('',#31703,#16382,#16383);
#14287=AXIS2_PLACEMENT_3D('',#31704,#16384,#16385);
#14288=AXIS2_PLACEMENT_3D('',#31706,#16386,#16387);
#14289=AXIS2_PLACEMENT_3D('',#31708,#16388,#16389);
#14290=AXIS2_PLACEMENT_3D('',#31709,#16390,#16391);
#14291=AXIS2_PLACEMENT_3D('',#31711,#16392,#16393);
#14292=AXIS2_PLACEMENT_3D('',#31713,#16394,#16395);
#14293=AXIS2_PLACEMENT_3D('',#31714,#16396,#16397);
#14294=AXIS2_PLACEMENT_3D('',#31716,#16398,#16399);
#14295=AXIS2_PLACEMENT_3D('',#31717,#16400,#16401);
#14296=AXIS2_PLACEMENT_3D('',#31718,#16402,#16403);
#14297=AXIS2_PLACEMENT_3D('',#31719,#16404,#16405);
#14298=AXIS2_PLACEMENT_3D('',#31720,#16406,#16407);
#14299=AXIS2_PLACEMENT_3D('',#31721,#16408,#16409);
#14300=AXIS2_PLACEMENT_3D('',#31966,#16410,#16411);
#14301=AXIS2_PLACEMENT_3D('',#32031,#16412,#16413);
#14302=AXIS2_PLACEMENT_3D('',#32590,#16416,#16417);
#14303=AXIS2_PLACEMENT_3D('',#32591,#16418,#16419);
#14304=AXIS2_PLACEMENT_3D('',#32647,#16420,#16421);
#14305=AXIS2_PLACEMENT_3D('',#32649,#16423,#16424);
#14306=AXIS2_PLACEMENT_3D('',#32650,#16425,#16426);
#14307=AXIS2_PLACEMENT_3D('',#32655,#16428,#16429);
#14308=AXIS2_PLACEMENT_3D('',#32657,#16431,#16432);
#14309=AXIS2_PLACEMENT_3D('',#32661,#16434,#16435);
#14310=AXIS2_PLACEMENT_3D('',#32671,#16436,#16437);
#14311=AXIS2_PLACEMENT_3D('',#33353,#16438,#16439);
#14312=AXIS2_PLACEMENT_3D('',#33356,#16442,#16443);
#14313=AXIS2_PLACEMENT_3D('',#33369,#16447,#16448);
#14314=AXIS2_PLACEMENT_3D('',#33444,#16449,#16450);
#14315=AXIS2_PLACEMENT_3D('',#33470,#16451,#16452);
#14316=AXIS2_PLACEMENT_3D('',#33471,#16453,#16454);
#14317=AXIS2_PLACEMENT_3D('',#33472,#16455,#16456);
#14318=AXIS2_PLACEMENT_3D('',#33473,#16457,#16458);
#14319=AXIS2_PLACEMENT_3D('',#33474,#16459,#16460);
#14320=AXIS2_PLACEMENT_3D('',#33476,#16461,#16462);
#14321=AXIS2_PLACEMENT_3D('',#33477,#16463,#16464);
#14322=AXIS2_PLACEMENT_3D('',#33479,#16465,#16466);
#14323=AXIS2_PLACEMENT_3D('',#33480,#16467,#16468);
#14324=AXIS2_PLACEMENT_3D('',#33481,#16469,#16470);
#14325=AXIS2_PLACEMENT_3D('',#33483,#16471,#16472);
#14326=AXIS2_PLACEMENT_3D('',#33484,#16473,#16474);
#14327=AXIS2_PLACEMENT_3D('',#33486,#16475,#16476);
#14328=AXIS2_PLACEMENT_3D('',#33487,#16477,#16478);
#14329=AXIS2_PLACEMENT_3D('',#33489,#16479,#16480);
#14330=AXIS2_PLACEMENT_3D('',#33491,#16481,#16482);
#14331=AXIS2_PLACEMENT_3D('',#33492,#16483,#16484);
#14332=AXIS2_PLACEMENT_3D('',#33493,#16485,#16486);
#14333=AXIS2_PLACEMENT_3D('',#33494,#16487,#16488);
#14334=AXIS2_PLACEMENT_3D('',#33495,#16489,#16490);
#14335=AXIS2_PLACEMENT_3D('',#33496,#16491,#16492);
#14336=AXIS2_PLACEMENT_3D('',#33497,#16493,#16494);
#14337=AXIS2_PLACEMENT_3D('',#33499,#16495,#16496);
#14338=AXIS2_PLACEMENT_3D('',#33501,#16497,#16498);
#14339=AXIS2_PLACEMENT_3D('',#33502,#16499,#16500);
#14340=AXIS2_PLACEMENT_3D('',#33504,#16501,#16502);
#14341=AXIS2_PLACEMENT_3D('',#33506,#16503,#16504);
#14342=AXIS2_PLACEMENT_3D('',#33507,#16505,#16506);
#14343=AXIS2_PLACEMENT_3D('',#33509,#16507,#16508);
#14344=AXIS2_PLACEMENT_3D('',#33511,#16509,#16510);
#14345=AXIS2_PLACEMENT_3D('',#33512,#16511,#16512);
#14346=AXIS2_PLACEMENT_3D('',#33514,#16513,#16514);
#14347=AXIS2_PLACEMENT_3D('',#33516,#16515,#16516);
#14348=AXIS2_PLACEMENT_3D('',#33517,#16517,#16518);
#14349=AXIS2_PLACEMENT_3D('',#33519,#16519,#16520);
#14350=AXIS2_PLACEMENT_3D('',#33521,#16521,#16522);
#14351=AXIS2_PLACEMENT_3D('',#33522,#16523,#16524);
#14352=AXIS2_PLACEMENT_3D('',#33524,#16525,#16526);
#14353=AXIS2_PLACEMENT_3D('',#33525,#16527,#16528);
#14354=AXIS2_PLACEMENT_3D('',#33527,#16529,#16530);
#14355=AXIS2_PLACEMENT_3D('',#33528,#16531,#16532);
#14356=AXIS2_PLACEMENT_3D('',#33530,#16533,#16534);
#14357=AXIS2_PLACEMENT_3D('',#33531,#16535,#16536);
#14358=AXIS2_PLACEMENT_3D('',#33533,#16537,#16538);
#14359=AXIS2_PLACEMENT_3D('',#33534,#16539,#16540);
#14360=AXIS2_PLACEMENT_3D('',#33536,#16541,#16542);
#14361=AXIS2_PLACEMENT_3D('',#33537,#16543,#16544);
#14362=AXIS2_PLACEMENT_3D('',#33538,#16545,#16546);
#14363=AXIS2_PLACEMENT_3D('',#33540,#16547,#16548);
#14364=AXIS2_PLACEMENT_3D('',#33541,#16549,#16550);
#14365=AXIS2_PLACEMENT_3D('',#33543,#16551,#16552);
#14366=AXIS2_PLACEMENT_3D('',#33545,#16553,#16554);
#14367=AXIS2_PLACEMENT_3D('',#33546,#16555,#16556);
#14368=AXIS2_PLACEMENT_3D('',#33548,#16557,#16558);
#14369=AXIS2_PLACEMENT_3D('',#33550,#16559,#16560);
#14370=AXIS2_PLACEMENT_3D('',#33551,#16561,#16562);
#14371=AXIS2_PLACEMENT_3D('',#33553,#16563,#16564);
#14372=AXIS2_PLACEMENT_3D('',#33554,#16565,#16566);
#14373=AXIS2_PLACEMENT_3D('',#33556,#16567,#16568);
#14374=AXIS2_PLACEMENT_3D('',#33557,#16569,#16570);
#14375=AXIS2_PLACEMENT_3D('',#33558,#16571,#16572);
#14376=AXIS2_PLACEMENT_3D('',#33559,#16573,#16574);
#14377=AXIS2_PLACEMENT_3D('',#33560,#16575,#16576);
#14378=AXIS2_PLACEMENT_3D('',#33561,#16577,#16578);
#14379=AXIS2_PLACEMENT_3D('',#33562,#16579,#16580);
#14380=AXIS2_PLACEMENT_3D('',#33563,#16581,#16582);
#14381=AXIS2_PLACEMENT_3D('',#33564,#16583,#16584);
#14382=AXIS2_PLACEMENT_3D('',#33566,#16585,#16586);
#14383=AXIS2_PLACEMENT_3D('',#34064,#16591,#16592);
#14384=AXIS2_PLACEMENT_3D('',#34067,#16595,#16596);
#14385=AXIS2_PLACEMENT_3D('',#34071,#16599,#16600);
#14386=AXIS2_PLACEMENT_3D('',#34073,#16602,#16603);
#14387=AXIS2_PLACEMENT_3D('',#34074,#16604,#16605);
#14388=AXIS2_PLACEMENT_3D('',#34075,#16606,#16607);
#14389=AXIS2_PLACEMENT_3D('',#34077,#16608,#16609);
#14390=AXIS2_PLACEMENT_3D('',#34081,#16611,#16612);
#14391=AXIS2_PLACEMENT_3D('',#34087,#16615,#16616);
#14392=AXIS2_PLACEMENT_3D('',#34093,#16619,#16620);
#14393=AXIS2_PLACEMENT_3D('',#34099,#16623,#16624);
#14394=AXIS2_PLACEMENT_3D('',#34105,#16627,#16628);
#14395=AXIS2_PLACEMENT_3D('',#34111,#16631,#16632);
#14396=AXIS2_PLACEMENT_3D('',#34117,#16635,#16636);
#14397=AXIS2_PLACEMENT_3D('',#34123,#16639,#16640);
#14398=AXIS2_PLACEMENT_3D('',#34129,#16643,#16644);
#14399=AXIS2_PLACEMENT_3D('',#34135,#16647,#16648);
#14400=AXIS2_PLACEMENT_3D('',#34141,#16651,#16652);
#14401=AXIS2_PLACEMENT_3D('',#34147,#16655,#16656);
#14402=AXIS2_PLACEMENT_3D('',#34153,#16659,#16660);
#14403=AXIS2_PLACEMENT_3D('',#34159,#16663,#16664);
#14404=AXIS2_PLACEMENT_3D('',#34165,#16667,#16668);
#14405=AXIS2_PLACEMENT_3D('',#34171,#16671,#16672);
#14406=AXIS2_PLACEMENT_3D('',#34177,#16675,#16676);
#14407=AXIS2_PLACEMENT_3D('',#34183,#16679,#16680);
#14408=AXIS2_PLACEMENT_3D('',#34189,#16683,#16684);
#14409=AXIS2_PLACEMENT_3D('',#34195,#16687,#16688);
#14410=AXIS2_PLACEMENT_3D('',#34201,#16691,#16692);
#14411=AXIS2_PLACEMENT_3D('',#34207,#16695,#16696);
#14412=AXIS2_PLACEMENT_3D('',#34213,#16699,#16700);
#14413=AXIS2_PLACEMENT_3D('',#34219,#16703,#16704);
#14414=AXIS2_PLACEMENT_3D('',#34225,#16707,#16708);
#14415=AXIS2_PLACEMENT_3D('',#34231,#16711,#16712);
#14416=AXIS2_PLACEMENT_3D('',#34237,#16715,#16716);
#14417=AXIS2_PLACEMENT_3D('',#34243,#16719,#16720);
#14418=AXIS2_PLACEMENT_3D('',#34249,#16723,#16724);
#14419=AXIS2_PLACEMENT_3D('',#34255,#16727,#16728);
#14420=AXIS2_PLACEMENT_3D('',#34261,#16731,#16732);
#14421=AXIS2_PLACEMENT_3D('',#34267,#16735,#16736);
#14422=AXIS2_PLACEMENT_3D('',#34273,#16739,#16740);
#14423=AXIS2_PLACEMENT_3D('',#34279,#16743,#16744);
#14424=AXIS2_PLACEMENT_3D('',#34285,#16747,#16748);
#14425=AXIS2_PLACEMENT_3D('',#34291,#16751,#16752);
#14426=AXIS2_PLACEMENT_3D('',#34297,#16755,#16756);
#14427=AXIS2_PLACEMENT_3D('',#34303,#16759,#16760);
#14428=AXIS2_PLACEMENT_3D('',#34309,#16763,#16764);
#14429=AXIS2_PLACEMENT_3D('',#34315,#16767,#16768);
#14430=AXIS2_PLACEMENT_3D('',#34321,#16771,#16772);
#14431=AXIS2_PLACEMENT_3D('',#34327,#16775,#16776);
#14432=AXIS2_PLACEMENT_3D('',#34333,#16779,#16780);
#14433=AXIS2_PLACEMENT_3D('',#34343,#16785,#16786);
#14434=AXIS2_PLACEMENT_3D('',#34349,#16789,#16790);
#14435=AXIS2_PLACEMENT_3D('',#34355,#16793,#16794);
#14436=AXIS2_PLACEMENT_3D('',#34361,#16797,#16798);
#14437=AXIS2_PLACEMENT_3D('',#34364,#16800,#16801);
#14438=AXIS2_PLACEMENT_3D('',#34366,#16802,#16803);
#14439=AXIS2_PLACEMENT_3D('',#34372,#16806,#16807);
#14440=AXIS2_PLACEMENT_3D('',#34378,#16810,#16811);
#14441=AXIS2_PLACEMENT_3D('',#34384,#16814,#16815);
#14442=AXIS2_PLACEMENT_3D('',#34390,#16818,#16819);
#14443=AXIS2_PLACEMENT_3D('',#34400,#16824,#16825);
#14444=AXIS2_PLACEMENT_3D('',#34406,#16828,#16829);
#14445=AXIS2_PLACEMENT_3D('',#34412,#16832,#16833);
#14446=AXIS2_PLACEMENT_3D('',#34418,#16836,#16837);
#14447=AXIS2_PLACEMENT_3D('',#34424,#16840,#16841);
#14448=AXIS2_PLACEMENT_3D('',#34430,#16844,#16845);
#14449=AXIS2_PLACEMENT_3D('',#34436,#16848,#16849);
#14450=AXIS2_PLACEMENT_3D('',#34442,#16852,#16853);
#14451=AXIS2_PLACEMENT_3D('',#34448,#16856,#16857);
#14452=AXIS2_PLACEMENT_3D('',#34454,#16860,#16861);
#14453=AXIS2_PLACEMENT_3D('',#34460,#16864,#16865);
#14454=AXIS2_PLACEMENT_3D('',#34466,#16868,#16869);
#14455=AXIS2_PLACEMENT_3D('',#34472,#16872,#16873);
#14456=AXIS2_PLACEMENT_3D('',#34478,#16876,#16877);
#14457=AXIS2_PLACEMENT_3D('',#34484,#16880,#16881);
#14458=AXIS2_PLACEMENT_3D('',#34490,#16884,#16885);
#14459=AXIS2_PLACEMENT_3D('',#34496,#16888,#16889);
#14460=AXIS2_PLACEMENT_3D('',#34502,#16892,#16893);
#14461=AXIS2_PLACEMENT_3D('',#34508,#16896,#16897);
#14462=AXIS2_PLACEMENT_3D('',#34514,#16900,#16901);
#14463=AXIS2_PLACEMENT_3D('',#34520,#16904,#16905);
#14464=AXIS2_PLACEMENT_3D('',#34526,#16908,#16909);
#14465=AXIS2_PLACEMENT_3D('',#34532,#16912,#16913);
#14466=AXIS2_PLACEMENT_3D('',#34538,#16916,#16917);
#14467=AXIS2_PLACEMENT_3D('',#34544,#16920,#16921);
#14468=AXIS2_PLACEMENT_3D('',#34550,#16924,#16925);
#14469=AXIS2_PLACEMENT_3D('',#34556,#16928,#16929);
#14470=AXIS2_PLACEMENT_3D('',#34562,#16932,#16933);
#14471=AXIS2_PLACEMENT_3D('',#34568,#16936,#16937);
#14472=AXIS2_PLACEMENT_3D('',#34574,#16940,#16941);
#14473=AXIS2_PLACEMENT_3D('',#34580,#16944,#16945);
#14474=AXIS2_PLACEMENT_3D('',#34586,#16948,#16949);
#14475=AXIS2_PLACEMENT_3D('',#34592,#16952,#16953);
#14476=AXIS2_PLACEMENT_3D('',#34598,#16956,#16957);
#14477=AXIS2_PLACEMENT_3D('',#34604,#16960,#16961);
#14478=AXIS2_PLACEMENT_3D('',#34610,#16964,#16965);
#14479=AXIS2_PLACEMENT_3D('',#34616,#16968,#16969);
#14480=AXIS2_PLACEMENT_3D('',#34622,#16972,#16973);
#14481=AXIS2_PLACEMENT_3D('',#34628,#16976,#16977);
#14482=AXIS2_PLACEMENT_3D('',#34634,#16980,#16981);
#14483=AXIS2_PLACEMENT_3D('',#34640,#16984,#16985);
#14484=AXIS2_PLACEMENT_3D('',#34646,#16988,#16989);
#14485=AXIS2_PLACEMENT_3D('',#34652,#16992,#16993);
#14486=AXIS2_PLACEMENT_3D('',#34653,#16994,#16995);
#14487=AXIS2_PLACEMENT_3D('',#34655,#16996,#16997);
#14488=AXIS2_PLACEMENT_3D('',#34658,#17000,#17001);
#14489=AXIS2_PLACEMENT_3D('',#34660,#17003,#17004);
#14490=AXIS2_PLACEMENT_3D('',#34662,#17006,#17007);
#14491=AXIS2_PLACEMENT_3D('',#34664,#17009,#17010);
#14492=AXIS2_PLACEMENT_3D('',#34666,#17012,#17013);
#14493=AXIS2_PLACEMENT_3D('',#34668,#17015,#17016);
#14494=AXIS2_PLACEMENT_3D('',#34670,#17018,#17019);
#14495=AXIS2_PLACEMENT_3D('',#34672,#17021,#17022);
#14496=AXIS2_PLACEMENT_3D('',#34674,#17024,#17025);
#14497=AXIS2_PLACEMENT_3D('',#34676,#17027,#17028);
#14498=AXIS2_PLACEMENT_3D('',#34678,#17030,#17031);
#14499=AXIS2_PLACEMENT_3D('',#34680,#17033,#17034);
#14500=AXIS2_PLACEMENT_3D('',#34682,#17036,#17037);
#14501=AXIS2_PLACEMENT_3D('',#34684,#17039,#17040);
#14502=AXIS2_PLACEMENT_3D('',#34686,#17042,#17043);
#14503=AXIS2_PLACEMENT_3D('',#34688,#17045,#17046);
#14504=AXIS2_PLACEMENT_3D('',#34690,#17048,#17049);
#14505=AXIS2_PLACEMENT_3D('',#34692,#17051,#17052);
#14506=AXIS2_PLACEMENT_3D('',#34694,#17054,#17055);
#14507=AXIS2_PLACEMENT_3D('',#34696,#17057,#17058);
#14508=AXIS2_PLACEMENT_3D('',#34698,#17060,#17061);
#14509=AXIS2_PLACEMENT_3D('',#34700,#17063,#17064);
#14510=AXIS2_PLACEMENT_3D('',#34702,#17066,#17067);
#14511=AXIS2_PLACEMENT_3D('',#34704,#17069,#17070);
#14512=AXIS2_PLACEMENT_3D('',#34706,#17072,#17073);
#14513=AXIS2_PLACEMENT_3D('',#34708,#17075,#17076);
#14514=AXIS2_PLACEMENT_3D('',#34710,#17078,#17079);
#14515=AXIS2_PLACEMENT_3D('',#34712,#17081,#17082);
#14516=AXIS2_PLACEMENT_3D('',#34714,#17084,#17085);
#14517=AXIS2_PLACEMENT_3D('',#34716,#17087,#17088);
#14518=AXIS2_PLACEMENT_3D('',#34718,#17090,#17091);
#14519=AXIS2_PLACEMENT_3D('',#34720,#17093,#17094);
#14520=AXIS2_PLACEMENT_3D('',#34722,#17096,#17097);
#14521=AXIS2_PLACEMENT_3D('',#34724,#17099,#17100);
#14522=AXIS2_PLACEMENT_3D('',#34726,#17102,#17103);
#14523=AXIS2_PLACEMENT_3D('',#34728,#17105,#17106);
#14524=AXIS2_PLACEMENT_3D('',#34730,#17108,#17109);
#14525=AXIS2_PLACEMENT_3D('',#34732,#17111,#17112);
#14526=AXIS2_PLACEMENT_3D('',#34734,#17114,#17115);
#14527=AXIS2_PLACEMENT_3D('',#34736,#17117,#17118);
#14528=AXIS2_PLACEMENT_3D('',#34738,#17120,#17121);
#14529=AXIS2_PLACEMENT_3D('',#34740,#17123,#17124);
#14530=AXIS2_PLACEMENT_3D('',#34742,#17126,#17127);
#14531=AXIS2_PLACEMENT_3D('',#34744,#17129,#17130);
#14532=AXIS2_PLACEMENT_3D('',#34746,#17132,#17133);
#14533=AXIS2_PLACEMENT_3D('',#34748,#17135,#17136);
#14534=AXIS2_PLACEMENT_3D('',#34750,#17138,#17139);
#14535=AXIS2_PLACEMENT_3D('',#34752,#17141,#17142);
#14536=AXIS2_PLACEMENT_3D('',#34754,#17144,#17145);
#14537=AXIS2_PLACEMENT_3D('',#34756,#17147,#17148);
#14538=AXIS2_PLACEMENT_3D('',#34758,#17150,#17151);
#14539=AXIS2_PLACEMENT_3D('',#34760,#17153,#17154);
#14540=AXIS2_PLACEMENT_3D('',#34762,#17156,#17157);
#14541=AXIS2_PLACEMENT_3D('',#34764,#17159,#17160);
#14542=AXIS2_PLACEMENT_3D('',#34766,#17162,#17163);
#14543=AXIS2_PLACEMENT_3D('',#34768,#17165,#17166);
#14544=AXIS2_PLACEMENT_3D('',#34770,#17168,#17169);
#14545=AXIS2_PLACEMENT_3D('',#34772,#17171,#17172);
#14546=AXIS2_PLACEMENT_3D('',#34774,#17174,#17175);
#14547=AXIS2_PLACEMENT_3D('',#34776,#17177,#17178);
#14548=AXIS2_PLACEMENT_3D('',#34778,#17180,#17181);
#14549=AXIS2_PLACEMENT_3D('',#34780,#17183,#17184);
#14550=AXIS2_PLACEMENT_3D('',#34782,#17186,#17187);
#14551=AXIS2_PLACEMENT_3D('',#34784,#17189,#17190);
#14552=AXIS2_PLACEMENT_3D('',#34786,#17192,#17193);
#14553=AXIS2_PLACEMENT_3D('',#34788,#17195,#17196);
#14554=AXIS2_PLACEMENT_3D('',#34790,#17198,#17199);
#14555=AXIS2_PLACEMENT_3D('',#34792,#17201,#17202);
#14556=AXIS2_PLACEMENT_3D('',#34794,#17204,#17205);
#14557=AXIS2_PLACEMENT_3D('',#34796,#17207,#17208);
#14558=AXIS2_PLACEMENT_3D('',#34798,#17210,#17211);
#14559=AXIS2_PLACEMENT_3D('',#34800,#17213,#17214);
#14560=AXIS2_PLACEMENT_3D('',#34802,#17216,#17217);
#14561=AXIS2_PLACEMENT_3D('',#34804,#17219,#17220);
#14562=AXIS2_PLACEMENT_3D('',#34806,#17222,#17223);
#14563=AXIS2_PLACEMENT_3D('',#34808,#17225,#17226);
#14564=AXIS2_PLACEMENT_3D('',#34810,#17228,#17229);
#14565=AXIS2_PLACEMENT_3D('',#34812,#17231,#17232);
#14566=AXIS2_PLACEMENT_3D('',#34814,#17234,#17235);
#14567=AXIS2_PLACEMENT_3D('',#34816,#17237,#17238);
#14568=AXIS2_PLACEMENT_3D('',#34818,#17240,#17241);
#14569=AXIS2_PLACEMENT_3D('',#34820,#17243,#17244);
#14570=AXIS2_PLACEMENT_3D('',#34822,#17246,#17247);
#14571=AXIS2_PLACEMENT_3D('',#34824,#17249,#17250);
#14572=AXIS2_PLACEMENT_3D('',#34826,#17252,#17253);
#14573=AXIS2_PLACEMENT_3D('',#34828,#17255,#17256);
#14574=AXIS2_PLACEMENT_3D('',#34830,#17258,#17259);
#14575=AXIS2_PLACEMENT_3D('',#34832,#17261,#17262);
#14576=AXIS2_PLACEMENT_3D('',#34834,#17264,#17265);
#14577=AXIS2_PLACEMENT_3D('',#34836,#17267,#17268);
#14578=AXIS2_PLACEMENT_3D('',#34838,#17270,#17271);
#14579=AXIS2_PLACEMENT_3D('',#34840,#17273,#17274);
#14580=AXIS2_PLACEMENT_3D('',#34842,#17276,#17277);
#14581=AXIS2_PLACEMENT_3D('',#34844,#17279,#17280);
#14582=AXIS2_PLACEMENT_3D('',#34846,#17282,#17283);
#14583=AXIS2_PLACEMENT_3D('',#34848,#17285,#17286);
#14584=AXIS2_PLACEMENT_3D('',#34850,#17288,#17289);
#14585=AXIS2_PLACEMENT_3D('',#34852,#17291,#17292);
#14586=AXIS2_PLACEMENT_3D('',#34854,#17294,#17295);
#14587=AXIS2_PLACEMENT_3D('',#34856,#17297,#17298);
#14588=AXIS2_PLACEMENT_3D('',#34858,#17300,#17301);
#14589=AXIS2_PLACEMENT_3D('',#34860,#17303,#17304);
#14590=AXIS2_PLACEMENT_3D('',#34862,#17306,#17307);
#14591=AXIS2_PLACEMENT_3D('',#34864,#17309,#17310);
#14592=AXIS2_PLACEMENT_3D('',#34866,#17312,#17313);
#14593=AXIS2_PLACEMENT_3D('',#34868,#17315,#17316);
#14594=AXIS2_PLACEMENT_3D('',#34870,#17318,#17319);
#14595=AXIS2_PLACEMENT_3D('',#34872,#17321,#17322);
#14596=AXIS2_PLACEMENT_3D('',#34874,#17324,#17325);
#14597=AXIS2_PLACEMENT_3D('',#34876,#17327,#17328);
#14598=AXIS2_PLACEMENT_3D('',#34878,#17330,#17331);
#14599=AXIS2_PLACEMENT_3D('',#34880,#17333,#17334);
#14600=AXIS2_PLACEMENT_3D('',#34882,#17336,#17337);
#14601=AXIS2_PLACEMENT_3D('',#34884,#17339,#17340);
#14602=AXIS2_PLACEMENT_3D('',#34886,#17342,#17343);
#14603=AXIS2_PLACEMENT_3D('',#34888,#17345,#17346);
#14604=AXIS2_PLACEMENT_3D('',#34890,#17348,#17349);
#14605=AXIS2_PLACEMENT_3D('',#34892,#17351,#17352);
#14606=AXIS2_PLACEMENT_3D('',#34894,#17354,#17355);
#14607=AXIS2_PLACEMENT_3D('',#34896,#17357,#17358);
#14608=AXIS2_PLACEMENT_3D('',#34898,#17360,#17361);
#14609=AXIS2_PLACEMENT_3D('',#34900,#17363,#17364);
#14610=AXIS2_PLACEMENT_3D('',#34902,#17366,#17367);
#14611=AXIS2_PLACEMENT_3D('',#34904,#17369,#17370);
#14612=AXIS2_PLACEMENT_3D('',#34906,#17372,#17373);
#14613=AXIS2_PLACEMENT_3D('',#34908,#17375,#17376);
#14614=AXIS2_PLACEMENT_3D('',#34910,#17378,#17379);
#14615=AXIS2_PLACEMENT_3D('',#34912,#17381,#17382);
#14616=AXIS2_PLACEMENT_3D('',#34914,#17384,#17385);
#14617=AXIS2_PLACEMENT_3D('',#34916,#17387,#17388);
#14618=AXIS2_PLACEMENT_3D('',#34918,#17390,#17391);
#14619=AXIS2_PLACEMENT_3D('',#34920,#17393,#17394);
#14620=AXIS2_PLACEMENT_3D('',#34922,#17396,#17397);
#14621=AXIS2_PLACEMENT_3D('',#34924,#17399,#17400);
#14622=AXIS2_PLACEMENT_3D('',#34926,#17402,#17403);
#14623=AXIS2_PLACEMENT_3D('',#34928,#17405,#17406);
#14624=AXIS2_PLACEMENT_3D('',#34930,#17408,#17409);
#14625=AXIS2_PLACEMENT_3D('',#34932,#17411,#17412);
#14626=AXIS2_PLACEMENT_3D('',#34934,#17414,#17415);
#14627=AXIS2_PLACEMENT_3D('',#34936,#17417,#17418);
#14628=AXIS2_PLACEMENT_3D('',#34938,#17420,#17421);
#14629=AXIS2_PLACEMENT_3D('',#34940,#17423,#17424);
#14630=AXIS2_PLACEMENT_3D('',#34941,#17425,#17426);
#14631=AXIS2_PLACEMENT_3D('',#34942,#17427,#17428);
#14632=AXIS2_PLACEMENT_3D('',#34943,#17429,#17430);
#14633=AXIS2_PLACEMENT_3D('',#34945,#17431,#17432);
#14634=AXIS2_PLACEMENT_3D('',#34946,#17433,#17434);
#14635=AXIS2_PLACEMENT_3D('',#34947,#17435,#17436);
#14636=AXIS2_PLACEMENT_3D('',#34948,#17437,#17438);
#14637=AXIS2_PLACEMENT_3D('',#34950,#17439,#17440);
#14638=AXIS2_PLACEMENT_3D('',#34951,#17441,#17442);
#14639=AXIS2_PLACEMENT_3D('',#34953,#17443,#17444);
#14640=AXIS2_PLACEMENT_3D('',#34954,#17445,#17446);
#14641=AXIS2_PLACEMENT_3D('',#34955,#17447,#17448);
#14642=AXIS2_PLACEMENT_3D('',#34956,#17449,#17450);
#14643=AXIS2_PLACEMENT_3D('',#34957,#17451,#17452);
#14644=AXIS2_PLACEMENT_3D('',#34959,#17453,#17454);
#14645=AXIS2_PLACEMENT_3D('',#34961,#17455,#17456);
#14646=AXIS2_PLACEMENT_3D('',#34962,#17457,#17458);
#14647=AXIS2_PLACEMENT_3D('',#34964,#17459,#17460);
#14648=AXIS2_PLACEMENT_3D('',#34966,#17461,#17462);
#14649=AXIS2_PLACEMENT_3D('',#34967,#17463,#17464);
#14650=AXIS2_PLACEMENT_3D('',#34968,#17465,#17466);
#14651=AXIS2_PLACEMENT_3D('',#34969,#17467,#17468);
#14652=AXIS2_PLACEMENT_3D('',#34970,#17469,#17470);
#14653=AXIS2_PLACEMENT_3D('',#34972,#17471,#17472);
#14654=AXIS2_PLACEMENT_3D('',#34974,#17473,#17474);
#14655=AXIS2_PLACEMENT_3D('',#34975,#17475,#17476);
#14656=AXIS2_PLACEMENT_3D('',#34977,#17477,#17478);
#14657=AXIS2_PLACEMENT_3D('',#34979,#17479,#17480);
#14658=AXIS2_PLACEMENT_3D('',#34980,#17481,#17482);
#14659=AXIS2_PLACEMENT_3D('',#34981,#17483,#17484);
#14660=AXIS2_PLACEMENT_3D('',#34982,#17485,#17486);
#14661=AXIS2_PLACEMENT_3D('',#34983,#17487,#17488);
#14662=AXIS2_PLACEMENT_3D('',#34984,#17489,#17490);
#14663=AXIS2_PLACEMENT_3D('',#34987,#17491,#17492);
#14664=AXIS2_PLACEMENT_3D('',#34989,#17493,#17494);
#14665=AXIS2_PLACEMENT_3D('',#34991,#17495,#17496);
#14666=AXIS2_PLACEMENT_3D('',#34992,#17497,#17498);
#14667=AXIS2_PLACEMENT_3D('',#34993,#17499,#17500);
#14668=AXIS2_PLACEMENT_3D('',#34998,#17503,#17504);
#14669=AXIS2_PLACEMENT_3D('',#34999,#17505,#17506);
#14670=AXIS2_PLACEMENT_3D('',#35004,#17509,#17510);
#14671=AXIS2_PLACEMENT_3D('',#35005,#17511,#17512);
#14672=AXIS2_PLACEMENT_3D('',#35008,#17513,#17514);
#14673=AXIS2_PLACEMENT_3D('',#35010,#17515,#17516);
#14674=AXIS2_PLACEMENT_3D('',#35012,#17517,#17518);
#14675=AXIS2_PLACEMENT_3D('',#35013,#17519,#17520);
#14676=AXIS2_PLACEMENT_3D('',#35014,#17521,#17522);
#14677=AXIS2_PLACEMENT_3D('',#35019,#17525,#17526);
#14678=AXIS2_PLACEMENT_3D('',#35020,#17527,#17528);
#14679=AXIS2_PLACEMENT_3D('',#35025,#17531,#17532);
#14680=AXIS2_PLACEMENT_3D('',#35026,#17533,#17534);
#14681=AXIS2_PLACEMENT_3D('',#35028,#17535,#17536);
#14682=AXIS2_PLACEMENT_3D('',#35029,#17537,#17538);
#14683=AXIS2_PLACEMENT_3D('',#35031,#17539,#17540);
#14684=AXIS2_PLACEMENT_3D('',#35032,#17541,#17542);
#14685=AXIS2_PLACEMENT_3D('',#35033,#17543,#17544);
#14686=AXIS2_PLACEMENT_3D('',#35034,#17545,#17546);
#14687=AXIS2_PLACEMENT_3D('',#35036,#17547,#17548);
#14688=AXIS2_PLACEMENT_3D('',#35038,#17549,#17550);
#14689=AXIS2_PLACEMENT_3D('',#35039,#17551,#17552);
#14690=AXIS2_PLACEMENT_3D('',#35040,#17553,#17554);
#14691=AXIS2_PLACEMENT_3D('',#35041,#17555,#17556);
#14692=AXIS2_PLACEMENT_3D('',#35042,#17557,#17558);
#14693=AXIS2_PLACEMENT_3D('',#35043,#17559,#17560);
#14694=AXIS2_PLACEMENT_3D('',#35044,#17561,#17562);
#14695=AXIS2_PLACEMENT_3D('',#35045,#17563,#17564);
#14696=AXIS2_PLACEMENT_3D('',#35046,#17565,#17566);
#14697=AXIS2_PLACEMENT_3D('',#35047,#17567,#17568);
#14698=AXIS2_PLACEMENT_3D('',#35049,#17569,#17570);
#14699=AXIS2_PLACEMENT_3D('',#35050,#17571,#17572);
#14700=AXIS2_PLACEMENT_3D('',#35059,#17577,#17578);
#14701=AXIS2_PLACEMENT_3D('',#35060,#17579,#17580);
#14702=AXIS2_PLACEMENT_3D('',#35064,#17582,#17583);
#14703=AXIS2_PLACEMENT_3D('',#35065,#17584,#17585);
#14704=AXIS2_PLACEMENT_3D('',#35071,#17589,#17590);
#14705=AXIS2_PLACEMENT_3D('',#35080,#17595,#17596);
#14706=AXIS2_PLACEMENT_3D('',#35089,#17601,#17602);
#14707=AXIS2_PLACEMENT_3D('',#35090,#17603,#17604);
#14708=AXIS2_PLACEMENT_3D('',#35091,#17605,#17606);
#14709=AXIS2_PLACEMENT_3D('',#35092,#17607,#17608);
#14710=AXIS2_PLACEMENT_3D('',#35101,#17613,#17614);
#14711=AXIS2_PLACEMENT_3D('',#35110,#17619,#17620);
#14712=AXIS2_PLACEMENT_3D('',#35111,#17621,#17622);
#14713=AXIS2_PLACEMENT_3D('',#35112,#17623,#17624);
#14714=AXIS2_PLACEMENT_3D('',#35113,#17625,#17626);
#14715=AXIS2_PLACEMENT_3D('',#35114,#17627,#17628);
#14716=AXIS2_PLACEMENT_3D('',#35116,#17629,#17630);
#14717=AXIS2_PLACEMENT_3D('',#35118,#17631,#17632);
#14718=AXIS2_PLACEMENT_3D('',#35119,#17633,#17634);
#14719=AXIS2_PLACEMENT_3D('',#35121,#17635,#17636);
#14720=AXIS2_PLACEMENT_3D('',#35123,#17637,#17638);
#14721=AXIS2_PLACEMENT_3D('',#35124,#17639,#17640);
#14722=AXIS2_PLACEMENT_3D('',#35126,#17641,#17642);
#14723=AXIS2_PLACEMENT_3D('',#35128,#17643,#17644);
#14724=AXIS2_PLACEMENT_3D('',#35129,#17645,#17646);
#14725=AXIS2_PLACEMENT_3D('',#35131,#17647,#17648);
#14726=AXIS2_PLACEMENT_3D('',#35133,#17649,#17650);
#14727=AXIS2_PLACEMENT_3D('',#35135,#17651,#17652);
#14728=AXIS2_PLACEMENT_3D('',#35136,#17653,#17654);
#14729=AXIS2_PLACEMENT_3D('',#35137,#17655,#17656);
#14730=AXIS2_PLACEMENT_3D('',#35138,#17657,#17658);
#14731=AXIS2_PLACEMENT_3D('',#35140,#17659,#17660);
#14732=AXIS2_PLACEMENT_3D('',#35142,#17661,#17662);
#14733=AXIS2_PLACEMENT_3D('',#35143,#17663,#17664);
#14734=AXIS2_PLACEMENT_3D('',#35145,#17665,#17666);
#14735=AXIS2_PLACEMENT_3D('',#35147,#17667,#17668);
#14736=AXIS2_PLACEMENT_3D('',#35149,#17669,#17670);
#14737=AXIS2_PLACEMENT_3D('',#35150,#17671,#17672);
#14738=AXIS2_PLACEMENT_3D('',#35151,#17673,#17674);
#14739=AXIS2_PLACEMENT_3D('',#35152,#17675,#17676);
#14740=AXIS2_PLACEMENT_3D('',#35154,#17677,#17678);
#14741=AXIS2_PLACEMENT_3D('',#35156,#17679,#17680);
#14742=AXIS2_PLACEMENT_3D('',#35157,#17681,#17682);
#14743=AXIS2_PLACEMENT_3D('',#35159,#17683,#17684);
#14744=AXIS2_PLACEMENT_3D('',#35161,#17685,#17686);
#14745=AXIS2_PLACEMENT_3D('',#35162,#17687,#17688);
#14746=AXIS2_PLACEMENT_3D('',#35164,#17689,#17690);
#14747=AXIS2_PLACEMENT_3D('',#35166,#17691,#17692);
#14748=AXIS2_PLACEMENT_3D('',#35167,#17693,#17694);
#14749=AXIS2_PLACEMENT_3D('',#35168,#17695,#17696);
#14750=AXIS2_PLACEMENT_3D('',#35169,#17697,#17698);
#14751=AXIS2_PLACEMENT_3D('',#35170,#17699,#17700);
#14752=AXIS2_PLACEMENT_3D('',#35171,#17701,#17702);
#14753=AXIS2_PLACEMENT_3D('',#35172,#17703,#17704);
#14754=AXIS2_PLACEMENT_3D('',#35173,#17705,#17706);
#14755=AXIS2_PLACEMENT_3D('',#35174,#17707,#17708);
#14756=AXIS2_PLACEMENT_3D('',#35175,#17709,#17710);
#14757=AXIS2_PLACEMENT_3D('',#35176,#17711,#17712);
#14758=AXIS2_PLACEMENT_3D('',#35177,#17713,#17714);
#14759=AXIS2_PLACEMENT_3D('',#35178,#17715,#17716);
#14760=AXIS2_PLACEMENT_3D('',#35179,#17717,#17718);
#14761=AXIS2_PLACEMENT_3D('',#35180,#17719,#17720);
#14762=AXIS2_PLACEMENT_3D('',#35182,#17721,#17722);
#14763=AXIS2_PLACEMENT_3D('',#35183,#17723,#17724);
#14764=AXIS2_PLACEMENT_3D('',#35184,#17725,#17726);
#14765=AXIS2_PLACEMENT_3D('',#35185,#17727,#17728);
#14766=AXIS2_PLACEMENT_3D('',#35186,#17729,#17730);
#14767=AXIS2_PLACEMENT_3D('',#35191,#17732,#17733);
#14768=AXIS2_PLACEMENT_3D('',#35194,#17735,#17736);
#14769=AXIS2_PLACEMENT_3D('',#35200,#17740,#17741);
#14770=AXIS2_PLACEMENT_3D('',#35206,#17745,#17746);
#14771=AXIS2_PLACEMENT_3D('',#35207,#17747,#17748);
#14772=AXIS2_PLACEMENT_3D('',#35208,#17749,#17750);
#14773=AXIS2_PLACEMENT_3D('',#35209,#17751,#17752);
#14774=AXIS2_PLACEMENT_3D('',#35214,#17754,#17755);
#14775=AXIS2_PLACEMENT_3D('',#35217,#17757,#17758);
#14776=AXIS2_PLACEMENT_3D('',#35223,#17762,#17763);
#14777=AXIS2_PLACEMENT_3D('',#35229,#17767,#17768);
#14778=AXIS2_PLACEMENT_3D('',#35230,#17769,#17770);
#14779=AXIS2_PLACEMENT_3D('',#35231,#17771,#17772);
#14780=AXIS2_PLACEMENT_3D('',#35232,#17773,#17774);
#14781=AXIS2_PLACEMENT_3D('',#35237,#17776,#17777);
#14782=AXIS2_PLACEMENT_3D('',#35240,#17779,#17780);
#14783=AXIS2_PLACEMENT_3D('',#35246,#17784,#17785);
#14784=AXIS2_PLACEMENT_3D('',#35252,#17789,#17790);
#14785=AXIS2_PLACEMENT_3D('',#35253,#17791,#17792);
#14786=AXIS2_PLACEMENT_3D('',#35254,#17793,#17794);
#14787=AXIS2_PLACEMENT_3D('',#35255,#17795,#17796);
#14788=AXIS2_PLACEMENT_3D('',#35257,#17797,#17798);
#14789=AXIS2_PLACEMENT_3D('',#35259,#17799,#17800);
#14790=AXIS2_PLACEMENT_3D('',#35260,#17801,#17802);
#14791=AXIS2_PLACEMENT_3D('',#35261,#17803,#17804);
#14792=AXIS2_PLACEMENT_3D('',#35262,#17805,#17806);
#14793=AXIS2_PLACEMENT_3D('',#35263,#17807,#17808);
#14794=AXIS2_PLACEMENT_3D('',#35265,#17809,#17810);
#14795=AXIS2_PLACEMENT_3D('',#35267,#17811,#17812);
#14796=AXIS2_PLACEMENT_3D('',#35268,#17813,#17814);
#14797=AXIS2_PLACEMENT_3D('',#35269,#17815,#17816);
#14798=AXIS2_PLACEMENT_3D('',#35270,#17817,#17818);
#14799=AXIS2_PLACEMENT_3D('',#35271,#17819,#17820);
#14800=AXIS2_PLACEMENT_3D('',#35272,#17821,#17822);
#14801=AXIS2_PLACEMENT_3D('',#35273,#17823,#17824);
#14802=AXIS2_PLACEMENT_3D('',#35282,#17829,#17830);
#14803=AXIS2_PLACEMENT_3D('',#35291,#17835,#17836);
#14804=AXIS2_PLACEMENT_3D('',#35300,#17841,#17842);
#14805=AXIS2_PLACEMENT_3D('',#35309,#17847,#17848);
#14806=AXIS2_PLACEMENT_3D('',#35310,#17849,#17850);
#14807=AXIS2_PLACEMENT_3D('',#35313,#17851,#17852);
#14808=AXIS2_PLACEMENT_3D('',#35315,#17853,#17854);
#14809=AXIS2_PLACEMENT_3D('',#35317,#17855,#17856);
#14810=AXIS2_PLACEMENT_3D('',#35318,#17857,#17858);
#14811=AXIS2_PLACEMENT_3D('',#35319,#17859,#17860);
#14812=AXIS2_PLACEMENT_3D('',#35324,#17863,#17864);
#14813=AXIS2_PLACEMENT_3D('',#35325,#17865,#17866);
#14814=AXIS2_PLACEMENT_3D('',#35330,#17869,#17870);
#14815=AXIS2_PLACEMENT_3D('',#35331,#17871,#17872);
#14816=AXIS2_PLACEMENT_3D('',#35334,#17873,#17874);
#14817=AXIS2_PLACEMENT_3D('',#35336,#17875,#17876);
#14818=AXIS2_PLACEMENT_3D('',#35338,#17877,#17878);
#14819=AXIS2_PLACEMENT_3D('',#35339,#17879,#17880);
#14820=AXIS2_PLACEMENT_3D('',#35340,#17881,#17882);
#14821=AXIS2_PLACEMENT_3D('',#35345,#17885,#17886);
#14822=AXIS2_PLACEMENT_3D('',#35346,#17887,#17888);
#14823=AXIS2_PLACEMENT_3D('',#35351,#17891,#17892);
#14824=AXIS2_PLACEMENT_3D('',#35352,#17893,#17894);
#14825=AXIS2_PLACEMENT_3D('',#35353,#17895,#17896);
#14826=AXIS2_PLACEMENT_3D('',#35354,#17897,#17898);
#14827=AXIS2_PLACEMENT_3D('',#35355,#17899,#17900);
#14828=AXIS2_PLACEMENT_3D('',#35356,#17901,#17902);
#14829=AXIS2_PLACEMENT_3D('',#35357,#17903,#17904);
#14830=AXIS2_PLACEMENT_3D('',#35359,#17905,#17906);
#14831=AXIS2_PLACEMENT_3D('',#35360,#17907,#17908);
#14832=AXIS2_PLACEMENT_3D('',#35361,#17909,#17910);
#14833=AXIS2_PLACEMENT_3D('',#35362,#17911,#17912);
#14834=AXIS2_PLACEMENT_3D('',#35363,#17913,#17914);
#14835=AXIS2_PLACEMENT_3D('',#35364,#17915,#17916);
#14836=AXIS2_PLACEMENT_3D('',#35365,#17917,#17918);
#14837=AXIS2_PLACEMENT_3D('',#35366,#17919,#17920);
#14838=AXIS2_PLACEMENT_3D('',#35367,#17921,#17922);
#14839=AXIS2_PLACEMENT_3D('',#35368,#17923,#17924);
#14840=AXIS2_PLACEMENT_3D('',#35369,#17925,#17926);
#14841=AXIS2_PLACEMENT_3D('',#35370,#17927,#17928);
#14842=AXIS2_PLACEMENT_3D('',#35371,#17929,#17930);
#14843=AXIS2_PLACEMENT_3D('',#35372,#17931,#17932);
#14844=AXIS2_PLACEMENT_3D('',#35373,#17933,#17934);
#14845=AXIS2_PLACEMENT_3D('',#35374,#17935,#17936);
#14846=AXIS2_PLACEMENT_3D('',#35375,#17937,#17938);
#14847=AXIS2_PLACEMENT_3D('',#35376,#17939,#17940);
#14848=AXIS2_PLACEMENT_3D('',#35377,#17941,#17942);
#14849=AXIS2_PLACEMENT_3D('',#35378,#17943,#17944);
#14850=AXIS2_PLACEMENT_3D('',#35380,#17945,#17946);
#14851=AXIS2_PLACEMENT_3D('',#35382,#17947,#17948);
#14852=AXIS2_PLACEMENT_3D('',#35383,#17949,#17950);
#14853=AXIS2_PLACEMENT_3D('',#35388,#17952,#17953);
#14854=AXIS2_PLACEMENT_3D('',#35391,#17955,#17956);
#14855=AXIS2_PLACEMENT_3D('',#35392,#17957,#17958);
#14856=AXIS2_PLACEMENT_3D('',#35394,#17959,#17960);
#14857=AXIS2_PLACEMENT_3D('',#35399,#17962,#17963);
#14858=AXIS2_PLACEMENT_3D('',#35403,#17965,#17966);
#14859=AXIS2_PLACEMENT_3D('',#35405,#17967,#17968);
#14860=AXIS2_PLACEMENT_3D('',#35407,#17970,#17971);
#14861=AXIS2_PLACEMENT_3D('',#35408,#17972,#17973);
#14862=AXIS2_PLACEMENT_3D('',#35413,#17976,#17977);
#14863=AXIS2_PLACEMENT_3D('',#35414,#17978,#17979);
#14864=AXIS2_PLACEMENT_3D('',#35416,#17980,#17981);
#14865=AXIS2_PLACEMENT_3D('',#35420,#17983,#17984);
#14866=AXIS2_PLACEMENT_3D('',#35423,#17986,#17987);
#14867=AXIS2_PLACEMENT_3D('',#35426,#17989,#17990);
#14868=AXIS2_PLACEMENT_3D('',#35427,#17991,#17992);
#14869=AXIS2_PLACEMENT_3D('',#35429,#17993,#17994);
#14870=AXIS2_PLACEMENT_3D('',#35434,#17996,#17997);
#14871=AXIS2_PLACEMENT_3D('',#35438,#17999,#18000);
#14872=AXIS2_PLACEMENT_3D('',#35440,#18001,#18002);
#14873=AXIS2_PLACEMENT_3D('',#35442,#18003,#18004);
#14874=AXIS2_PLACEMENT_3D('',#35445,#18006,#18007);
#14875=AXIS2_PLACEMENT_3D('',#35446,#18008,#18009);
#14876=AXIS2_PLACEMENT_3D('',#35451,#18012,#18013);
#14877=AXIS2_PLACEMENT_3D('',#35452,#18014,#18015);
#14878=AXIS2_PLACEMENT_3D('',#35454,#18016,#18017);
#14879=AXIS2_PLACEMENT_3D('',#35459,#18019,#18020);
#14880=AXIS2_PLACEMENT_3D('',#35461,#18021,#18022);
#14881=AXIS2_PLACEMENT_3D('',#35464,#18024,#18025);
#14882=AXIS2_PLACEMENT_3D('',#35467,#18027,#18028);
#14883=AXIS2_PLACEMENT_3D('',#35470,#18031,#18032);
#14884=AXIS2_PLACEMENT_3D('',#35471,#18033,#18034);
#14885=AXIS2_PLACEMENT_3D('',#35473,#18035,#18036);
#14886=AXIS2_PLACEMENT_3D('',#35478,#18038,#18039);
#14887=AXIS2_PLACEMENT_3D('',#35482,#18041,#18042);
#14888=AXIS2_PLACEMENT_3D('',#35484,#18043,#18044);
#14889=AXIS2_PLACEMENT_3D('',#35486,#18045,#18046);
#14890=AXIS2_PLACEMENT_3D('',#35489,#18048,#18049);
#14891=AXIS2_PLACEMENT_3D('',#35490,#18050,#18051);
#14892=AXIS2_PLACEMENT_3D('',#35492,#18052,#18053);
#14893=AXIS2_PLACEMENT_3D('',#35497,#18055,#18056);
#14894=AXIS2_PLACEMENT_3D('',#35499,#18057,#18058);
#14895=AXIS2_PLACEMENT_3D('',#35501,#18059,#18060);
#14896=AXIS2_PLACEMENT_3D('',#35505,#18062,#18063);
#14897=AXIS2_PLACEMENT_3D('',#35508,#18065,#18066);
#14898=AXIS2_PLACEMENT_3D('',#35509,#18067,#18068);
#14899=AXIS2_PLACEMENT_3D('',#35511,#18069,#18070);
#14900=AXIS2_PLACEMENT_3D('',#35516,#18072,#18073);
#14901=AXIS2_PLACEMENT_3D('',#35520,#18075,#18076);
#14902=AXIS2_PLACEMENT_3D('',#35522,#18077,#18078);
#14903=AXIS2_PLACEMENT_3D('',#35524,#18079,#18080);
#14904=AXIS2_PLACEMENT_3D('',#35527,#18082,#18083);
#14905=AXIS2_PLACEMENT_3D('',#35528,#18084,#18085);
#14906=AXIS2_PLACEMENT_3D('',#35533,#18088,#18089);
#14907=AXIS2_PLACEMENT_3D('',#35534,#18090,#18091);
#14908=AXIS2_PLACEMENT_3D('',#35536,#18092,#18093);
#14909=AXIS2_PLACEMENT_3D('',#35541,#18095,#18096);
#14910=AXIS2_PLACEMENT_3D('',#35543,#18097,#18098);
#14911=AXIS2_PLACEMENT_3D('',#35546,#18100,#18101);
#14912=AXIS2_PLACEMENT_3D('',#35549,#18103,#18104);
#14913=AXIS2_PLACEMENT_3D('',#35552,#18107,#18108);
#14914=AXIS2_PLACEMENT_3D('',#35554,#18110,#18111);
#14915=AXIS2_PLACEMENT_3D('',#35556,#18113,#18114);
#14916=AXIS2_PLACEMENT_3D('',#35558,#18116,#18117);
#14917=AXIS2_PLACEMENT_3D('',#35560,#18119,#18120);
#14918=AXIS2_PLACEMENT_3D('',#35561,#18121,#18122);
#14919=AXIS2_PLACEMENT_3D('',#35564,#18125,#18126);
#14920=AXIS2_PLACEMENT_3D('',#35566,#18128,#18129);
#14921=AXIS2_PLACEMENT_3D('',#35568,#18131,#18132);
#14922=AXIS2_PLACEMENT_3D('',#35569,#18133,#18134);
#14923=AXIS2_PLACEMENT_3D('',#35570,#18135,#18136);
#14924=AXIS2_PLACEMENT_3D('',#35573,#18139,#18140);
#14925=AXIS2_PLACEMENT_3D('',#35575,#18142,#18143);
#14926=AXIS2_PLACEMENT_3D('',#35577,#18145,#18146);
#14927=AXIS2_PLACEMENT_3D('',#35579,#18148,#18149);
#14928=AXIS2_PLACEMENT_3D('',#35581,#18151,#18152);
#14929=AXIS2_PLACEMENT_3D('',#35584,#18155,#18156);
#14930=AXIS2_PLACEMENT_3D('',#35586,#18158,#18159);
#14931=AXIS2_PLACEMENT_3D('',#35588,#18161,#18162);
#14932=AXIS2_PLACEMENT_3D('',#35589,#18163,#18164);
#14933=AXIS2_PLACEMENT_3D('',#35590,#18165,#18166);
#14934=AXIS2_PLACEMENT_3D('',#35591,#18167,#18168);
#14935=AXIS2_PLACEMENT_3D('',#36153,#18173,#18174);
#14936=AXIS2_PLACEMENT_3D('',#36156,#18177,#18178);
#14937=AXIS2_PLACEMENT_3D('',#36158,#18180,#18181);
#14938=AXIS2_PLACEMENT_3D('',#36160,#18183,#18184);
#14939=AXIS2_PLACEMENT_3D('',#36161,#18185,#18186);
#14940=AXIS2_PLACEMENT_3D('',#36162,#18187,#18188);
#14941=AXIS2_PLACEMENT_3D('',#37425,#18189,#18190);
#14942=AXIS2_PLACEMENT_3D('',#37447,#18191,#18192);
#14943=AXIS2_PLACEMENT_3D('',#37448,#18193,#18194);
#14944=AXIS2_PLACEMENT_3D('',#38516,#18195,#18196);
#14945=AXIS2_PLACEMENT_3D('',#38769,#18197,#18198);
#14946=AXIS2_PLACEMENT_3D('',#38770,#18199,#18200);
#14947=AXIS2_PLACEMENT_3D('',#38771,#18201,#18202);
#14948=AXIS2_PLACEMENT_3D('',#38772,#18203,#18204);
#14949=AXIS2_PLACEMENT_3D('',#38773,#18205,#18206);
#14950=AXIS2_PLACEMENT_3D('',#38774,#18207,#18208);
#14951=AXIS2_PLACEMENT_3D('',#38776,#18209,#18210);
#14952=AXIS2_PLACEMENT_3D('',#38777,#18211,#18212);
#14953=AXIS2_PLACEMENT_3D('',#38779,#18213,#18214);
#14954=AXIS2_PLACEMENT_3D('',#38781,#18215,#18216);
#14955=AXIS2_PLACEMENT_3D('',#38782,#18217,#18218);
#14956=AXIS2_PLACEMENT_3D('',#38785,#18219,#18220);
#14957=AXIS2_PLACEMENT_3D('',#38786,#18221,#18222);
#14958=AXIS2_PLACEMENT_3D('',#38788,#18223,#18224);
#14959=AXIS2_PLACEMENT_3D('',#38789,#18225,#18226);
#14960=AXIS2_PLACEMENT_3D('',#38792,#18227,#18228);
#14961=AXIS2_PLACEMENT_3D('',#38793,#18229,#18230);
#14962=AXIS2_PLACEMENT_3D('',#38795,#18231,#18232);
#14963=AXIS2_PLACEMENT_3D('',#38796,#18233,#18234);
#14964=AXIS2_PLACEMENT_3D('',#38805,#18235,#18236);
#14965=AXIS2_PLACEMENT_3D('',#38806,#18237,#18238);
#14966=AXIS2_PLACEMENT_3D('',#38807,#18239,#18240);
#14967=AXIS2_PLACEMENT_3D('',#38808,#18241,#18242);
#14968=AXIS2_PLACEMENT_3D('',#38810,#18243,#18244);
#14969=AXIS2_PLACEMENT_3D('',#38811,#18245,#18246);
#14970=AXIS2_PLACEMENT_3D('',#38813,#18247,#18248);
#14971=AXIS2_PLACEMENT_3D('',#38815,#18249,#18250);
#14972=AXIS2_PLACEMENT_3D('',#38816,#18251,#18252);
#14973=AXIS2_PLACEMENT_3D('',#38818,#18253,#18254);
#14974=AXIS2_PLACEMENT_3D('',#38820,#18255,#18256);
#14975=AXIS2_PLACEMENT_3D('',#38821,#18257,#18258);
#14976=AXIS2_PLACEMENT_3D('',#38823,#18259,#18260);
#14977=AXIS2_PLACEMENT_3D('',#38825,#18261,#18262);
#14978=AXIS2_PLACEMENT_3D('',#39428,#18263,#18264);
#14979=AXIS2_PLACEMENT_3D('',#39429,#18265,#18266);
#14980=AXIS2_PLACEMENT_3D('',#39430,#18267,#18268);
#14981=AXIS2_PLACEMENT_3D('',#39431,#18269,#18270);
#14982=AXIS2_PLACEMENT_3D('',#39433,#18271,#18272);
#14983=AXIS2_PLACEMENT_3D('',#39434,#18273,#18274);
#14984=AXIS2_PLACEMENT_3D('',#39442,#18275,#18276);
#14985=AXIS2_PLACEMENT_3D('',#39444,#18277,#18278);
#14986=AXIS2_PLACEMENT_3D('',#39445,#18279,#18280);
#14987=AXIS2_PLACEMENT_3D('',#39446,#18281,#18282);
#14988=AXIS2_PLACEMENT_3D('',#39447,#18283,#18284);
#14989=AXIS2_PLACEMENT_3D('',#39448,#18285,#18286);
#14990=AXIS2_PLACEMENT_3D('',#39449,#18287,#18288);
#14991=AXIS2_PLACEMENT_3D('',#39451,#18289,#18290);
#14992=AXIS2_PLACEMENT_3D('',#39452,#18291,#18292);
#14993=AXIS2_PLACEMENT_3D('',#39453,#18293,#18294);
#14994=AXIS2_PLACEMENT_3D('',#39454,#18295,#18296);
#14995=AXIS2_PLACEMENT_3D('',#39455,#18297,#18298);
#14996=AXIS2_PLACEMENT_3D('',#39456,#18299,#18300);
#14997=AXIS2_PLACEMENT_3D('',#39458,#18302,#18303);
#14998=AXIS2_PLACEMENT_3D('',#39460,#18305,#18306);
#14999=AXIS2_PLACEMENT_3D('',#39461,#18307,#18308);
#15000=AXIS2_PLACEMENT_3D('',#39462,#18309,#18310);
#15001=AXIS2_PLACEMENT_3D('',#39463,#18311,#18312);
#15002=AXIS2_PLACEMENT_3D('',#39464,#18313,#18314);
#15003=AXIS2_PLACEMENT_3D('',#39469,#18316,#18317);
#15004=AXIS2_PLACEMENT_3D('',#39472,#18319,#18320);
#15005=AXIS2_PLACEMENT_3D('',#39478,#18324,#18325);
#15006=AXIS2_PLACEMENT_3D('',#39484,#18329,#18330);
#15007=AXIS2_PLACEMENT_3D('',#39485,#18331,#18332);
#15008=AXIS2_PLACEMENT_3D('',#39486,#18333,#18334);
#15009=AXIS2_PLACEMENT_3D('',#39487,#18335,#18336);
#15010=AXIS2_PLACEMENT_3D('',#39492,#18338,#18339);
#15011=AXIS2_PLACEMENT_3D('',#39495,#18341,#18342);
#15012=AXIS2_PLACEMENT_3D('',#39501,#18346,#18347);
#15013=AXIS2_PLACEMENT_3D('',#39507,#18351,#18352);
#15014=AXIS2_PLACEMENT_3D('',#39508,#18353,#18354);
#15015=AXIS2_PLACEMENT_3D('',#39509,#18355,#18356);
#15016=AXIS2_PLACEMENT_3D('',#39510,#18357,#18358);
#15017=AXIS2_PLACEMENT_3D('',#39515,#18360,#18361);
#15018=AXIS2_PLACEMENT_3D('',#39518,#18363,#18364);
#15019=AXIS2_PLACEMENT_3D('',#39524,#18368,#18369);
#15020=AXIS2_PLACEMENT_3D('',#39530,#18373,#18374);
#15021=AXIS2_PLACEMENT_3D('',#39531,#18375,#18376);
#15022=AXIS2_PLACEMENT_3D('',#39532,#18377,#18378);
#15023=AXIS2_PLACEMENT_3D('',#39533,#18379,#18380);
#15024=AXIS2_PLACEMENT_3D('',#39535,#18381,#18382);
#15025=AXIS2_PLACEMENT_3D('',#39537,#18383,#18384);
#15026=AXIS2_PLACEMENT_3D('',#39539,#18385,#18386);
#15027=AXIS2_PLACEMENT_3D('',#39541,#18387,#18388);
#15028=AXIS2_PLACEMENT_3D('',#39543,#18389,#18390);
#15029=AXIS2_PLACEMENT_3D('',#39544,#18391,#18392);
#15030=AXIS2_PLACEMENT_3D('',#39545,#18393,#18394);
#15031=AXIS2_PLACEMENT_3D('',#39546,#18395,#18396);
#15032=AXIS2_PLACEMENT_3D('',#39548,#18397,#18398);
#15033=AXIS2_PLACEMENT_3D('',#39549,#18399,#18400);
#15034=AXIS2_PLACEMENT_3D('',#39551,#18401,#18402);
#15035=AXIS2_PLACEMENT_3D('',#39553,#18403,#18404);
#15036=AXIS2_PLACEMENT_3D('',#39555,#18405,#18406);
#15037=AXIS2_PLACEMENT_3D('',#39557,#18407,#18408);
#15038=AXIS2_PLACEMENT_3D('',#39559,#18409,#18410);
#15039=AXIS2_PLACEMENT_3D('',#39561,#18411,#18412);
#15040=AXIS2_PLACEMENT_3D('',#39562,#18413,#18414);
#15041=AXIS2_PLACEMENT_3D('',#39563,#18415,#18416);
#15042=AXIS2_PLACEMENT_3D('',#39564,#18417,#18418);
#15043=AXIS2_PLACEMENT_3D('',#39565,#18419,#18420);
#15044=AXIS2_PLACEMENT_3D('',#39566,#18421,#18422);
#15045=AXIS2_PLACEMENT_3D('',#39567,#18423,#18424);
#15046=AXIS2_PLACEMENT_3D('',#39568,#18425,#18426);
#15047=AXIS2_PLACEMENT_3D('',#39569,#18427,#18428);
#15048=AXIS2_PLACEMENT_3D('',#39570,#18429,#18430);
#15049=AXIS2_PLACEMENT_3D('',#40821,#18437,#18438);
#15050=AXIS2_PLACEMENT_3D('',#40823,#18440,#18441);
#15051=AXIS2_PLACEMENT_3D('',#40825,#18443,#18444);
#15052=AXIS2_PLACEMENT_3D('',#40834,#18449,#18450);
#15053=AXIS2_PLACEMENT_3D('',#40840,#18454,#18455);
#15054=AXIS2_PLACEMENT_3D('',#40846,#18459,#18460);
#15055=AXIS2_PLACEMENT_3D('',#40855,#18465,#18466);
#15056=AXIS2_PLACEMENT_3D('',#40861,#18470,#18471);
#15057=AXIS2_PLACEMENT_3D('',#40867,#18475,#18476);
#15058=AXIS2_PLACEMENT_3D('',#40876,#18481,#18482);
#15059=AXIS2_PLACEMENT_3D('',#40882,#18486,#18487);
#15060=AXIS2_PLACEMENT_3D('',#40888,#18491,#18492);
#15061=AXIS2_PLACEMENT_3D('',#40897,#18497,#18498);
#15062=AXIS2_PLACEMENT_3D('',#40903,#18502,#18503);
#15063=AXIS2_PLACEMENT_3D('',#40909,#18507,#18508);
#15064=AXIS2_PLACEMENT_3D('',#40918,#18513,#18514);
#15065=AXIS2_PLACEMENT_3D('',#40924,#18518,#18519);
#15066=AXIS2_PLACEMENT_3D('',#40930,#18523,#18524);
#15067=AXIS2_PLACEMENT_3D('',#40939,#18529,#18530);
#15068=AXIS2_PLACEMENT_3D('',#40945,#18534,#18535);
#15069=AXIS2_PLACEMENT_3D('',#40951,#18539,#18540);
#15070=AXIS2_PLACEMENT_3D('',#40960,#18545,#18546);
#15071=AXIS2_PLACEMENT_3D('',#40966,#18550,#18551);
#15072=AXIS2_PLACEMENT_3D('',#40972,#18555,#18556);
#15073=AXIS2_PLACEMENT_3D('',#40981,#18561,#18562);
#15074=AXIS2_PLACEMENT_3D('',#40987,#18566,#18567);
#15075=AXIS2_PLACEMENT_3D('',#40993,#18571,#18572);
#15076=AXIS2_PLACEMENT_3D('',#41002,#18577,#18578);
#15077=AXIS2_PLACEMENT_3D('',#41008,#18582,#18583);
#15078=AXIS2_PLACEMENT_3D('',#41014,#18587,#18588);
#15079=AXIS2_PLACEMENT_3D('',#41023,#18593,#18594);
#15080=AXIS2_PLACEMENT_3D('',#41029,#18598,#18599);
#15081=AXIS2_PLACEMENT_3D('',#41035,#18603,#18604);
#15082=AXIS2_PLACEMENT_3D('',#41044,#18609,#18610);
#15083=AXIS2_PLACEMENT_3D('',#41050,#18614,#18615);
#15084=AXIS2_PLACEMENT_3D('',#41056,#18619,#18620);
#15085=AXIS2_PLACEMENT_3D('',#41057,#18621,#18622);
#15086=AXIS2_PLACEMENT_3D('',#41058,#18623,#18624);
#15087=AXIS2_PLACEMENT_3D('',#41059,#18625,#18626);
#15088=AXIS2_PLACEMENT_3D('',#41060,#18627,#18628);
#15089=AXIS2_PLACEMENT_3D('',#41061,#18629,#18630);
#15090=AXIS2_PLACEMENT_3D('',#41062,#18631,#18632);
#15091=AXIS2_PLACEMENT_3D('',#41063,#18633,#18634);
#15092=AXIS2_PLACEMENT_3D('',#41064,#18635,#18636);
#15093=AXIS2_PLACEMENT_3D('',#41065,#18637,#18638);
#15094=AXIS2_PLACEMENT_3D('',#41066,#18639,#18640);
#15095=AXIS2_PLACEMENT_3D('',#41067,#18641,#18642);
#15096=AXIS2_PLACEMENT_3D('',#41068,#18643,#18644);
#15097=AXIS2_PLACEMENT_3D('',#41070,#18645,#18646);
#15098=AXIS2_PLACEMENT_3D('',#41071,#18647,#18648);
#15099=AXIS2_PLACEMENT_3D('',#41072,#18649,#18650);
#15100=AXIS2_PLACEMENT_3D('',#41073,#18651,#18652);
#15101=AXIS2_PLACEMENT_3D('',#41074,#18653,#18654);
#15102=AXIS2_PLACEMENT_3D('',#41075,#18655,#18656);
#15103=AXIS2_PLACEMENT_3D('',#41076,#18657,#18658);
#15104=AXIS2_PLACEMENT_3D('',#41077,#18659,#18660);
#15105=AXIS2_PLACEMENT_3D('',#41078,#18661,#18662);
#15106=AXIS2_PLACEMENT_3D('',#41079,#18663,#18664);
#15107=AXIS2_PLACEMENT_3D('',#41080,#18665,#18666);
#15108=AXIS2_PLACEMENT_3D('',#41081,#18667,#18668);
#15109=AXIS2_PLACEMENT_3D('',#41082,#18669,#18670);
#15110=AXIS2_PLACEMENT_3D('',#41083,#18671,#18672);
#15111=AXIS2_PLACEMENT_3D('',#41084,#18673,#18674);
#15112=AXIS2_PLACEMENT_3D('',#41085,#18675,#18676);
#15113=AXIS2_PLACEMENT_3D('',#41087,#18677,#18678);
#15114=AXIS2_PLACEMENT_3D('',#41089,#18679,#18680);
#15115=AXIS2_PLACEMENT_3D('',#41090,#18681,#18682);
#15116=AXIS2_PLACEMENT_3D('',#41091,#18683,#18684);
#15117=AXIS2_PLACEMENT_3D('',#41092,#18685,#18686);
#15118=AXIS2_PLACEMENT_3D('',#41093,#18687,#18688);
#15119=AXIS2_PLACEMENT_3D('',#41094,#18689,#18690);
#15120=AXIS2_PLACEMENT_3D('',#41095,#18691,#18692);
#15121=AXIS2_PLACEMENT_3D('',#41096,#18693,#18694);
#15122=AXIS2_PLACEMENT_3D('',#41097,#18695,#18696);
#15123=AXIS2_PLACEMENT_3D('',#41098,#18697,#18698);
#15124=AXIS2_PLACEMENT_3D('',#41099,#18699,#18700);
#15125=AXIS2_PLACEMENT_3D('',#41100,#18701,#18702);
#15126=AXIS2_PLACEMENT_3D('',#41101,#18703,#18704);
#15127=AXIS2_PLACEMENT_3D('',#41102,#18705,#18706);
#15128=AXIS2_PLACEMENT_3D('',#41103,#18707,#18708);
#15129=AXIS2_PLACEMENT_3D('',#41104,#18709,#18710);
#15130=AXIS2_PLACEMENT_3D('',#41107,#18711,#18712);
#15131=AXIS2_PLACEMENT_3D('',#41109,#18713,#18714);
#15132=AXIS2_PLACEMENT_3D('',#41111,#18715,#18716);
#15133=AXIS2_PLACEMENT_3D('',#41112,#18717,#18718);
#15134=AXIS2_PLACEMENT_3D('',#41113,#18719,#18720);
#15135=AXIS2_PLACEMENT_3D('',#41118,#18723,#18724);
#15136=AXIS2_PLACEMENT_3D('',#41119,#18725,#18726);
#15137=AXIS2_PLACEMENT_3D('',#41124,#18729,#18730);
#15138=AXIS2_PLACEMENT_3D('',#41125,#18731,#18732);
#15139=AXIS2_PLACEMENT_3D('',#41128,#18733,#18734);
#15140=AXIS2_PLACEMENT_3D('',#41130,#18735,#18736);
#15141=AXIS2_PLACEMENT_3D('',#41132,#18737,#18738);
#15142=AXIS2_PLACEMENT_3D('',#41133,#18739,#18740);
#15143=AXIS2_PLACEMENT_3D('',#41134,#18741,#18742);
#15144=AXIS2_PLACEMENT_3D('',#41139,#18745,#18746);
#15145=AXIS2_PLACEMENT_3D('',#41140,#18747,#18748);
#15146=AXIS2_PLACEMENT_3D('',#41145,#18751,#18752);
#15147=AXIS2_PLACEMENT_3D('',#41149,#18754,#18755);
#15148=AXIS2_PLACEMENT_3D('',#41151,#18756,#18757);
#15149=AXIS2_PLACEMENT_3D('',#41153,#18758,#18759);
#15150=AXIS2_PLACEMENT_3D('',#41157,#18761,#18762);
#15151=AXIS2_PLACEMENT_3D('',#41718,#18767,#18768);
#15152=AXIS2_PLACEMENT_3D('',#41721,#18771,#18772);
#15153=AXIS2_PLACEMENT_3D('',#41723,#18774,#18775);
#15154=AXIS2_PLACEMENT_3D('',#41725,#18777,#18778);
#15155=AXIS2_PLACEMENT_3D('',#41729,#18780,#18781);
#15156=AXIS2_PLACEMENT_3D('',#41733,#18783,#18784);
#15157=AXIS2_PLACEMENT_3D('',#41734,#18785,#18786);
#15158=AXIS2_PLACEMENT_3D('',#41735,#18787,#18788);
#15159=AXIS2_PLACEMENT_3D('',#41737,#18789,#18790);
#15160=AXIS2_PLACEMENT_3D('',#41739,#18791,#18792);
#15161=AXIS2_PLACEMENT_3D('',#41742,#18794,#18795);
#15162=AXIS2_PLACEMENT_3D('',#41747,#18798,#18799);
#15163=AXIS2_PLACEMENT_3D('',#41750,#18801,#18802);
#15164=AXIS2_PLACEMENT_3D('',#41751,#18803,#18804);
#15165=AXIS2_PLACEMENT_3D('',#41753,#18805,#18806);
#15166=AXIS2_PLACEMENT_3D('',#41757,#18808,#18809);
#15167=AXIS2_PLACEMENT_3D('',#41760,#18811,#18812);
#15168=AXIS2_PLACEMENT_3D('',#41762,#18814,#18815);
#15169=AXIS2_PLACEMENT_3D('',#41764,#18817,#18818);
#15170=AXIS2_PLACEMENT_3D('',#41765,#18819,#18820);
#15171=AXIS2_PLACEMENT_3D('',#41766,#18821,#18822);
#15172=AXIS2_PLACEMENT_3D('',#41767,#18823,#18824);
#15173=AXIS2_PLACEMENT_3D('',#41768,#18825,#18826);
#15174=AXIS2_PLACEMENT_3D('',#41769,#18827,#18828);
#15175=AXIS2_PLACEMENT_3D('',#41770,#18829,#18830);
#15176=AXIS2_PLACEMENT_3D('',#41771,#18831,#18832);
#15177=AXIS2_PLACEMENT_3D('',#41772,#18833,#18834);
#15178=AXIS2_PLACEMENT_3D('',#41773,#18835,#18836);
#15179=AXIS2_PLACEMENT_3D('',#41774,#18837,#18838);
#15180=AXIS2_PLACEMENT_3D('',#41780,#18839,#18840);
#15181=AXIS2_PLACEMENT_3D('',#41781,#18841,#18842);
#15182=AXIS2_PLACEMENT_3D('',#41782,#18843,#18844);
#15183=AXIS2_PLACEMENT_3D('',#41784,#18845,#18846);
#15184=AXIS2_PLACEMENT_3D('',#41785,#18847,#18848);
#15185=AXIS2_PLACEMENT_3D('',#41786,#18849,#18850);
#15186=AXIS2_PLACEMENT_3D('',#41787,#18851,#18852);
#15187=AXIS2_PLACEMENT_3D('',#41788,#18853,#18854);
#15188=AXIS2_PLACEMENT_3D('',#41789,#18855,#18856);
#15189=AXIS2_PLACEMENT_3D('',#41790,#18857,#18858);
#15190=AXIS2_PLACEMENT_3D('',#41791,#18859,#18860);
#15191=AXIS2_PLACEMENT_3D('',#41802,#18866,#18867);
#15192=AXIS2_PLACEMENT_3D('',#41803,#18868,#18869);
#15193=AXIS2_PLACEMENT_3D('',#41807,#18871,#18872);
#15194=AXIS2_PLACEMENT_3D('',#41808,#18873,#18874);
#15195=AXIS2_PLACEMENT_3D('',#41816,#18879,#18880);
#15196=AXIS2_PLACEMENT_3D('',#41817,#18881,#18882);
#15197=AXIS2_PLACEMENT_3D('',#41818,#18883,#18884);
#15198=AXIS2_PLACEMENT_3D('',#41819,#18885,#18886);
#15199=AXIS2_PLACEMENT_3D('',#41830,#18892,#18893);
#15200=AXIS2_PLACEMENT_3D('',#41831,#18894,#18895);
#15201=AXIS2_PLACEMENT_3D('',#41835,#18897,#18898);
#15202=AXIS2_PLACEMENT_3D('',#41836,#18899,#18900);
#15203=AXIS2_PLACEMENT_3D('',#41844,#18905,#18906);
#15204=AXIS2_PLACEMENT_3D('',#41845,#18907,#18908);
#15205=AXIS2_PLACEMENT_3D('',#41846,#18909,#18910);
#15206=AXIS2_PLACEMENT_3D('',#41847,#18911,#18912);
#15207=AXIS2_PLACEMENT_3D('',#41858,#18918,#18919);
#15208=AXIS2_PLACEMENT_3D('',#41859,#18920,#18921);
#15209=AXIS2_PLACEMENT_3D('',#41863,#18923,#18924);
#15210=AXIS2_PLACEMENT_3D('',#41864,#18925,#18926);
#15211=AXIS2_PLACEMENT_3D('',#41872,#18931,#18932);
#15212=AXIS2_PLACEMENT_3D('',#41873,#18933,#18934);
#15213=AXIS2_PLACEMENT_3D('',#41874,#18935,#18936);
#15214=AXIS2_PLACEMENT_3D('',#41875,#18937,#18938);
#15215=AXIS2_PLACEMENT_3D('',#41886,#18944,#18945);
#15216=AXIS2_PLACEMENT_3D('',#41887,#18946,#18947);
#15217=AXIS2_PLACEMENT_3D('',#41891,#18949,#18950);
#15218=AXIS2_PLACEMENT_3D('',#41892,#18951,#18952);
#15219=AXIS2_PLACEMENT_3D('',#41900,#18957,#18958);
#15220=AXIS2_PLACEMENT_3D('',#41901,#18959,#18960);
#15221=AXIS2_PLACEMENT_3D('',#41902,#18961,#18962);
#15222=AXIS2_PLACEMENT_3D('',#41903,#18963,#18964);
#15223=AXIS2_PLACEMENT_3D('',#41904,#18965,#18966);
#15224=AXIS2_PLACEMENT_3D('',#41906,#18967,#18968);
#15225=AXIS2_PLACEMENT_3D('',#41907,#18969,#18970);
#15226=AXIS2_PLACEMENT_3D('',#41908,#18971,#18972);
#15227=AXIS2_PLACEMENT_3D('',#41909,#18973,#18974);
#15228=AXIS2_PLACEMENT_3D('',#41910,#18975,#18976);
#15229=AXIS2_PLACEMENT_3D('',#41911,#18977,#18978);
#15230=AXIS2_PLACEMENT_3D('',#41913,#18979,#18980);
#15231=AXIS2_PLACEMENT_3D('',#41914,#18981,#18982);
#15232=AXIS2_PLACEMENT_3D('',#41915,#18983,#18984);
#15233=AXIS2_PLACEMENT_3D('',#41916,#18985,#18986);
#15234=AXIS2_PLACEMENT_3D('',#41917,#18987,#18988);
#15235=AXIS2_PLACEMENT_3D('',#41918,#18989,#18990);
#15236=AXIS2_PLACEMENT_3D('',#41920,#18991,#18992);
#15237=AXIS2_PLACEMENT_3D('',#41921,#18993,#18994);
#15238=AXIS2_PLACEMENT_3D('',#41922,#18995,#18996);
#15239=AXIS2_PLACEMENT_3D('',#41923,#18997,#18998);
#15240=AXIS2_PLACEMENT_3D('',#41924,#18999,#19000);
#15241=AXIS2_PLACEMENT_3D('',#41925,#19001,#19002);
#15242=AXIS2_PLACEMENT_3D('',#41926,#19003,#19004);
#15243=AXIS2_PLACEMENT_3D('',#41927,#19005,#19006);
#15244=AXIS2_PLACEMENT_3D('',#41928,#19007,#19008);
#15245=AXIS2_PLACEMENT_3D('',#41929,#19009,#19010);
#15246=AXIS2_PLACEMENT_3D('',#41931,#19011,#19012);
#15247=AXIS2_PLACEMENT_3D('',#41932,#19013,#19014);
#15248=AXIS2_PLACEMENT_3D('',#41933,#19015,#19016);
#15249=AXIS2_PLACEMENT_3D('',#41934,#19017,#19018);
#15250=AXIS2_PLACEMENT_3D('',#41935,#19019,#19020);
#15251=AXIS2_PLACEMENT_3D('',#41936,#19021,#19022);
#15252=AXIS2_PLACEMENT_3D('',#41937,#19023,#19024);
#15253=AXIS2_PLACEMENT_3D('',#41938,#19025,#19026);
#15254=AXIS2_PLACEMENT_3D('',#41939,#19027,#19028);
#15255=AXIS2_PLACEMENT_3D('',#41940,#19029,#19030);
#15256=AXIS2_PLACEMENT_3D('',#41942,#19031,#19032);
#15257=AXIS2_PLACEMENT_3D('',#41943,#19033,#19034);
#15258=AXIS2_PLACEMENT_3D('',#41944,#19035,#19036);
#15259=AXIS2_PLACEMENT_3D('',#41976,#19037,#19038);
#15260=AXIS2_PLACEMENT_3D('',#41991,#19039,#19040);
#15261=AXIS2_PLACEMENT_3D('',#42098,#19041,#19042);
#15262=AXIS2_PLACEMENT_3D('',#42142,#19043,#19044);
#15263=AXIS2_PLACEMENT_3D('',#42179,#19045,#19046);
#15264=AXIS2_PLACEMENT_3D('',#42199,#19047,#19048);
#15265=AXIS2_PLACEMENT_3D('',#42275,#19049,#19050);
#15266=AXIS2_PLACEMENT_3D('',#42319,#19051,#19052);
#15267=AXIS2_PLACEMENT_3D('',#43543,#19053,#19054);
#15268=AXIS2_PLACEMENT_3D('',#43557,#19055,#19056);
#15269=AXIS2_PLACEMENT_3D('',#44803,#19057,#19058);
#15270=AXIS2_PLACEMENT_3D('',#44804,#19059,#19060);
#15271=AXIS2_PLACEMENT_3D('',#44806,#19061,#19062);
#15272=AXIS2_PLACEMENT_3D('',#44808,#19063,#19064);
#15273=AXIS2_PLACEMENT_3D('',#44809,#19065,#19066);
#15274=AXIS2_PLACEMENT_3D('',#44811,#19067,#19068);
#15275=AXIS2_PLACEMENT_3D('',#44813,#19069,#19070);
#15276=AXIS2_PLACEMENT_3D('',#44814,#19071,#19072);
#15277=AXIS2_PLACEMENT_3D('',#44816,#19073,#19074);
#15278=AXIS2_PLACEMENT_3D('',#44866,#19075,#19076);
#15279=AXIS2_PLACEMENT_3D('',#44867,#19077,#19078);
#15280=AXIS2_PLACEMENT_3D('',#44869,#19079,#19080);
#15281=AXIS2_PLACEMENT_3D('',#44871,#19081,#19082);
#15282=AXIS2_PLACEMENT_3D('',#44872,#19083,#19084);
#15283=AXIS2_PLACEMENT_3D('',#44874,#19085,#19086);
#15284=AXIS2_PLACEMENT_3D('',#44875,#19087,#19088);
#15285=AXIS2_PLACEMENT_3D('',#45451,#19089,#19090);
#15286=AXIS2_PLACEMENT_3D('',#45452,#19091,#19092);
#15287=AXIS2_PLACEMENT_3D('',#45453,#19093,#19094);
#15288=AXIS2_PLACEMENT_3D('',#45454,#19095,#19096);
#15289=AXIS2_PLACEMENT_3D('',#45455,#19097,#19098);
#15290=AXIS2_PLACEMENT_3D('',#45456,#19099,#19100);
#15291=AXIS2_PLACEMENT_3D('',#45457,#19101,#19102);
#15292=AXIS2_PLACEMENT_3D('',#45459,#19103,#19104);
#15293=AXIS2_PLACEMENT_3D('',#45461,#19105,#19106);
#15294=AXIS2_PLACEMENT_3D('',#45462,#19107,#19108);
#15295=DIRECTION('',(0.,0.,1.));
#15296=DIRECTION('',(1.,0.,0.));
#15297=DIRECTION('',(0.866025403784438,0.,-0.5));
#15298=DIRECTION('',(0.866025403784438,1.0605752387249E-16,0.5));
#15299=DIRECTION('',(0.,0.,1.));
#15300=DIRECTION('',(1.,0.,0.));
#15301=DIRECTION('',(0.,0.,-1.));
#15302=DIRECTION('',(0.,0.,1.));
#15303=DIRECTION('',(0.,1.,0.));
#15304=DIRECTION('',(-1.,0.,0.));
#15305=DIRECTION('',(0.,0.,-1.));
#15306=DIRECTION('',(-0.866025403784438,-1.0605752387249E-16,0.5));
#15307=DIRECTION('',(-0.866025403784438,0.,-0.5));
#15308=DIRECTION('',(0.,1.,0.));
#15309=DIRECTION('',(-1.,0.,0.));
#15310=DIRECTION('',(0.,0.,1.));
#15311=DIRECTION('',(-1.,0.,0.));
#15312=DIRECTION('',(0.,0.,-1.));
#15313=DIRECTION('',(-1.,0.,0.));
#15314=DIRECTION('',(0.,0.,1.));
#15315=DIRECTION('',(-1.,0.,0.));
#15316=DIRECTION('',(0.,0.,1.));
#15317=DIRECTION('',(1.,0.,0.));
#15318=DIRECTION('',(0.,0.,1.));
#15319=DIRECTION('',(1.,0.,0.));
#15320=DIRECTION('',(0.,0.,1.));
#15321=DIRECTION('',(1.,0.,0.));
#15322=DIRECTION('',(0.,0.,1.));
#15323=DIRECTION('',(1.,0.,0.));
#15324=DIRECTION('',(0.,0.,1.));
#15325=DIRECTION('',(1.,0.,0.));
#15326=DIRECTION('',(0.,0.,-1.));
#15327=DIRECTION('',(1.,0.,0.));
#15328=DIRECTION('',(0.,0.,1.));
#15329=DIRECTION('',(1.,0.,0.));
#15330=DIRECTION('',(0.,0.,-1.));
#15331=DIRECTION('',(1.,0.,0.));
#15332=DIRECTION('',(0.,0.,1.));
#15333=DIRECTION('',(1.,0.,0.));
#15334=DIRECTION('',(0.86602540378444,-0.5,0.));
#15335=DIRECTION('',(0.5,0.86602540378444,0.));
#15336=DIRECTION('',(0.5,0.86602540378444,0.));
#15337=DIRECTION('',(0.,0.,1.));
#15338=DIRECTION('',(0.5,0.86602540378444,0.));
#15339=DIRECTION('',(0.,0.,1.));
#15340=DIRECTION('',(-0.86602540378444,0.5,0.));
#15341=DIRECTION('',(-0.5,-0.86602540378444,0.));
#15342=DIRECTION('',(-0.5,-0.86602540378444,0.));
#15343=DIRECTION('',(0.,0.,1.));
#15344=DIRECTION('',(-0.5,-0.86602540378444,0.));
#15345=DIRECTION('',(0.,0.,1.));
#15346=DIRECTION('',(0.,0.,1.));
#15347=DIRECTION('',(-0.5,0.866025403784436,0.));
#15348=DIRECTION('',(0.,0.,1.));
#15349=DIRECTION('',(-0.5,0.866025403784436,0.));
#15350=DIRECTION('',(0.,0.,1.));
#15351=DIRECTION('',(-0.5,0.866025403784436,0.));
#15352=DIRECTION('',(0.,1.,0.));
#15353=DIRECTION('',(-1.,0.,0.));
#15354=DIRECTION('',(-1.,-6.60582699651968E-15,0.));
#15355=DIRECTION('',(0.,0.,1.));
#15356=DIRECTION('',(-1.,-6.60582699651968E-15,0.));
#15357=DIRECTION('',(0.,0.,1.));
#15358=DIRECTION('',(0.,-1.,0.));
#15359=DIRECTION('',(1.,0.,0.));
#15360=DIRECTION('',(1.,7.105427357601E-15,0.));
#15361=DIRECTION('',(0.,0.,1.));
#15362=DIRECTION('',(1.,7.105427357601E-15,0.));
#15363=DIRECTION('',(0.,0.,1.));
#15364=DIRECTION('',(0.,0.,1.));
#15365=DIRECTION('',(-0.499999999999993,-0.866025403784443,0.));
#15366=DIRECTION('',(0.,0.,1.));
#15367=DIRECTION('',(-0.499999999999993,-0.866025403784443,0.));
#15368=DIRECTION('',(0.,0.,1.));
#15369=DIRECTION('',(-0.499999999999993,-0.866025403784443,0.));
#15370=DIRECTION('',(-0.86602540378444,-0.5,0.));
#15371=DIRECTION('',(0.5,-0.86602540378444,0.));
#15372=DIRECTION('',(0.5,-0.86602540378444,0.));
#15373=DIRECTION('',(0.,0.,1.));
#15374=DIRECTION('',(0.5,-0.86602540378444,0.));
#15375=DIRECTION('',(0.,0.,1.));
#15376=DIRECTION('',(0.86602540378444,0.5,0.));
#15377=DIRECTION('',(-0.5,0.86602540378444,0.));
#15378=DIRECTION('',(-0.5,0.86602540378444,0.));
#15379=DIRECTION('',(0.,0.,1.));
#15380=DIRECTION('',(-0.5,0.86602540378444,0.));
#15381=DIRECTION('',(0.,0.,1.));
#15382=DIRECTION('',(0.,0.,1.));
#15383=DIRECTION('',(1.,0.,0.));
#15384=DIRECTION('',(0.,0.,1.));
#15385=DIRECTION('',(1.,0.,0.));
#15386=DIRECTION('',(0.,0.,1.));
#15387=DIRECTION('',(1.,0.,0.));
#15388=DIRECTION('',(0.,0.,-1.));
#15389=DIRECTION('',(-1.04744440165294E-14,1.,0.));
#15390=DIRECTION('',(0.,0.,1.));
#15391=DIRECTION('',(-3.49148133884314E-15,1.,0.));
#15392=DIRECTION('',(0.,0.,1.));
#15393=DIRECTION('',(-3.49148133884314E-15,1.,0.));
#15394=DIRECTION('',(0.,0.,-1.));
#15395=DIRECTION('',(-1.04744440165294E-14,1.,0.));
#15396=DIRECTION('',(0.,0.,1.));
#15397=DIRECTION('',(-1.,0.,0.));
#15398=DIRECTION('',(0.,0.,1.));
#15399=DIRECTION('',(-1.,0.,0.));
#15400=DIRECTION('',(0.,0.,-1.));
#15401=DIRECTION('',(-1.04744440165294E-14,1.,0.));
#15402=DIRECTION('',(0.,0.,1.));
#15403=DIRECTION('',(1.04744440165294E-14,-1.,0.));
#15404=DIRECTION('',(0.,0.,1.));
#15405=DIRECTION('',(1.04744440165294E-14,-1.,0.));
#15406=DIRECTION('',(0.,0.,-1.));
#15407=DIRECTION('',(-1.04744440165294E-14,1.,0.));
#15408=DIRECTION('',(0.,0.,1.));
#15409=DIRECTION('',(1.,0.,0.));
#15410=DIRECTION('',(0.,0.,1.));
#15411=DIRECTION('',(1.,0.,0.));
#15412=DIRECTION('',(0.,0.,1.));
#15413=DIRECTION('',(1.,0.,0.));
#15414=DIRECTION('',(0.,0.,1.));
#15415=DIRECTION('',(1.,0.,0.));
#15416=DIRECTION('',(0.,0.,1.));
#15417=DIRECTION('',(1.,0.,0.));
#15418=DIRECTION('',(0.,0.,1.));
#15419=DIRECTION('',(1.,0.,0.));
#15420=DIRECTION('',(0.,0.,1.));
#15421=DIRECTION('',(1.,0.,0.));
#15422=DIRECTION('',(0.,0.,1.));
#15423=DIRECTION('',(1.,0.,0.));
#15424=DIRECTION('',(0.,0.,1.));
#15425=DIRECTION('',(1.,0.,0.));
#15426=DIRECTION('',(0.,0.,1.));
#15427=DIRECTION('',(1.04744440165294E-14,-1.,0.));
#15428=DIRECTION('',(0.,0.,1.));
#15429=DIRECTION('',(-1.,0.,0.));
#15430=DIRECTION('',(0.,0.,1.));
#15431=DIRECTION('',(-3.49148133884314E-15,1.,0.));
#15432=DIRECTION('',(0.,0.,1.));
#15433=DIRECTION('',(1.,0.,0.));
#15434=DIRECTION('',(0.,0.,1.));
#15435=DIRECTION('',(-0.499999999999993,-0.866025403784443,0.));
#15436=DIRECTION('',(0.,0.,1.));
#15437=DIRECTION('',(-0.5,0.866025403784436,0.));
#15438=DIRECTION('',(0.,0.,-1.));
#15439=DIRECTION('',(1.,0.,0.));
#15440=DIRECTION('',(0.,0.,1.));
#15441=DIRECTION('',(1.,0.,0.));
#15442=DIRECTION('',(0.,0.,1.));
#15443=DIRECTION('',(1.,0.,0.));
#15444=DIRECTION('',(0.,0.,1.));
#15445=DIRECTION('',(1.,0.,0.));
#15446=DIRECTION('',(0.,0.,1.));
#15447=DIRECTION('',(1.,0.,0.));
#15448=DIRECTION('',(0.,0.,-1.));
#15449=DIRECTION('',(1.,0.,0.));
#15450=DIRECTION('',(0.,0.,1.));
#15451=DIRECTION('',(1.,0.,0.));
#15452=DIRECTION('',(0.,0.,1.));
#15453=DIRECTION('',(1.,0.,0.));
#15454=DIRECTION('',(0.,0.,1.));
#15455=DIRECTION('',(1.04744440165294E-14,-1.,0.));
#15456=DIRECTION('',(0.,0.,1.));
#15457=DIRECTION('',(-1.,0.,0.));
#15458=DIRECTION('',(0.,0.,1.));
#15459=DIRECTION('',(-3.49148133884314E-15,1.,0.));
#15460=DIRECTION('',(0.,0.,1.));
#15461=DIRECTION('',(1.,0.,0.));
#15462=DIRECTION('',(0.,0.,1.));
#15463=DIRECTION('',(-0.499999999999993,-0.866025403784443,0.));
#15464=DIRECTION('',(0.,0.,1.));
#15465=DIRECTION('',(-0.5,0.866025403784436,0.));
#15466=DIRECTION('',(0.,0.,-1.));
#15467=DIRECTION('',(1.,0.,0.));
#15468=DIRECTION('',(0.,0.,1.));
#15469=DIRECTION('',(1.,0.,0.));
#15470=DIRECTION('',(0.,0.,1.));
#15471=DIRECTION('',(1.,0.,0.));
#15472=DIRECTION('',(0.,0.,1.));
#15473=DIRECTION('',(1.,0.,0.));
#15474=DIRECTION('',(0.,0.,1.));
#15475=DIRECTION('',(1.,0.,0.));
#15476=DIRECTION('',(0.,0.,1.));
#15477=DIRECTION('',(1.,0.,0.));
#15478=DIRECTION('',(0.,0.,1.));
#15479=DIRECTION('',(1.,0.,0.));
#15480=DIRECTION('',(0.,0.,1.));
#15481=DIRECTION('',(1.,0.,0.));
#15482=DIRECTION('',(0.,0.,-1.));
#15483=DIRECTION('',(1.,0.,0.));
#15484=DIRECTION('',(0.,0.,1.));
#15485=DIRECTION('',(1.,0.,0.));
#15486=DIRECTION('',(0.,0.,1.));
#15487=DIRECTION('',(1.,0.,0.));
#15488=DIRECTION('',(0.,0.,1.));
#15489=DIRECTION('',(1.,0.,0.));
#15490=DIRECTION('',(0.,0.,-1.));
#15491=DIRECTION('',(-1.,0.,0.));
#15492=DIRECTION('',(0.,0.,-1.));
#15493=DIRECTION('',(-1.,0.,0.));
#15494=DIRECTION('',(0.,0.,-1.));
#15495=DIRECTION('',(-1.,0.,0.));
#15496=DIRECTION('',(0.,0.,-1.));
#15497=DIRECTION('',(-1.,0.,0.));
#15498=DIRECTION('',(0.,0.,1.));
#15499=DIRECTION('',(1.,0.,0.));
#15500=DIRECTION('',(0.,0.,1.));
#15501=DIRECTION('',(1.,0.,0.));
#15502=DIRECTION('',(0.,0.,1.));
#15503=DIRECTION('',(1.04744440165294E-14,-1.,0.));
#15504=DIRECTION('',(0.,0.,1.));
#15505=DIRECTION('',(1.04744440165294E-14,-1.,0.));
#15506=DIRECTION('',(0.,0.,1.));
#15507=DIRECTION('',(-1.,0.,0.));
#15508=DIRECTION('',(0.,0.,1.));
#15509=DIRECTION('',(-1.,0.,0.));
#15510=DIRECTION('',(0.,0.,1.));
#15511=DIRECTION('',(-3.49148133884314E-15,1.,0.));
#15512=DIRECTION('',(0.,0.,1.));
#15513=DIRECTION('',(-3.49148133884314E-15,1.,0.));
#15514=DIRECTION('',(0.,0.,1.));
#15515=DIRECTION('',(1.,0.,0.));
#15516=DIRECTION('',(0.,0.,1.));
#15517=DIRECTION('',(-0.499999999999993,-0.866025403784443,0.));
#15518=DIRECTION('',(0.,0.,1.));
#15519=DIRECTION('',(-0.5,0.866025403784436,0.));
#15520=DIRECTION('',(0.,0.,-1.));
#15521=DIRECTION('',(-1.,0.,0.));
#15522=DIRECTION('',(0.,0.,1.));
#15523=DIRECTION('',(1.,0.,0.));
#15524=DIRECTION('',(0.,0.,1.));
#15525=DIRECTION('',(1.,0.,0.));
#15526=DIRECTION('',(0.,0.,1.));
#15527=DIRECTION('',(1.,0.,0.));
#15528=DIRECTION('',(0.,0.,1.));
#15529=DIRECTION('',(1.,0.,0.));
#15530=DIRECTION('',(0.,0.,1.));
#15531=DIRECTION('',(1.,0.,0.));
#15532=DIRECTION('',(0.,0.,1.));
#15533=DIRECTION('',(1.,0.,0.));
#15534=DIRECTION('',(4.16495833440966E-16,0.,1.));
#15535=DIRECTION('',(1.,0.,0.));
#15536=DIRECTION('',(4.16495833440966E-16,0.,1.));
#15537=DIRECTION('',(1.,0.,0.));
#15538=DIRECTION('',(0.,0.,-1.));
#15539=DIRECTION('',(-1.,0.,0.));
#15540=DIRECTION('',(-4.16495833440966E-16,0.,-1.));
#15541=DIRECTION('',(-1.,0.,0.));
#15542=DIRECTION('',(-4.16495833440966E-16,0.,-1.));
#15543=DIRECTION('',(-1.,0.,0.));
#15544=DIRECTION('',(0.86602540378444,0.,-0.5));
#15545=DIRECTION('',(0.493314209934358,-0.711787250712482,0.500000000000007));
#15546=DIRECTION('',(-0.493314209934064,0.711787250712696,-0.499999999999992));
#15547=DIRECTION('',(0.0139418328291082,0.0429085493761317,-0.998981722399265));
#15548=DIRECTION('',(0.999902807845662,-0.000610909849002805,0.0139284475630859));
#15549=DIRECTION('',(-0.86602540378444,0.,-0.5));
#15550=DIRECTION('',(-0.493317861910604,0.711784820259979,0.4999998567674));
#15551=DIRECTION('',(1.5963568800503E-17,-8.85021464712618E-18,-1.));
#15552=DIRECTION('',(-1.,0.,-1.5963568800503E-17));
#15553=DIRECTION('',(0.,0.,-1.));
#15554=DIRECTION('',(4.89971376945695E-6,3.39581651649945E-6,0.999999999982231));
#15555=DIRECTION('',(0.821901121609115,0.569630183801455,0.));
#15556=DIRECTION('',(-0.569630183801455,0.821901121609115,0.));
#15557=DIRECTION('',(0.,0.,-1.));
#15558=DIRECTION('',(0.821901121609115,0.569630183801455,0.));
#15559=DIRECTION('',(-0.569630183801455,0.821901121609115,0.));
#15560=DIRECTION('',(0.,-1.,0.));
#15561=DIRECTION('',(0.,0.,-1.));
#15562=DIRECTION('',(0.,0.,1.));
#15563=DIRECTION('',(0.,0.,-1.));
#15564=DIRECTION('',(-1.,0.,0.));
#15565=DIRECTION('',(-1.22464679914735E-16,0.,-1.));
#15566=DIRECTION('',(-1.,0.,2.06514699521048E-16));
#15567=DIRECTION('',(1.22464679914735E-16,0.,1.));
#15568=DIRECTION('',(-1.,0.,1.80700362080917E-16));
#15569=DIRECTION('',(0.,0.,1.));
#15570=DIRECTION('',(1.,0.,0.));
#15571=DIRECTION('',(1.22464679914735E-16,0.,1.));
#15572=DIRECTION('',(1.,0.,-2.06514699521048E-16));
#15573=DIRECTION('',(-1.22464679914735E-16,0.,-1.));
#15574=DIRECTION('',(1.,0.,-1.80700362080917E-16));
#15575=DIRECTION('',(0.,0.,-1.));
#15576=DIRECTION('',(-1.,0.,0.));
#15577=DIRECTION('',(-1.22464679914735E-16,0.,-1.));
#15578=DIRECTION('',(-1.,0.,0.));
#15579=DIRECTION('',(-1.22464679914735E-16,0.,-1.));
#15580=DIRECTION('',(-1.,0.,0.));
#15581=DIRECTION('',(0.,0.,1.));
#15582=DIRECTION('',(1.,0.,0.));
#15583=DIRECTION('',(1.22464679914735E-16,0.,1.));
#15584=DIRECTION('',(1.,0.,0.));
#15585=DIRECTION('',(-1.22464679914735E-16,0.,-1.));
#15586=DIRECTION('',(1.,0.,0.));
#15587=DIRECTION('',(0.,0.,-1.));
#15588=DIRECTION('',(-1.,0.,0.));
#15589=DIRECTION('',(-1.22464679914735E-16,0.,-1.));
#15590=DIRECTION('',(-1.,0.,0.));
#15591=DIRECTION('',(1.22464679914735E-16,0.,1.));
#15592=DIRECTION('',(-1.,0.,0.));
#15593=DIRECTION('',(0.,0.,-1.));
#15594=DIRECTION('',(-1.,0.,0.));
#15595=DIRECTION('',(-1.22464679914735E-16,0.,-1.));
#15596=DIRECTION('',(-1.,0.,0.));
#15597=DIRECTION('',(-1.22464679914735E-16,0.,-1.));
#15598=DIRECTION('',(-1.,0.,0.));
#15599=DIRECTION('',(0.,0.,1.));
#15600=DIRECTION('',(1.,0.,0.));
#15601=DIRECTION('',(1.22464679914735E-16,0.,1.));
#15602=DIRECTION('',(1.,0.,0.));
#15603=DIRECTION('',(-1.22464679914735E-16,0.,-1.));
#15604=DIRECTION('',(1.,0.,0.));
#15605=DIRECTION('',(0.,0.,1.));
#15606=DIRECTION('',(1.,0.,0.));
#15607=DIRECTION('',(-1.22464679914735E-16,0.,-1.));
#15608=DIRECTION('',(-1.,0.,0.));
#15609=DIRECTION('',(-1.22464679914735E-16,0.,-1.));
#15610=DIRECTION('',(-1.,0.,0.));
#15611=DIRECTION('',(0.,0.,1.));
#15612=DIRECTION('',(1.,0.,0.));
#15613=DIRECTION('',(-1.22464679914735E-16,0.,-1.));
#15614=DIRECTION('',(-1.,0.,1.20466908053945E-16));
#15615=DIRECTION('',(1.22464679914735E-16,0.,1.));
#15616=DIRECTION('',(1.,0.,-1.21972744404619E-16));
#15617=DIRECTION('',(0.,0.,-1.));
#15618=DIRECTION('',(-1.,0.,0.));
#15619=DIRECTION('',(1.22464679914735E-16,0.,1.));
#15620=DIRECTION('',(-1.,0.,0.));
#15621=DIRECTION('',(0.,0.,-1.));
#15622=DIRECTION('',(-1.,0.,0.));
#15623=DIRECTION('',(1.22464679914735E-16,0.,1.));
#15624=DIRECTION('',(1.,0.,0.));
#15625=DIRECTION('',(-1.22464679914735E-16,0.,-1.));
#15626=DIRECTION('',(-1.,0.,0.));
#15627=DIRECTION('',(0.,0.,-1.));
#15628=DIRECTION('',(-1.,0.,0.));
#15629=DIRECTION('',(-1.22464679914735E-16,0.,-1.));
#15630=DIRECTION('',(1.,0.,-1.22876246215024E-16));
#15631=DIRECTION('',(0.,0.,-1.));
#15632=DIRECTION('',(-1.,0.,0.));
#15633=DIRECTION('',(-1.22464679914735E-16,0.,-1.));
#15634=DIRECTION('',(-1.,0.,0.));
#15635=DIRECTION('',(0.,0.,-1.));
#15636=DIRECTION('',(-1.,0.,0.));
#15637=DIRECTION('',(1.22464679914735E-16,0.,1.));
#15638=DIRECTION('',(1.,0.,0.));
#15639=DIRECTION('',(0.,0.,-1.));
#15640=DIRECTION('',(-1.,0.,0.));
#15641=DIRECTION('',(-1.22464679914735E-16,0.,-1.));
#15642=DIRECTION('',(1.,0.,0.));
#15643=DIRECTION('',(-1.22464679914735E-16,0.,-1.));
#15644=DIRECTION('',(-1.,0.,0.));
#15645=DIRECTION('',(0.,0.,1.));
#15646=DIRECTION('',(1.,0.,0.));
#15647=DIRECTION('',(0.,0.,-1.));
#15648=DIRECTION('',(-1.,0.,0.));
#15649=DIRECTION('',(0.,0.,-1.));
#15650=DIRECTION('',(-1.,0.,0.));
#15651=DIRECTION('',(-1.22464679914735E-16,0.,-1.));
#15652=DIRECTION('',(-1.,0.,0.));
#15653=DIRECTION('',(-1.22464679914735E-16,0.,-1.));
#15654=DIRECTION('',(1.,0.,0.));
#15655=DIRECTION('',(0.,0.,-1.));
#15656=DIRECTION('',(-1.,0.,0.));
#15657=DIRECTION('',(0.,0.,-1.));
#15658=DIRECTION('',(-1.,0.,0.));
#15659=DIRECTION('',(1.22464679914735E-16,0.,1.));
#15660=DIRECTION('',(1.,0.,-1.75224593533011E-16));
#15661=DIRECTION('',(0.,0.,-1.));
#15662=DIRECTION('',(-1.,0.,0.));
#15663=DIRECTION('',(1.22464679914735E-16,0.,1.));
#15664=DIRECTION('',(-1.,0.,2.0900282843094E-16));
#15665=DIRECTION('',(-1.22464679914735E-16,0.,-1.));
#15666=DIRECTION('',(1.,0.,-2.0900282843094E-16));
#15667=DIRECTION('',(0.,0.,-1.));
#15668=DIRECTION('',(-1.,0.,0.));
#15669=DIRECTION('',(-1.22464679914735E-16,0.,-1.));
#15670=DIRECTION('',(-1.,0.,1.75224593533011E-16));
#15671=DIRECTION('',(0.,0.,1.));
#15672=DIRECTION('',(1.,0.,0.));
#15673=DIRECTION('',(0.,0.,-1.));
#15674=DIRECTION('',(-1.,0.,0.));
#15675=DIRECTION('',(0.,0.,1.));
#15676=DIRECTION('',(1.,0.,0.));
#15677=DIRECTION('',(0.,0.,1.));
#15678=DIRECTION('',(1.,0.,0.));
#15679=DIRECTION('',(0.,0.,1.));
#15680=DIRECTION('',(1.,0.,0.));
#15681=DIRECTION('',(0.,0.,-1.));
#15682=DIRECTION('',(-1.,0.,0.));
#15683=DIRECTION('',(0.,0.,1.));
#15684=DIRECTION('',(1.,0.,0.));
#15685=DIRECTION('',(0.,0.,-1.));
#15686=DIRECTION('',(-1.,0.,0.));
#15687=DIRECTION('',(0.,0.,-1.));
#15688=DIRECTION('',(-1.,0.,0.));
#15689=DIRECTION('',(0.,0.,1.));
#15690=DIRECTION('',(1.,0.,0.));
#15691=DIRECTION('',(0.,0.,1.));
#15692=DIRECTION('',(1.,0.,0.));
#15693=DIRECTION('',(0.,0.,1.));
#15694=DIRECTION('',(1.,0.,0.));
#15695=DIRECTION('',(-4.16495833440966E-16,0.,-1.));
#15696=DIRECTION('',(1.,0.,0.));
#15697=DIRECTION('',(4.16495833440966E-16,0.,1.));
#15698=DIRECTION('',(-1.,0.,0.));
#15699=DIRECTION('',(0.,0.,-1.));
#15700=DIRECTION('',(-1.,0.,0.));
#15701=DIRECTION('',(0.,0.,1.));
#15702=DIRECTION('',(1.,0.,0.));
#15703=DIRECTION('',(0.,0.,1.));
#15704=DIRECTION('',(1.,0.,0.));
#15705=DIRECTION('',(0.,1.,0.));
#15706=DIRECTION('',(-1.,0.,0.));
#15707=DIRECTION('',(0.929776485888249,0.,0.368124552684684));
#15708=DIRECTION('',(0.368124552684685,0.,-0.929776485888249));
#15709=DIRECTION('',(0.929776485888249,0.,0.368124552684685));
#15710=DIRECTION('',(0.368124552684685,0.,0.929776485888249));
#15711=DIRECTION('',(0.929776485888249,0.,-0.368124552684685));
#15712=DIRECTION('',(0.929776485888249,0.,-0.368124552684684));
#15713=DIRECTION('',(0.,-1.,0.));
#15714=DIRECTION('',(1.,0.,0.));
#15715=DIRECTION('',(-0.527577044868635,0.84863281360662,0.0385332245963262));
#15716=DIRECTION('',(0.847657022497041,0.52887822967871,-0.0420165489226022));
#15717=DIRECTION('',(2.2574675679014E-14,-1.,-2.69034508421066E-14));
#15718=DIRECTION('',(1.,0.,0.));
#15719=DIRECTION('',(-0.984807753012211,0.,0.173648177666916));
#15720=DIRECTION('',(2.73184799366419E-14,1.,-1.46992276411323E-27));
#15721=DIRECTION('',(-0.173648177667176,0.,-0.984807753012165));
#15722=DIRECTION('',(-4.56139972616518E-30,-5.72420986807231E-15,-1.));
#15723=DIRECTION('',(0.,1.,-5.72420986807231E-15));
#15724=DIRECTION('',(0.,0.,-1.));
#15725=DIRECTION('',(-1.,0.,0.));
#15726=DIRECTION('',(0.,9.91462232468849E-15,1.));
#15727=DIRECTION('',(0.,1.,0.));
#15728=DIRECTION('',(-1.,0.,5.46369598732789E-14));
#15729=DIRECTION('',(0.707106781186552,3.95413916520204E-15,0.707106781186544));
#15730=DIRECTION('',(-1.69409931513961E-14,-1.,1.69409931513985E-14));
#15731=DIRECTION('',(0.707106781186497,-2.2765399947205E-14,-0.707106781186598));
#15732=DIRECTION('',(0.,-1.,0.));
#15733=DIRECTION('',(1.,0.,0.));
#15734=DIRECTION('',(0.,0.,-1.));
#15735=DIRECTION('',(0.,0.,-1.));
#15736=DIRECTION('',(-1.,0.,0.));
#15737=DIRECTION('',(0.,0.,-1.));
#15738=DIRECTION('',(-1.,0.,0.));
#15739=DIRECTION('',(0.,0.,-1.));
#15740=DIRECTION('',(-1.,0.,0.));
#15741=DIRECTION('',(0.,0.,-1.));
#15742=DIRECTION('',(-1.,0.,0.));
#15743=DIRECTION('',(0.,0.,-1.));
#15744=DIRECTION('',(-1.,0.,0.));
#15745=DIRECTION('',(0.,0.,1.));
#15746=DIRECTION('',(1.,0.,0.));
#15747=DIRECTION('',(-7.77379789764059E-15,0.999160784934254,0.0409600518745398));
#15748=DIRECTION('',(0.,-0.0409600518745398,0.999160784934254));
#15749=DIRECTION('',(-7.77379789764059E-15,0.999160784934254,0.0409600518745398));
#15750=DIRECTION('',(0.,-0.0409600518745399,0.999160784934254));
#15751=DIRECTION('',(1.54365415442519E-13,0.999160784934254,0.040960051874541));
#15752=DIRECTION('',(9.60032442200731E-5,-0.0409600516857843,0.99916078032981));
#15753=DIRECTION('',(1.54365416289552E-13,0.999160784934254,0.040960051874541));
#15754=DIRECTION('',(9.60032442198703E-5,-0.0409600516857843,0.99916078032981));
#15755=DIRECTION('',(0.,0.,1.));
#15756=DIRECTION('',(0.983655403747905,0.180061230356638,0.));
#15757=DIRECTION('',(0.891006524188365,0.453990499739553,0.));
#15758=DIRECTION('',(-0.453990499739553,0.891006524188365,0.));
#15759=DIRECTION('',(0.891006524188366,0.453990499739551,0.));
#15760=DIRECTION('',(0.45399049973955,-0.891006524188366,0.));
#15761=DIRECTION('',(-0.891006524188365,-0.453990499739553,0.));
#15762=DIRECTION('',(0.891006524188365,0.453990499739553,0.));
#15763=DIRECTION('',(0.,0.,-1.));
#15764=DIRECTION('',(-1.,0.,0.));
#15765=DIRECTION('',(-0.966706191517614,-0.255888919809962,-2.46545352372542E-17));
#15766=DIRECTION('',(-0.255888919809963,0.966706191517614,0.));
#15767=DIRECTION('',(0.,0.,1.));
#15768=DIRECTION('',(-1.,0.,0.));
#15769=DIRECTION('',(0.,0.,-1.));
#15770=DIRECTION('',(-1.,0.,0.));
#15771=DIRECTION('',(0.,0.,-1.));
#15772=DIRECTION('',(-1.,0.,0.));
#15773=DIRECTION('',(0.86760952952486,0.497246120424937,0.));
#15774=DIRECTION('',(-0.497246120424937,0.86760952952486,0.));
#15775=DIRECTION('',(0.,0.,-1.));
#15776=DIRECTION('',(-1.,0.,0.));
#15777=DIRECTION('',(0.,0.,1.));
#15778=DIRECTION('',(-1.,-3.46944695195361E-15,0.));
#15779=DIRECTION('',(0.,0.,-1.));
#15780=DIRECTION('',(-1.,0.,0.));
#15781=DIRECTION('',(-0.891006524188365,0.453990499739553,0.));
#15782=DIRECTION('',(-0.453990499739553,-0.891006524188365,0.));
#15783=DIRECTION('',(0.,0.,1.));
#15784=DIRECTION('',(-1.,-1.73472347597681E-15,0.));
#15785=DIRECTION('',(0.,0.,-1.));
#15786=DIRECTION('',(-1.,0.,0.));
#15787=DIRECTION('',(0.,0.,1.));
#15788=DIRECTION('',(1.,0.,0.));
#15789=DIRECTION('',(0.,0.,1.));
#15790=DIRECTION('',(-1.,-3.46944695195361E-15,0.));
#15791=DIRECTION('',(0.,0.,1.));
#15792=DIRECTION('',(0.,0.,-1.));
#15793=DIRECTION('',(0.891006524188365,-0.453990499739553,0.));
#15794=DIRECTION('',(0.453990499739554,0.891006524188364,0.));
#15795=DIRECTION('',(-0.891006524188365,0.453990499739553,0.));
#15796=DIRECTION('',(0.453990499739553,0.891006524188365,0.));
#15797=DIRECTION('',(0.891006524188365,-0.453990499739553,0.));
#15798=DIRECTION('',(-0.891006524188365,0.453990499739553,0.));
#15799=DIRECTION('',(0.,0.,1.));
#15800=DIRECTION('',(1.,0.,0.));
#15801=DIRECTION('',(0.,0.,1.));
#15802=DIRECTION('',(-1.,-1.73472347597681E-15,0.));
#15803=DIRECTION('',(0.,0.,1.));
#15804=DIRECTION('',(0.,0.,-1.));
#15805=DIRECTION('',(0.,0.,-1.));
#15806=DIRECTION('',(-1.,0.,0.));
#15807=DIRECTION('',(0.,0.,1.));
#15808=DIRECTION('',(-1.,2.25514051876985E-14,0.));
#15809=DIRECTION('',(0.86760952952486,0.497246120424937,0.));
#15810=DIRECTION('',(-0.497246120424937,0.86760952952486,0.));
#15811=DIRECTION('',(-0.891006524188365,-0.453990499739553,-1.57509595553729E-15));
#15812=DIRECTION('',(0.453990499739553,-0.891006524188365,0.));
#15813=DIRECTION('',(0.,0.,-1.));
#15814=DIRECTION('',(-1.,0.,0.));
#15815=DIRECTION('',(-0.838670567945428,-0.544639035015021,0.));
#15816=DIRECTION('',(0.544639035015021,-0.838670567945428,0.));
#15817=DIRECTION('',(0.,0.,-1.));
#15818=DIRECTION('',(-1.,0.,0.));
#15819=DIRECTION('',(-0.864432536983703,-0.50274883292149,0.));
#15820=DIRECTION('',(-0.50274883292149,0.864432536983703,0.));
#15821=DIRECTION('',(0.,0.,1.));
#15822=DIRECTION('',(-1.,9.6277152916713E-14,0.));
#15823=DIRECTION('',(0.,0.,-1.));
#15824=DIRECTION('',(-1.,0.,0.));
#15825=DIRECTION('',(-0.867609529524852,0.497246120424951,0.));
#15826=DIRECTION('',(-0.497246120424951,-0.867609529524852,0.));
#15827=DIRECTION('',(0.,0.,1.));
#15828=DIRECTION('',(-1.,-1.90819582357449E-13,0.));
#15829=DIRECTION('',(0.,0.,-1.));
#15830=DIRECTION('',(-1.,0.,0.));
#15831=DIRECTION('',(0.,0.,-1.));
#15832=DIRECTION('',(-1.,0.,0.));
#15833=DIRECTION('',(0.,0.,1.));
#15834=DIRECTION('',(-1.,0.,0.));
#15835=DIRECTION('',(0.966706191517614,0.255888919809962,0.));
#15836=DIRECTION('',(-0.255888919809962,0.966706191517615,0.));
#15837=DIRECTION('',(-0.891006524188365,0.453990499739553,-1.47230103896192E-17));
#15838=DIRECTION('',(-0.453990499739553,-0.891006524188365,0.));
#15839=DIRECTION('',(-0.891006524188365,-0.453990499739553,0.));
#15840=DIRECTION('',(0.453990499739553,-0.891006524188365,0.));
#15841=DIRECTION('',(0.891006524188365,0.453990499739553,0.));
#15842=DIRECTION('',(-0.891006524188365,-0.453990499739553,0.));
#15843=DIRECTION('',(0.,0.,1.));
#15844=DIRECTION('',(1.,0.,0.));
#15845=DIRECTION('',(0.,0.,1.));
#15846=DIRECTION('',(-1.,9.6277152916713E-14,0.));
#15847=DIRECTION('',(0.,0.,1.));
#15848=DIRECTION('',(0.,0.,-1.));
#15849=DIRECTION('',(-0.838670567945428,-0.544639035015021,0.));
#15850=DIRECTION('',(0.544639035015021,-0.838670567945428,0.));
#15851=DIRECTION('',(-0.838670567945428,-0.544639035015022,0.));
#15852=DIRECTION('',(-0.544639035015022,0.838670567945428,0.));
#15853=DIRECTION('',(0.838670567945428,0.544639035015021,0.));
#15854=DIRECTION('',(-0.838670567945428,-0.544639035015021,0.));
#15855=DIRECTION('',(0.,0.,-1.));
#15856=DIRECTION('',(-1.,0.,0.));
#15857=DIRECTION('',(0.86443253698369,-0.50274883292151,0.));
#15858=DIRECTION('',(-0.50274883292151,-0.86443253698369,0.));
#15859=DIRECTION('',(0.,0.,1.));
#15860=DIRECTION('',(-1.,0.,0.));
#15861=DIRECTION('',(0.,0.,-1.));
#15862=DIRECTION('',(-1.,0.,0.));
#15863=DIRECTION('',(0.,0.,1.));
#15864=DIRECTION('',(1.,0.,0.));
#15865=DIRECTION('',(0.,0.,1.));
#15866=DIRECTION('',(-1.,-1.90819582357449E-13,0.));
#15867=DIRECTION('',(0.,0.,1.));
#15868=DIRECTION('',(0.,0.,-1.));
#15869=DIRECTION('',(-0.891006524188365,0.453990499739553,0.));
#15870=DIRECTION('',(-0.453990499739553,-0.891006524188365,0.));
#15871=DIRECTION('',(-0.891006524188365,0.453990499739553,0.));
#15872=DIRECTION('',(0.453990499739553,0.891006524188365,0.));
#15873=DIRECTION('',(0.891006524188365,-0.453990499739553,0.));
#15874=DIRECTION('',(-0.891006524188365,0.453990499739553,0.));
#15875=DIRECTION('',(0.,0.,-1.));
#15876=DIRECTION('',(-1.,0.,0.));
#15877=DIRECTION('',(0.,0.,1.));
#15878=DIRECTION('',(-1.,0.,0.));
#15879=DIRECTION('',(0.,0.,-1.));
#15880=DIRECTION('',(-1.,0.,0.));
#15881=DIRECTION('',(0.,0.,-1.));
#15882=DIRECTION('',(-1.,0.,0.));
#15883=DIRECTION('',(0.,0.,1.));
#15884=DIRECTION('',(-1.,3.90312782094782E-14,0.));
#15885=DIRECTION('',(-0.838670567945428,-0.544639035015021,0.));
#15886=DIRECTION('',(0.544639035015021,-0.838670567945428,0.));
#15887=DIRECTION('',(-0.864432536983703,-0.50274883292149,0.));
#15888=DIRECTION('',(-0.50274883292149,0.864432536983703,0.));
#15889=DIRECTION('',(0.,0.,-1.));
#15890=DIRECTION('',(-1.,0.,0.));
#15891=DIRECTION('',(-0.26174679065642,-0.96513657975494,0.));
#15892=DIRECTION('',(0.96513657975494,-0.26174679065642,0.));
#15893=DIRECTION('',(0.,0.,-1.));
#15894=DIRECTION('',(-1.,0.,0.));
#15895=DIRECTION('',(0.,0.,1.));
#15896=DIRECTION('',(-1.,1.73472347597681E-15,0.));
#15897=DIRECTION('',(0.,0.,-1.));
#15898=DIRECTION('',(-1.,0.,0.));
#15899=DIRECTION('',(0.838670567945428,-0.544639035015021,0.));
#15900=DIRECTION('',(0.544639035015021,0.838670567945428,0.));
#15901=DIRECTION('',(0.,0.,1.));
#15902=DIRECTION('',(-1.,2.51534904016637E-14,0.));
#15903=DIRECTION('',(0.,0.,-1.));
#15904=DIRECTION('',(-1.,0.,0.));
#15905=DIRECTION('',(0.,0.,-1.));
#15906=DIRECTION('',(-1.,0.,0.));
#15907=DIRECTION('',(-0.867609529524852,0.497246120424951,0.));
#15908=DIRECTION('',(-0.497246120424951,-0.867609529524852,0.));
#15909=DIRECTION('',(0.,0.,1.));
#15910=DIRECTION('',(-1.,0.,0.));
#15911=DIRECTION('',(0.838670567945428,0.544639035015021,0.));
#15912=DIRECTION('',(-0.544639035015021,0.838670567945428,0.));
#15913=DIRECTION('',(-0.838670567945428,-0.544639035015022,6.28163167848562E-16));
#15914=DIRECTION('',(-0.544639035015022,0.838670567945428,0.));
#15915=DIRECTION('',(0.838670567945428,0.544639035015021,0.));
#15916=DIRECTION('',(-0.838670567945428,-0.544639035015021,0.));
#15917=DIRECTION('',(0.,0.,1.));
#15918=DIRECTION('',(1.,0.,0.));
#15919=DIRECTION('',(0.,0.,1.));
#15920=DIRECTION('',(-1.,1.73472347597681E-15,0.));
#15921=DIRECTION('',(0.,0.,1.));
#15922=DIRECTION('',(0.,0.,-1.));
#15923=DIRECTION('',(0.,0.,-1.));
#15924=DIRECTION('',(-1.,0.,0.));
#15925=DIRECTION('',(-0.704959400861195,-0.709247659944977,0.));
#15926=DIRECTION('',(-0.709247659944977,0.704959400861195,0.));
#15927=DIRECTION('',(0.,0.,-1.));
#15928=DIRECTION('',(-1.,0.,0.));
#15929=DIRECTION('',(0.,0.,1.));
#15930=DIRECTION('',(-1.,8.88178419700125E-16,0.));
#15931=DIRECTION('',(-0.838670567945428,0.544639035015022,0.));
#15932=DIRECTION('',(-0.544639035015022,-0.838670567945428,0.));
#15933=DIRECTION('',(0.838670567945428,-0.544639035015022,0.));
#15934=DIRECTION('',(-0.544639035015022,-0.838670567945428,0.));
#15935=DIRECTION('',(-0.838670567945428,0.544639035015022,0.));
#15936=DIRECTION('',(0.838670567945428,-0.544639035015022,0.));
#15937=DIRECTION('',(0.,0.,1.));
#15938=DIRECTION('',(1.,0.,0.));
#15939=DIRECTION('',(0.,0.,1.));
#15940=DIRECTION('',(-1.,2.51534904016637E-14,0.));
#15941=DIRECTION('',(0.,0.,1.));
#15942=DIRECTION('',(0.,0.,-1.));
#15943=DIRECTION('',(0.,0.,-1.));
#15944=DIRECTION('',(-1.,0.,0.));
#15945=DIRECTION('',(0.86443253698369,-0.50274883292151,0.));
#15946=DIRECTION('',(-0.50274883292151,-0.86443253698369,0.));
#15947=DIRECTION('',(0.,0.,1.));
#15948=DIRECTION('',(-1.,0.,0.));
#15949=DIRECTION('',(0.,0.,-1.));
#15950=DIRECTION('',(-1.,0.,0.));
#15951=DIRECTION('',(0.,0.,-1.));
#15952=DIRECTION('',(-1.,0.,0.));
#15953=DIRECTION('',(0.,0.,1.));
#15954=DIRECTION('',(-1.,0.,0.));
#15955=DIRECTION('',(-0.26174679065642,-0.96513657975494,0.));
#15956=DIRECTION('',(0.96513657975494,-0.26174679065642,0.));
#15957=DIRECTION('',(0.,0.,-1.));
#15958=DIRECTION('',(-1.,0.,0.));
#15959=DIRECTION('',(-0.0523359562429378,-0.998629534754574,-4.53942059661595E-17));
#15960=DIRECTION('',(0.998629534754574,-0.0523359562429379,0.));
#15961=DIRECTION('',(0.,0.,-1.));
#15962=DIRECTION('',(-1.,0.,0.));
#15963=DIRECTION('',(0.,0.,1.));
#15964=DIRECTION('',(-1.,5.20417042793042E-15,0.));
#15965=DIRECTION('',(0.,0.,-1.));
#15966=DIRECTION('',(-1.,0.,0.));
#15967=DIRECTION('',(0.26174679065642,-0.96513657975494,0.));
#15968=DIRECTION('',(0.96513657975494,0.26174679065642,0.));
#15969=DIRECTION('',(0.,0.,1.));
#15970=DIRECTION('',(-1.,0.,0.));
#15971=DIRECTION('',(0.,0.,-1.));
#15972=DIRECTION('',(-1.,0.,0.));
#15973=DIRECTION('',(0.,0.,-1.));
#15974=DIRECTION('',(-1.,0.,0.));
#15975=DIRECTION('',(0.838670567945428,-0.544639035015021,0.));
#15976=DIRECTION('',(0.544639035015021,0.838670567945428,0.));
#15977=DIRECTION('',(0.,0.,1.));
#15978=DIRECTION('',(-1.,-2.60208521396521E-15,0.));
#15979=DIRECTION('',(0.,0.,-1.));
#15980=DIRECTION('',(-1.,0.,0.));
#15981=DIRECTION('',(-0.704959400861195,-0.709247659944977,0.));
#15982=DIRECTION('',(-0.709247659944977,0.704959400861195,0.));
#15983=DIRECTION('',(0.,0.,-1.));
#15984=DIRECTION('',(-1.,0.,0.));
#15985=DIRECTION('',(0.,0.,1.));
#15986=DIRECTION('',(-1.,1.77635683940025E-15,0.));
#15987=DIRECTION('',(0.,0.,1.));
#15988=DIRECTION('',(1.,0.,0.));
#15989=DIRECTION('',(0.,0.,1.));
#15990=DIRECTION('',(-1.,5.20417042793042E-15,0.));
#15991=DIRECTION('',(0.,0.,1.));
#15992=DIRECTION('',(0.,0.,-1.));
#15993=DIRECTION('',(-0.052335956242937,-0.998629534754574,0.));
#15994=DIRECTION('',(0.998629534754574,-0.052335956242937,0.));
#15995=DIRECTION('',(-0.052335956242936,-0.998629534754574,0.));
#15996=DIRECTION('',(-0.998629534754574,0.0523359562429361,0.));
#15997=DIRECTION('',(0.052335956242937,0.998629534754574,0.));
#15998=DIRECTION('',(-0.052335956242937,-0.998629534754574,0.));
#15999=DIRECTION('',(0.,0.,-1.));
#16000=DIRECTION('',(-1.,0.,0.));
#16001=DIRECTION('',(0.704959400861195,-0.709247659944977,0.));
#16002=DIRECTION('',(-0.709247659944977,-0.704959400861195,0.));
#16003=DIRECTION('',(0.,0.,1.));
#16004=DIRECTION('',(-1.,0.,0.));
#16005=DIRECTION('',(0.,0.,-1.));
#16006=DIRECTION('',(-1.,0.,0.));
#16007=DIRECTION('',(0.,0.,1.));
#16008=DIRECTION('',(1.,0.,0.));
#16009=DIRECTION('',(0.,0.,1.));
#16010=DIRECTION('',(-1.,0.,0.));
#16011=DIRECTION('',(0.,0.,1.));
#16012=DIRECTION('',(0.,0.,-1.));
#16013=DIRECTION('',(0.838670567945428,-0.544639035015022,0.));
#16014=DIRECTION('',(0.544639035015022,0.838670567945428,0.));
#16015=DIRECTION('',(0.838670567945427,-0.544639035015022,0.));
#16016=DIRECTION('',(-0.544639035015022,-0.838670567945428,0.));
#16017=DIRECTION('',(-0.838670567945428,0.544639035015022,0.));
#16018=DIRECTION('',(0.838670567945428,-0.544639035015022,0.));
#16019=DIRECTION('',(0.,0.,-1.));
#16020=DIRECTION('',(-1.,0.,0.));
#16021=DIRECTION('',(0.,0.,1.));
#16022=DIRECTION('',(-1.,1.73472347597681E-15,0.));
#16023=DIRECTION('',(-0.0523359562429378,-0.998629534754574,0.));
#16024=DIRECTION('',(0.998629534754574,-0.0523359562429379,0.));
#16025=DIRECTION('',(0.,0.,-1.));
#16026=DIRECTION('',(-1.,0.,0.));
#16027=DIRECTION('',(-0.00317699254116094,-0.999994953346462,0.));
#16028=DIRECTION('',(0.999994953346462,-0.00317699254116094,0.));
#16029=DIRECTION('',(0.,0.,-1.));
#16030=DIRECTION('',(-1.,0.,0.));
#16031=DIRECTION('',(0.,0.,1.));
#16032=DIRECTION('',(-1.,0.,0.));
#16033=DIRECTION('',(0.,0.,-1.));
#16034=DIRECTION('',(-1.,0.,0.));
#16035=DIRECTION('',(0.0523359562429378,-0.998629534754574,0.));
#16036=DIRECTION('',(0.998629534754574,0.0523359562429378,0.));
#16037=DIRECTION('',(0.,0.,1.));
#16038=DIRECTION('',(-1.,0.,0.));
#16039=DIRECTION('',(0.,0.,-1.));
#16040=DIRECTION('',(-1.,0.,0.));
#16041=DIRECTION('',(0.,0.,-1.));
#16042=DIRECTION('',(-1.,0.,0.));
#16043=DIRECTION('',(0.26174679065642,-0.96513657975494,0.));
#16044=DIRECTION('',(0.96513657975494,0.26174679065642,0.));
#16045=DIRECTION('',(0.,0.,1.));
#16046=DIRECTION('',(-1.,0.,0.));
#16047=DIRECTION('',(0.052335956242937,0.998629534754574,0.));
#16048=DIRECTION('',(-0.998629534754574,0.052335956242937,0.));
#16049=DIRECTION('',(-0.0523359562429361,-0.998629534754574,4.5394205966158E-17));
#16050=DIRECTION('',(-0.998629534754574,0.0523359562429361,0.));
#16051=DIRECTION('',(0.052335956242937,0.998629534754574,0.));
#16052=DIRECTION('',(-0.052335956242937,-0.998629534754574,0.));
#16053=DIRECTION('',(0.,0.,1.));
#16054=DIRECTION('',(1.,0.,0.));
#16055=DIRECTION('',(0.,0.,1.));
#16056=DIRECTION('',(-1.,0.,0.));
#16057=DIRECTION('',(0.,0.,1.));
#16058=DIRECTION('',(0.,0.,-1.));
#16059=DIRECTION('',(0.,0.,-1.));
#16060=DIRECTION('',(-1.,0.,0.));
#16061=DIRECTION('',(-0.00317699254116094,0.999994953346462,0.));
#16062=DIRECTION('',(0.999994953346462,0.00317699254116094,0.));
#16063=DIRECTION('',(0.,0.,-1.));
#16064=DIRECTION('',(-1.,0.,0.));
#16065=DIRECTION('',(0.,0.,1.));
#16066=DIRECTION('',(-1.,0.,0.));
#16067=DIRECTION('',(-0.052335956242937,0.998629534754574,0.));
#16068=DIRECTION('',(-0.998629534754574,-0.052335956242937,0.));
#16069=DIRECTION('',(0.0523359562429361,-0.998629534754574,-4.5394205966158E-17));
#16070=DIRECTION('',(-0.998629534754574,-0.0523359562429361,0.));
#16071=DIRECTION('',(-0.052335956242937,0.998629534754574,0.));
#16072=DIRECTION('',(0.052335956242937,-0.998629534754574,0.));
#16073=DIRECTION('',(0.,0.,1.));
#16074=DIRECTION('',(1.,0.,0.));
#16075=DIRECTION('',(0.,0.,1.));
#16076=DIRECTION('',(-1.,0.,0.));
#16077=DIRECTION('',(0.,0.,1.));
#16078=DIRECTION('',(0.,0.,-1.));
#16079=DIRECTION('',(0.,0.,-1.));
#16080=DIRECTION('',(-1.,0.,0.));
#16081=DIRECTION('',(0.704959400861195,-0.709247659944977,0.));
#16082=DIRECTION('',(-0.709247659944977,-0.704959400861195,0.));
#16083=DIRECTION('',(0.,0.,1.));
#16084=DIRECTION('',(-1.,0.,0.));
#16085=DIRECTION('',(0.,0.,-1.));
#16086=DIRECTION('',(-1.,0.,0.));
#16087=DIRECTION('',(0.,0.,-1.));
#16088=DIRECTION('',(-1.,0.,0.));
#16089=DIRECTION('',(0.,0.,1.));
#16090=DIRECTION('',(-1.,0.,0.));
#16091=DIRECTION('',(-0.00317699254116094,-0.999994953346462,0.));
#16092=DIRECTION('',(0.999994953346462,-0.00317699254116094,0.));
#16093=DIRECTION('',(0.,0.,-1.));
#16094=DIRECTION('',(-1.,0.,0.));
#16095=DIRECTION('',(0.,0.,1.));
#16096=DIRECTION('',(-1.,0.,0.));
#16097=DIRECTION('',(0.,0.,-1.));
#16098=DIRECTION('',(-1.,0.,0.));
#16099=DIRECTION('',(0.,0.,-1.));
#16100=DIRECTION('',(-1.,0.,0.));
#16101=DIRECTION('',(0.0523359562429378,-0.998629534754574,0.));
#16102=DIRECTION('',(0.998629534754574,0.0523359562429378,0.));
#16103=DIRECTION('',(0.,0.,1.));
#16104=DIRECTION('',(-1.,0.,0.));
#16105=DIRECTION('',(0.,0.,-1.));
#16106=DIRECTION('',(-1.,0.,0.));
#16107=DIRECTION('',(-0.00317699254116094,0.999994953346462,0.));
#16108=DIRECTION('',(0.999994953346462,0.00317699254116094,0.));
#16109=DIRECTION('',(0.,0.,-1.));
#16110=DIRECTION('',(-1.,0.,0.));
#16111=DIRECTION('',(0.,0.,1.));
#16112=DIRECTION('',(-1.,0.,0.));
#16113=DIRECTION('',(0.,0.,1.));
#16114=DIRECTION('',(1.,0.,0.));
#16115=DIRECTION('',(0.,0.,1.));
#16116=DIRECTION('',(-1.,0.,0.));
#16117=DIRECTION('',(0.,0.,1.));
#16118=DIRECTION('',(0.,0.,-1.));
#16119=DIRECTION('',(0.052335956242937,-0.998629534754574,0.));
#16120=DIRECTION('',(0.998629534754574,0.052335956242937,0.));
#16121=DIRECTION('',(0.052335956242936,-0.998629534754574,0.));
#16122=DIRECTION('',(-0.998629534754574,-0.0523359562429361,0.));
#16123=DIRECTION('',(-0.052335956242937,0.998629534754574,0.));
#16124=DIRECTION('',(0.052335956242937,-0.998629534754574,0.));
#16125=DIRECTION('',(0.,0.,-1.));
#16126=DIRECTION('',(-1.,0.,0.));
#16127=DIRECTION('',(0.,0.,1.));
#16128=DIRECTION('',(-1.,0.,0.));
#16129=DIRECTION('',(0.,0.,1.));
#16130=DIRECTION('',(1.,0.,0.));
#16131=DIRECTION('',(0.,0.,-1.));
#16132=DIRECTION('',(-1.,0.,0.));
#16133=DIRECTION('',(0.,0.,-1.));
#16134=DIRECTION('',(-1.,0.,0.));
#16135=DIRECTION('',(0.,0.,1.));
#16136=DIRECTION('',(1.,0.,0.));
#16137=DIRECTION('',(0.,0.,-1.));
#16138=DIRECTION('',(-1.,0.,0.));
#16139=DIRECTION('',(0.,0.,-1.));
#16140=DIRECTION('',(-1.,0.,0.));
#16141=DIRECTION('',(0.,0.,1.));
#16142=DIRECTION('',(1.,0.,0.));
#16143=DIRECTION('',(0.,0.,-1.));
#16144=DIRECTION('',(-1.,0.,0.));
#16145=DIRECTION('',(0.,0.,-1.));
#16146=DIRECTION('',(-1.,0.,0.));
#16147=DIRECTION('',(0.866025403784438,0.,-0.5));
#16148=DIRECTION('',(0.493314204695212,-0.711787254343556,0.499999999999992));
#16149=DIRECTION('',(-0.866025403784438,0.,-0.5));
#16150=DIRECTION('',(-0.493317826094965,0.711784843538332,0.499999858966031));
#16151=DIRECTION('',(0.,0.,-1.));
#16152=DIRECTION('',(-1.,0.,0.));
#16153=DIRECTION('',(0.,0.,-1.));
#16154=DIRECTION('',(4.82420265013935E-6,3.34348237489084E-6,0.999999999982774));
#16155=DIRECTION('',(0.821901125801989,0.569630177751691,0.));
#16156=DIRECTION('',(-0.569630177751691,0.821901125801989,0.));
#16157=DIRECTION('',(0.,0.,-1.));
#16158=DIRECTION('',(0.,-1.,0.));
#16159=DIRECTION('',(0.,0.,-1.));
#16160=DIRECTION('',(0.,0.,1.));
#16161=DIRECTION('',(0.,0.,1.));
#16162=DIRECTION('',(1.,0.,0.));
#16163=DIRECTION('',(0.,0.,1.));
#16164=DIRECTION('',(1.,0.,0.));
#16165=DIRECTION('',(0.,0.,-1.));
#16166=DIRECTION('',(1.,0.,0.));
#16167=DIRECTION('',(0.,0.,-1.));
#16168=DIRECTION('',(-1.,0.,0.));
#16169=DIRECTION('',(0.,0.,-1.));
#16170=DIRECTION('',(-1.,0.,0.));
#16171=DIRECTION('',(0.,0.,-1.));
#16172=DIRECTION('',(-1.,0.,0.));
#16173=DIRECTION('',(0.,0.,-1.));
#16174=DIRECTION('',(-1.,0.,0.));
#16175=DIRECTION('',(0.,0.,-1.));
#16176=DIRECTION('',(-1.,0.,0.));
#16177=DIRECTION('',(0.,0.,1.));
#16178=DIRECTION('',(-1.,0.,0.));
#16179=DIRECTION('',(0.,0.,1.));
#16180=DIRECTION('',(1.,0.,0.));
#16181=DIRECTION('',(0.544639035015021,-0.838670567945428,0.));
#16182=DIRECTION('',(0.838670567945428,0.544639035015021,0.));
#16183=DIRECTION('',(0.,0.,1.));
#16184=DIRECTION('',(1.,0.,0.));
#16185=DIRECTION('',(0.,0.,1.));
#16186=DIRECTION('',(-1.,0.,0.));
#16187=DIRECTION('',(0.,0.,-1.));
#16188=DIRECTION('',(-1.,0.,0.));
#16189=DIRECTION('',(0.453990499739553,-0.891006524188365,0.));
#16190=DIRECTION('',(0.891006524188365,0.453990499739553,0.));
#16191=DIRECTION('',(0.,0.,1.));
#16192=DIRECTION('',(0.,0.,1.));
#16193=DIRECTION('',(1.,0.,0.));
#16194=DIRECTION('',(0.453990499739553,0.891006524188365,0.));
#16195=DIRECTION('',(-0.891006524188365,0.453990499739553,0.));
#16196=DIRECTION('',(0.544639035015022,0.838670567945428,0.));
#16197=DIRECTION('',(-0.838670567945428,0.544639035015022,0.));
#16198=DIRECTION('',(0.,0.,1.));
#16199=DIRECTION('',(1.,0.,0.));
#16200=DIRECTION('',(-0.998629534754574,-0.052335956242937,0.));
#16201=DIRECTION('',(0.052335956242937,-0.998629534754574,0.));
#16202=DIRECTION('',(0.,0.,1.));
#16203=DIRECTION('',(1.,0.,0.));
#16204=DIRECTION('',(-0.998629534754574,0.052335956242937,0.));
#16205=DIRECTION('',(-0.052335956242937,-0.998629534754574,0.));
#16206=DIRECTION('',(0.,0.,-1.));
#16207=DIRECTION('',(-1.,0.,0.));
#16208=DIRECTION('',(0.,0.,1.));
#16209=DIRECTION('',(-1.,0.,0.));
#16210=DIRECTION('',(0.,0.,-1.));
#16211=DIRECTION('',(-1.,0.,0.));
#16212=DIRECTION('',(0.,0.,-1.));
#16213=DIRECTION('',(-1.,0.,0.));
#16214=DIRECTION('',(0.,0.,-1.));
#16215=DIRECTION('',(-1.,0.,0.));
#16216=DIRECTION('',(0.,0.,-1.));
#16217=DIRECTION('',(-1.,0.,0.));
#16218=DIRECTION('',(0.,0.,1.));
#16219=DIRECTION('',(1.,0.,0.));
#16220=DIRECTION('',(0.,0.,1.));
#16221=DIRECTION('',(1.,0.,0.));
#16222=DIRECTION('',(0.,0.,-1.));
#16223=DIRECTION('',(-1.,0.,0.));
#16224=DIRECTION('',(0.,0.,-1.));
#16225=DIRECTION('',(-1.,0.,0.));
#16226=DIRECTION('',(0.,0.,-1.));
#16227=DIRECTION('',(-1.,0.,0.));
#16228=DIRECTION('',(0.,0.,-1.));
#16229=DIRECTION('',(-1.,0.,0.));
#16230=DIRECTION('',(0.,0.,-1.));
#16231=DIRECTION('',(-1.,0.,0.));
#16232=DIRECTION('',(0.,0.,-1.));
#16233=DIRECTION('',(-1.,0.,0.));
#16234=DIRECTION('',(0.,0.,-1.));
#16235=DIRECTION('',(-1.,0.,0.));
#16236=DIRECTION('',(0.,0.,-1.));
#16237=DIRECTION('',(-1.,0.,0.));
#16238=DIRECTION('',(0.,0.,-1.));
#16239=DIRECTION('',(-1.,0.,0.));
#16240=DIRECTION('',(0.,0.,-1.));
#16241=DIRECTION('',(-1.,0.,0.));
#16242=DIRECTION('',(0.,0.,1.));
#16243=DIRECTION('',(1.,0.,0.));
#16244=DIRECTION('',(0.,0.,1.));
#16245=DIRECTION('',(-0.500000000000056,0.866025403784406,0.));
#16246=DIRECTION('',(0.616239312964626,2.85818950259745E-15,-0.787558955987986));
#16247=DIRECTION('',(0.787558955987986,-2.15158806147751E-15,0.616239312964626));
#16248=DIRECTION('',(-0.616239312964626,-2.85818950259745E-15,0.787558955987986));
#16249=DIRECTION('',(-0.787558955987986,0.,-0.616239312964626));
#16250=DIRECTION('',(0.785096318706608,0.0790194346750136,0.614312379247703));
#16251=DIRECTION('',(0.,-1.,-1.37693951293562E-16));
#16252=DIRECTION('',(0.785096318706608,-0.079019434675018,0.614312379247703));
#16253=DIRECTION('',(-0.100143387937821,0.994973015640291,3.47392971676056E-15));
#16254=DIRECTION('',(-0.994973015640291,-0.100143387937821,-3.49648770193432E-16));
#16255=DIRECTION('',(-0.990021088684022,-0.0996449797052097,-0.0996449797052101));
#16256=DIRECTION('',(0.100143387937821,-0.994973015640291,-3.47392971676056E-15));
#16257=DIRECTION('',(-0.994973015640291,-0.100143387937821,0.));
#16258=DIRECTION('',(-0.100143387937822,-0.994973015640291,-3.59560665342334E-15));
#16259=DIRECTION('',(0.994973015640291,-0.100143387937822,-3.49648770193432E-16));
#16260=DIRECTION('',(0.990021088684022,-0.0996449797052105,0.0996449797052101));
#16261=DIRECTION('',(0.100143387937822,0.994973015640291,3.59560665342334E-15));
#16262=DIRECTION('',(0.994973015640291,-0.100143387937822,0.));
#16263=DIRECTION('',(0.616239312964626,-2.74974739807084E-15,0.787558955987986));
#16264=DIRECTION('',(-0.787558955987986,-2.15158806147751E-15,0.616239312964626));
#16265=DIRECTION('',(-0.616239312964626,2.74974739807084E-15,-0.787558955987986));
#16266=DIRECTION('',(0.787558955987986,1.06581410364015E-14,-0.616239312964626));
#16267=DIRECTION('',(0.785096318706608,-0.0790194346750135,-0.614312379247703));
#16268=DIRECTION('',(0.,1.,6.88469756467808E-17));
#16269=DIRECTION('',(0.785096318706608,0.0790194346750179,-0.614312379247703));
#16270=DIRECTION('',(-0.100143387937821,0.994973015640291,3.47392971676056E-15));
#16271=DIRECTION('',(-0.994973015640291,-0.100143387937821,-3.49648770193432E-16));
#16272=DIRECTION('',(0.990021088684022,0.0996449797052104,-0.09964497970521));
#16273=DIRECTION('',(0.100143387937821,-0.994973015640291,-3.47392971676056E-15));
#16274=DIRECTION('',(-0.994973015640291,-0.100143387937821,-9.76996261670138E-15));
#16275=DIRECTION('',(-0.100143387937822,-0.994973015640291,-3.59560665342334E-15));
#16276=DIRECTION('',(0.994973015640291,-0.100143387937822,-3.49648770193432E-16));
#16277=DIRECTION('',(-0.990021088684022,0.0996449797052097,0.09964497970521));
#16278=DIRECTION('',(0.100143387937822,0.994973015640291,3.59560665342334E-15));
#16279=DIRECTION('',(0.994973015640291,-0.100143387937822,0.));
#16280=DIRECTION('',(0.616239312964626,-0.787558955987986,-1.08442104526618E-16));
#16281=DIRECTION('',(0.787558955987986,0.616239312964626,0.));
#16282=DIRECTION('',(0.785096318706608,0.614312379247703,0.0790194346750159));
#16283=DIRECTION('',(-0.616239312964626,0.787558955987986,1.08442104526618E-16));
#16284=DIRECTION('',(0.787558955987986,0.616239312964626,0.));
#16285=DIRECTION('',(0.785096318706608,0.614312379247703,-0.0790194346750157));
#16286=DIRECTION('',(0.,-1.37693951293562E-16,1.));
#16287=DIRECTION('',(0.616239312964626,0.787558955987986,0.));
#16288=DIRECTION('',(-0.787558955987986,0.616239312964626,0.));
#16289=DIRECTION('',(-0.616239312964626,-0.787558955987986,0.));
#16290=DIRECTION('',(-0.787558955987986,0.616239312964626,3.19744231092045E-14));
#16291=DIRECTION('',(0.785096318706608,-0.614312379247703,0.0790194346750157));
#16292=DIRECTION('',(0.,0.,-1.));
#16293=DIRECTION('',(0.785096318706608,-0.614312379247703,-0.0790194346750157));
#16294=DIRECTION('',(-1.,0.,0.));
#16295=DIRECTION('',(0.,0.,1.));
#16296=DIRECTION('',(-1.,0.,0.));
#16297=DIRECTION('',(0.,0.,1.));
#16298=DIRECTION('',(-1.,0.,0.));
#16299=DIRECTION('',(0.,0.,1.));
#16300=DIRECTION('',(-1.,0.,0.));
#16301=DIRECTION('',(0.,0.,1.));
#16302=DIRECTION('',(1.,0.,0.));
#16303=DIRECTION('',(0.,0.,-1.));
#16304=DIRECTION('',(-1.,0.,0.));
#16305=DIRECTION('',(0.,0.,1.));
#16306=DIRECTION('',(-0.100143387937821,0.,-0.994973015640291));
#16307=DIRECTION('',(-0.994973015640291,0.,0.100143387937821));
#16308=DIRECTION('',(0.100143387937821,0.,0.994973015640291));
#16309=DIRECTION('',(-0.994973015640291,0.,0.100143387937821));
#16310=DIRECTION('',(-0.100143387937821,0.,-0.994973015640291));
#16311=DIRECTION('',(-0.994973015640291,0.,0.100143387937821));
#16312=DIRECTION('',(0.100143387937821,0.,0.994973015640291));
#16313=DIRECTION('',(-0.994973015640291,2.66453525910038E-15,0.100143387937821));
#16314=DIRECTION('',(-0.100143387937822,-1.21676936662784E-16,0.994973015640291));
#16315=DIRECTION('',(0.994973015640291,0.,0.100143387937822));
#16316=DIRECTION('',(0.100143387937822,1.21676936662784E-16,-0.994973015640291));
#16317=DIRECTION('',(0.994973015640291,0.,0.100143387937822));
#16318=DIRECTION('',(-0.100143387937822,-1.21676936662784E-16,0.994973015640291));
#16319=DIRECTION('',(0.994973015640291,0.,0.100143387937822));
#16320=DIRECTION('',(0.100143387937822,1.21676936662784E-16,-0.994973015640291));
#16321=DIRECTION('',(0.994973015640291,0.,0.100143387937822));
#16322=DIRECTION('',(0.,0.,1.));
#16323=DIRECTION('',(0.,-1.,0.));
#16324=DIRECTION('',(-1.,0.,0.));
#16325=DIRECTION('',(0.,0.,1.));
#16326=DIRECTION('',(-1.,0.,0.));
#16327=DIRECTION('',(0.,0.,1.));
#16328=DIRECTION('',(1.,0.,0.));
#16329=DIRECTION('',(0.,0.,-1.));
#16330=DIRECTION('',(1.,0.,0.));
#16331=DIRECTION('',(0.,0.,-1.));
#16332=DIRECTION('',(1.,0.,0.));
#16333=DIRECTION('',(0.,0.,-1.));
#16334=DIRECTION('',(0.,0.,-1.));
#16335=DIRECTION('',(-1.,0.,0.));
#16336=DIRECTION('',(0.,0.,-1.));
#16337=DIRECTION('',(-1.,0.,0.));
#16338=DIRECTION('',(0.,0.,-1.));
#16339=DIRECTION('',(-1.,0.,0.));
#16340=DIRECTION('',(0.,0.,-1.));
#16341=DIRECTION('',(-1.,0.,0.));
#16342=DIRECTION('',(0.,0.,-1.));
#16343=DIRECTION('',(-1.,0.,0.));
#16344=DIRECTION('',(0.,0.,-1.));
#16345=DIRECTION('',(-1.,0.,0.));
#16346=DIRECTION('',(0.,0.,1.));
#16347=DIRECTION('',(1.,0.,0.));
#16348=DIRECTION('',(0.,0.,-1.));
#16349=DIRECTION('',(-1.,0.,0.));
#16350=DIRECTION('',(0.,0.,1.));
#16351=DIRECTION('',(1.,0.,0.));
#16352=DIRECTION('',(0.,0.,1.));
#16353=DIRECTION('',(1.,0.,0.));
#16354=DIRECTION('',(0.,0.,-1.));
#16355=DIRECTION('',(-1.,0.,0.));
#16356=DIRECTION('',(0.,0.,-1.));
#16357=DIRECTION('',(-1.,0.,0.));
#16358=DIRECTION('',(0.,0.,-1.));
#16359=DIRECTION('',(-1.,0.,0.));
#16360=DIRECTION('',(2.02279097019906E-26,2.29526927169303E-26,1.));
#16361=DIRECTION('',(-0.249706656951008,-0.968321530006615,2.72766302382206E-26));
#16362=DIRECTION('',(1.,0.,0.));
#16363=DIRECTION('',(0.,0.,-1.));
#16364=DIRECTION('',(0.,0.,-1.));
#16365=DIRECTION('',(-1.,0.,0.));
#16366=DIRECTION('',(0.,0.,-1.));
#16367=DIRECTION('',(-1.,0.,0.));
#16368=DIRECTION('',(0.,0.,-1.));
#16369=DIRECTION('',(-1.,0.,0.));
#16370=DIRECTION('',(0.,0.,1.));
#16371=DIRECTION('',(1.,0.,0.));
#16372=DIRECTION('',(0.,0.,-1.));
#16373=DIRECTION('',(-1.,0.,0.));
#16374=DIRECTION('',(0.,0.,-1.));
#16375=DIRECTION('',(-1.,0.,0.));
#16376=DIRECTION('',(0.,0.,-1.));
#16377=DIRECTION('',(-1.,0.,0.));
#16378=DIRECTION('',(0.,0.,-1.));
#16379=DIRECTION('',(-1.,0.,0.));
#16380=DIRECTION('',(0.,0.,-1.));
#16381=DIRECTION('',(-1.,0.,0.));
#16382=DIRECTION('',(0.,0.,-1.));
#16383=DIRECTION('',(-1.,0.,0.));
#16384=DIRECTION('',(0.,0.,-1.));
#16385=DIRECTION('',(-1.,0.,0.));
#16386=DIRECTION('',(0.,0.,-1.));
#16387=DIRECTION('',(-1.,0.,0.));
#16388=DIRECTION('',(0.,0.,-1.));
#16389=DIRECTION('',(-1.,0.,0.));
#16390=DIRECTION('',(0.,0.,-1.));
#16391=DIRECTION('',(-1.,0.,0.));
#16392=DIRECTION('',(0.,0.,-1.));
#16393=DIRECTION('',(-1.,0.,0.));
#16394=DIRECTION('',(0.,0.,1.));
#16395=DIRECTION('',(1.,0.,0.));
#16396=DIRECTION('',(0.,0.,-1.));
#16397=DIRECTION('',(-1.,0.,0.));
#16398=DIRECTION('',(0.,0.,-1.));
#16399=DIRECTION('',(-1.,0.,0.));
#16400=DIRECTION('',(0.,0.,-1.));
#16401=DIRECTION('',(-1.,0.,0.));
#16402=DIRECTION('',(0.,0.,-1.));
#16403=DIRECTION('',(-1.,0.,0.));
#16404=DIRECTION('',(0.,0.,-1.));
#16405=DIRECTION('',(-1.,0.,0.));
#16406=DIRECTION('',(0.,0.,-1.));
#16407=DIRECTION('',(-1.,0.,0.));
#16408=DIRECTION('',(0.,0.,1.));
#16409=DIRECTION('',(0.999669994077398,0.0256885760853925,0.));
#16410=DIRECTION('',(0.,-1.,0.));
#16411=DIRECTION('',(1.,4.55307998944049E-15,0.));
#16412=DIRECTION('',(1.69409931514E-14,-1.,-1.69409931514E-14));
#16413=DIRECTION('',(-0.707106781186545,-1.82123199577605E-14,0.70710678118655));
#16414=DIRECTION('',(-0.707106781186548,-6.69019751772657E-12,-0.707106781186548));
#16415=DIRECTION('',(-0.707106781186549,-7.90827833040412E-15,0.707106781186547));
#16416=DIRECTION('',(4.08991754261793E-14,1.,1.69409931513988E-14));
#16417=DIRECTION('',(-0.707106781186585,4.09777199049619E-14,-0.70710678118651));
#16418=DIRECTION('',(0.,0.,-1.));
#16419=DIRECTION('',(-1.,0.,0.));
#16420=DIRECTION('',(0.,0.,-1.));
#16421=DIRECTION('',(-1.,0.,0.));
#16422=DIRECTION('',(0.,0.,1.));
#16423=DIRECTION('',(0.,1.,0.));
#16424=DIRECTION('',(0.,0.,1.));
#16425=DIRECTION('',(3.20622841942719E-14,-1.,-2.6903450842113E-14));
#16426=DIRECTION('',(0.173648177666964,2.73184799366429E-14,-0.984807753012202));
#16427=DIRECTION('',(0.984807753012211,1.05615708143971E-14,0.173648177666915));
#16428=DIRECTION('',(0.,1.,0.));
#16429=DIRECTION('',(-1.,0.,0.));
#16430=DIRECTION('',(0.,0.,-1.));
#16431=DIRECTION('',(0.,0.,-1.));
#16432=DIRECTION('',(-1.,0.,0.));
#16433=DIRECTION('',(0.,0.,1.));
#16434=DIRECTION('',(0.,0.,-1.));
#16435=DIRECTION('',(-1.,0.,0.));
#16436=DIRECTION('',(0.,0.,1.));
#16437=DIRECTION('',(1.,0.,0.));
#16438=DIRECTION('',(0.,1.,0.));
#16439=DIRECTION('',(0.,0.,1.));
#16440=DIRECTION('',(-1.,2.41270005758632E-13,0.));
#16441=DIRECTION('',(0.,0.,1.));
#16442=DIRECTION('',(0.,1.,0.));
#16443=DIRECTION('',(0.,0.,1.));
#16444=DIRECTION('',(0.,0.,1.));
#16445=DIRECTION('',(1.,-2.41270005758632E-13,0.));
#16446=DIRECTION('',(0.984807753012211,1.05615708143972E-14,-0.173648177666916));
#16447=DIRECTION('',(-3.20622841942655E-14,-1.,-2.69034508421121E-14));
#16448=DIRECTION('',(-1.,2.73184799366474E-14,0.));
#16449=DIRECTION('',(0.0157590095386061,0.0588134242587623,0.998144596110865));
#16450=DIRECTION('',(-0.89391175202766,0.448074518359429,-0.012288432927183));
#16451=DIRECTION('',(0.,0.,-1.));
#16452=DIRECTION('',(-1.,0.,0.));
#16453=DIRECTION('',(0.,0.,1.));
#16454=DIRECTION('',(1.,0.,0.));
#16455=DIRECTION('',(0.,0.,1.));
#16456=DIRECTION('',(1.,0.,0.));
#16457=DIRECTION('',(0.,0.,-1.));
#16458=DIRECTION('',(-1.,0.,0.));
#16459=DIRECTION('',(0.,0.,1.));
#16460=DIRECTION('',(1.,0.,0.));
#16461=DIRECTION('',(0.,0.,1.));
#16462=DIRECTION('',(1.,0.,0.));
#16463=DIRECTION('',(0.,0.,1.));
#16464=DIRECTION('',(1.,0.,0.));
#16465=DIRECTION('',(0.,0.,1.));
#16466=DIRECTION('',(1.,0.,0.));
#16467=DIRECTION('',(0.,0.,-1.));
#16468=DIRECTION('',(1.,0.,0.));
#16469=DIRECTION('',(0.,0.,-1.));
#16470=DIRECTION('',(1.,0.,0.));
#16471=DIRECTION('',(0.,0.,1.));
#16472=DIRECTION('',(1.,0.,0.));
#16473=DIRECTION('',(0.,0.,-1.));
#16474=DIRECTION('',(-1.,0.,0.));
#16475=DIRECTION('',(0.,0.,-1.));
#16476=DIRECTION('',(-1.,0.,0.));
#16477=DIRECTION('',(0.,0.,-1.));
#16478=DIRECTION('',(-1.,0.,0.));
#16479=DIRECTION('',(0.,0.,-1.));
#16480=DIRECTION('',(-1.,0.,0.));
#16481=DIRECTION('',(0.,0.,1.));
#16482=DIRECTION('',(1.,0.,0.));
#16483=DIRECTION('',(0.,0.,-1.));
#16484=DIRECTION('',(-1.,0.,0.));
#16485=DIRECTION('',(0.,0.,-1.));
#16486=DIRECTION('',(-1.,0.,0.));
#16487=DIRECTION('',(0.,0.,-1.));
#16488=DIRECTION('',(-1.,0.,0.));
#16489=DIRECTION('',(0.,0.,1.));
#16490=DIRECTION('',(1.,0.,0.));
#16491=DIRECTION('',(0.,0.,-1.));
#16492=DIRECTION('',(-1.,0.,0.));
#16493=DIRECTION('',(0.,0.,-1.));
#16494=DIRECTION('',(-1.,0.,0.));
#16495=DIRECTION('',(0.,0.,-1.));
#16496=DIRECTION('',(-1.,0.,0.));
#16497=DIRECTION('',(0.,0.,-1.));
#16498=DIRECTION('',(-1.,0.,0.));
#16499=DIRECTION('',(0.,0.,-1.));
#16500=DIRECTION('',(-1.,0.,0.));
#16501=DIRECTION('',(0.,0.,-1.));
#16502=DIRECTION('',(-1.,0.,0.));
#16503=DIRECTION('',(0.,0.,1.));
#16504=DIRECTION('',(1.,0.,0.));
#16505=DIRECTION('',(0.,0.,-1.));
#16506=DIRECTION('',(1.,0.,0.));
#16507=DIRECTION('',(0.,0.,1.));
#16508=DIRECTION('',(1.,0.,0.));
#16509=DIRECTION('',(0.,0.,1.));
#16510=DIRECTION('',(1.,0.,0.));
#16511=DIRECTION('',(0.,0.,-1.));
#16512=DIRECTION('',(1.,0.,0.));
#16513=DIRECTION('',(0.,0.,1.));
#16514=DIRECTION('',(1.,0.,0.));
#16515=DIRECTION('',(0.,0.,-1.));
#16516=DIRECTION('',(-1.,0.,0.));
#16517=DIRECTION('',(0.,0.,1.));
#16518=DIRECTION('',(1.,0.,0.));
#16519=DIRECTION('',(0.,0.,-1.));
#16520=DIRECTION('',(1.,0.,0.));
#16521=DIRECTION('',(0.,0.,-1.));
#16522=DIRECTION('',(-1.,0.,0.));
#16523=DIRECTION('',(0.,0.,-1.));
#16524=DIRECTION('',(1.,0.,0.));
#16525=DIRECTION('',(0.,0.,-1.));
#16526=DIRECTION('',(-1.,0.,0.));
#16527=DIRECTION('',(0.,0.,-1.));
#16528=DIRECTION('',(-1.,0.,0.));
#16529=DIRECTION('',(0.,0.,-1.));
#16530=DIRECTION('',(-1.,0.,0.));
#16531=DIRECTION('',(0.,0.,-1.));
#16532=DIRECTION('',(-1.,0.,0.));
#16533=DIRECTION('',(0.,0.,1.));
#16534=DIRECTION('',(1.,0.,0.));
#16535=DIRECTION('',(0.,0.,-1.));
#16536=DIRECTION('',(-1.,0.,0.));
#16537=DIRECTION('',(0.,0.,1.));
#16538=DIRECTION('',(1.,0.,0.));
#16539=DIRECTION('',(0.,0.,-1.));
#16540=DIRECTION('',(-1.,0.,0.));
#16541=DIRECTION('',(0.,0.,-1.));
#16542=DIRECTION('',(-1.,0.,0.));
#16543=DIRECTION('',(0.,0.,-1.));
#16544=DIRECTION('',(-1.,0.,0.));
#16545=DIRECTION('',(0.,0.,1.));
#16546=DIRECTION('',(1.,0.,0.));
#16547=DIRECTION('',(0.,0.,1.));
#16548=DIRECTION('',(1.,0.,0.));
#16549=DIRECTION('',(0.,0.,1.));
#16550=DIRECTION('',(-1.,0.,0.));
#16551=DIRECTION('',(0.,0.,-1.));
#16552=DIRECTION('',(-1.,0.,0.));
#16553=DIRECTION('',(0.,0.,1.));
#16554=DIRECTION('',(1.,0.,0.));
#16555=DIRECTION('',(0.,0.,-1.));
#16556=DIRECTION('',(-1.,0.,0.));
#16557=DIRECTION('',(0.,0.,-1.));
#16558=DIRECTION('',(-1.,0.,0.));
#16559=DIRECTION('',(0.,0.,-1.));
#16560=DIRECTION('',(-1.,0.,0.));
#16561=DIRECTION('',(0.,0.,-1.));
#16562=DIRECTION('',(-1.,0.,0.));
#16563=DIRECTION('',(0.,0.,-1.));
#16564=DIRECTION('',(-1.,0.,0.));
#16565=DIRECTION('',(0.,0.,1.));
#16566=DIRECTION('',(1.,0.,0.));
#16567=DIRECTION('',(0.,0.,1.));
#16568=DIRECTION('',(1.,0.,0.));
#16569=DIRECTION('',(0.,0.,1.));
#16570=DIRECTION('',(1.,0.,0.));
#16571=DIRECTION('',(0.,0.,1.));
#16572=DIRECTION('',(1.,0.,0.));
#16573=DIRECTION('',(0.,0.,1.));
#16574=DIRECTION('',(1.,0.,0.));
#16575=DIRECTION('',(0.,0.,1.));
#16576=DIRECTION('',(1.,0.,0.));
#16577=DIRECTION('',(0.,0.,1.));
#16578=DIRECTION('',(1.,0.,0.));
#16579=DIRECTION('',(0.,0.,1.));
#16580=DIRECTION('',(1.,0.,0.));
#16581=DIRECTION('',(0.,1.,0.));
#16582=DIRECTION('',(1.,0.,0.));
#16583=DIRECTION('',(0.,-1.,0.));
#16584=DIRECTION('',(0.,0.,-1.));
#16585=DIRECTION('',(0.,1.,0.));
#16586=DIRECTION('',(0.,0.,-1.));
#16587=DIRECTION('',(0.86602540378444,-0.5,0.));
#16588=DIRECTION('',(0.866025403784438,0.5,-1.06057523872491E-16));
#16589=DIRECTION('',(-0.86602540378444,-0.5,0.));
#16590=DIRECTION('',(-0.86602540378444,0.5,1.06057523872491E-16));
#16591=DIRECTION('',(0.,1.,0.));
#16592=DIRECTION('',(0.,0.,1.));
#16593=DIRECTION('',(0.,-1.,0.));
#16594=DIRECTION('',(0.,1.,0.));
#16595=DIRECTION('',(0.,0.,1.));
#16596=DIRECTION('',(1.,0.,0.));
#16597=DIRECTION('',(-1.,0.,1.22464679914735E-16));
#16598=DIRECTION('',(0.,-1.,0.));
#16599=DIRECTION('',(0.,0.,1.));
#16600=DIRECTION('',(1.,0.,0.));
#16601=DIRECTION('',(0.,1.,0.));
#16602=DIRECTION('',(0.,1.,0.));
#16603=DIRECTION('',(0.,0.,1.));
#16604=DIRECTION('',(0.,1.,0.));
#16605=DIRECTION('',(0.,0.,1.));
#16606=DIRECTION('',(0.,-1.,0.));
#16607=DIRECTION('',(0.,0.,1.));
#16608=DIRECTION('',(0.,1.,0.));
#16609=DIRECTION('',(0.,0.,1.));
#16610=DIRECTION('',(0.86602540378444,0.,-0.5));
#16611=DIRECTION('',(0.,1.,0.));
#16612=DIRECTION('',(0.,0.,1.));
#16613=DIRECTION('',(-0.793353340291235,0.,-0.608761429008721));
#16614=DIRECTION('',(0.923879532511287,0.,-0.382683432365091));
#16615=DIRECTION('',(0.,1.,0.));
#16616=DIRECTION('',(0.,0.,1.));
#16617=DIRECTION('',(-0.707106781186548,0.,-0.707106781186548));
#16618=DIRECTION('',(0.965925826289068,0.,-0.258819045102522));
#16619=DIRECTION('',(0.,1.,0.));
#16620=DIRECTION('',(0.,0.,1.));
#16621=DIRECTION('',(-0.60876142900872,0.,-0.793353340291235));
#16622=DIRECTION('',(0.99144486137381,0.,-0.130526192220053));
#16623=DIRECTION('',(0.,1.,0.));
#16624=DIRECTION('',(0.,0.,1.));
#16625=DIRECTION('',(-0.5,0.,-0.866025403784439));
#16626=DIRECTION('',(1.,0.,-1.47392777911416E-15));
#16627=DIRECTION('',(0.,1.,0.));
#16628=DIRECTION('',(0.,0.,1.));
#16629=DIRECTION('',(-0.382683432365089,0.,-0.923879532511287));
#16630=DIRECTION('',(0.991444861373811,0.,0.130526192220051));
#16631=DIRECTION('',(0.,1.,0.));
#16632=DIRECTION('',(0.,0.,1.));
#16633=DIRECTION('',(-0.258819045102521,0.,-0.965925826289068));
#16634=DIRECTION('',(0.965925826289069,0.,0.25881904510252));
#16635=DIRECTION('',(0.,1.,0.));
#16636=DIRECTION('',(0.,0.,1.));
#16637=DIRECTION('',(-0.130526192220051,0.,-0.99144486137381));
#16638=DIRECTION('',(0.923879532511287,0.,0.382683432365089));
#16639=DIRECTION('',(0.,1.,0.));
#16640=DIRECTION('',(0.,0.,1.));
#16641=DIRECTION('',(7.36963889557083E-16,0.,-1.));
#16642=DIRECTION('',(0.866025403784439,0.,0.5));
#16643=DIRECTION('',(0.,1.,0.));
#16644=DIRECTION('',(0.,0.,1.));
#16645=DIRECTION('',(0.130526192220052,0.,-0.99144486137381));
#16646=DIRECTION('',(0.793353340291236,0.,0.608761429008719));
#16647=DIRECTION('',(0.,1.,0.));
#16648=DIRECTION('',(0.,0.,1.));
#16649=DIRECTION('',(0.258819045102521,0.,-0.965925826289068));
#16650=DIRECTION('',(0.707106781186549,0.,0.707106781186547));
#16651=DIRECTION('',(0.,1.,0.));
#16652=DIRECTION('',(0.,0.,1.));
#16653=DIRECTION('',(0.38268343236509,0.,-0.923879532511287));
#16654=DIRECTION('',(0.608761429008721,0.,0.793353340291235));
#16655=DIRECTION('',(0.,1.,0.));
#16656=DIRECTION('',(0.,0.,1.));
#16657=DIRECTION('',(0.5,0.,-0.866025403784439));
#16658=DIRECTION('',(0.5,0.,0.866025403784438));
#16659=DIRECTION('',(0.,1.,0.));
#16660=DIRECTION('',(0.,0.,1.));
#16661=DIRECTION('',(0.608761429008722,0.,-0.793353340291234));
#16662=DIRECTION('',(0.382683432365091,0.,0.923879532511286));
#16663=DIRECTION('',(0.,1.,0.));
#16664=DIRECTION('',(0.,0.,1.));
#16665=DIRECTION('',(0.707106781186548,0.,-0.707106781186548));
#16666=DIRECTION('',(0.258819045102522,0.,0.965925826289068));
#16667=DIRECTION('',(0.,1.,0.));
#16668=DIRECTION('',(0.,0.,1.));
#16669=DIRECTION('',(0.793353340291235,0.,-0.608761429008721));
#16670=DIRECTION('',(0.130526192220053,0.,0.99144486137381));
#16671=DIRECTION('',(0.,1.,0.));
#16672=DIRECTION('',(0.,0.,1.));
#16673=DIRECTION('',(0.866025403784439,0.,-0.5));
#16674=DIRECTION('',(1.47392777911416E-15,0.,1.));
#16675=DIRECTION('',(0.,1.,0.));
#16676=DIRECTION('',(0.,0.,1.));
#16677=DIRECTION('',(0.923879532511287,0.,-0.38268343236509));
#16678=DIRECTION('',(-0.130526192220051,0.,0.991444861373811));
#16679=DIRECTION('',(0.,1.,0.));
#16680=DIRECTION('',(0.,0.,1.));
#16681=DIRECTION('',(0.965925826289068,0.,-0.258819045102521));
#16682=DIRECTION('',(-0.258819045102519,0.,0.965925826289069));
#16683=DIRECTION('',(0.,1.,0.));
#16684=DIRECTION('',(0.,0.,1.));
#16685=DIRECTION('',(0.99144486137381,0.,-0.130526192220052));
#16686=DIRECTION('',(-0.382683432365088,0.,0.923879532511288));
#16687=DIRECTION('',(0.,1.,0.));
#16688=DIRECTION('',(0.,0.,1.));
#16689=DIRECTION('',(1.,0.,0.));
#16690=DIRECTION('',(-0.5,0.,0.86602540378444));
#16691=DIRECTION('',(0.,1.,0.));
#16692=DIRECTION('',(0.,0.,1.));
#16693=DIRECTION('',(0.99144486137381,0.,0.130526192220052));
#16694=DIRECTION('',(-0.608761429008719,0.,0.793353340291236));
#16695=DIRECTION('',(0.,1.,0.));
#16696=DIRECTION('',(0.,0.,1.));
#16697=DIRECTION('',(0.965925826289068,0.,0.258819045102521));
#16698=DIRECTION('',(-0.707106781186546,0.,0.707106781186549));
#16699=DIRECTION('',(0.,1.,0.));
#16700=DIRECTION('',(0.,0.,1.));
#16701=DIRECTION('',(0.923879532511287,0.,0.382683432365089));
#16702=DIRECTION('',(-0.793353340291235,0.,0.608761429008721));
#16703=DIRECTION('',(0.,1.,0.));
#16704=DIRECTION('',(0.,0.,1.));
#16705=DIRECTION('',(0.866025403784439,0.,0.5));
#16706=DIRECTION('',(-0.866025403784438,0.,0.5));
#16707=DIRECTION('',(0.,1.,0.));
#16708=DIRECTION('',(0.,0.,1.));
#16709=DIRECTION('',(0.793353340291235,0.,0.608761429008722));
#16710=DIRECTION('',(-0.923879532511286,0.,0.382683432365092));
#16711=DIRECTION('',(0.,1.,0.));
#16712=DIRECTION('',(0.,0.,1.));
#16713=DIRECTION('',(0.707106781186548,0.,0.707106781186547));
#16714=DIRECTION('',(-0.965925826289068,0.,0.258819045102523));
#16715=DIRECTION('',(0.,1.,0.));
#16716=DIRECTION('',(0.,0.,1.));
#16717=DIRECTION('',(0.608761429008721,0.,0.793353340291235));
#16718=DIRECTION('',(-0.99144486137381,0.,0.130526192220053));
#16719=DIRECTION('',(0.,1.,0.));
#16720=DIRECTION('',(0.,0.,1.));
#16721=DIRECTION('',(0.5,0.,0.866025403784439));
#16722=DIRECTION('',(-1.,0.,1.47392777911416E-15));
#16723=DIRECTION('',(0.,1.,0.));
#16724=DIRECTION('',(0.,0.,1.));
#16725=DIRECTION('',(0.38268343236509,0.,0.923879532511287));
#16726=DIRECTION('',(-0.991444861373811,0.,-0.130526192220051));
#16727=DIRECTION('',(0.,1.,0.));
#16728=DIRECTION('',(0.,0.,1.));
#16729=DIRECTION('',(0.258819045102521,0.,0.965925826289068));
#16730=DIRECTION('',(-0.965925826289069,0.,-0.258819045102519));
#16731=DIRECTION('',(0.,1.,0.));
#16732=DIRECTION('',(0.,0.,1.));
#16733=DIRECTION('',(0.130526192220052,0.,0.99144486137381));
#16734=DIRECTION('',(-0.923879532511288,0.,-0.382683432365088));
#16735=DIRECTION('',(0.,1.,0.));
#16736=DIRECTION('',(0.,0.,1.));
#16737=DIRECTION('',(-7.36963889557083E-16,0.,1.));
#16738=DIRECTION('',(-0.86602540378444,0.,-0.5));
#16739=DIRECTION('',(0.,1.,0.));
#16740=DIRECTION('',(0.,0.,1.));
#16741=DIRECTION('',(-0.130526192220052,0.,0.99144486137381));
#16742=DIRECTION('',(-0.793353340291236,0.,-0.608761429008719));
#16743=DIRECTION('',(0.,1.,0.));
#16744=DIRECTION('',(0.,0.,1.));
#16745=DIRECTION('',(-0.25881904510252,0.,0.965925826289068));
#16746=DIRECTION('',(-0.707106781186549,0.,-0.707106781186546));
#16747=DIRECTION('',(0.,1.,0.));
#16748=DIRECTION('',(0.,0.,1.));
#16749=DIRECTION('',(-0.38268343236509,0.,0.923879532511287));
#16750=DIRECTION('',(-0.608761429008723,0.,-0.793353340291234));
#16751=DIRECTION('',(0.,1.,0.));
#16752=DIRECTION('',(0.,0.,1.));
#16753=DIRECTION('',(-0.5,0.,0.866025403784439));
#16754=DIRECTION('',(-0.5,0.,-0.866025403784438));
#16755=DIRECTION('',(0.,1.,0.));
#16756=DIRECTION('',(0.,0.,1.));
#16757=DIRECTION('',(-0.608761429008721,0.,0.793353340291235));
#16758=DIRECTION('',(-0.382683432365092,0.,-0.923879532511286));
#16759=DIRECTION('',(0.,1.,0.));
#16760=DIRECTION('',(0.,0.,1.));
#16761=DIRECTION('',(-0.707106781186548,0.,0.707106781186548));
#16762=DIRECTION('',(-0.258819045102522,0.,-0.965925826289068));
#16763=DIRECTION('',(0.,1.,0.));
#16764=DIRECTION('',(0.,0.,1.));
#16765=DIRECTION('',(-0.793353340291235,0.,0.608761429008721));
#16766=DIRECTION('',(-0.130526192220053,0.,-0.99144486137381));
#16767=DIRECTION('',(0.,1.,0.));
#16768=DIRECTION('',(0.,0.,1.));
#16769=DIRECTION('',(-0.866025403784439,0.,0.5));
#16770=DIRECTION('',(-2.21089166867125E-15,0.,-1.));
#16771=DIRECTION('',(0.,1.,0.));
#16772=DIRECTION('',(0.,0.,1.));
#16773=DIRECTION('',(-0.923879532511287,0.,0.382683432365091));
#16774=DIRECTION('',(0.13052619222005,0.,-0.991444861373811));
#16775=DIRECTION('',(0.,1.,0.));
#16776=DIRECTION('',(0.,0.,1.));
#16777=DIRECTION('',(-0.965925826289068,0.,0.258819045102521));
#16778=DIRECTION('',(0.258819045102519,0.,-0.965925826289069));
#16779=DIRECTION('',(0.,1.,0.));
#16780=DIRECTION('',(0.,0.,1.));
#16781=DIRECTION('',(-0.99144486137381,0.,0.130526192220052));
#16782=DIRECTION('',(0.382476066482387,0.,-0.923965399010245));
#16783=DIRECTION('',(-1.,0.,-7.36963889557082E-16));
#16784=DIRECTION('',(0.5,0.,-0.866025403784439));
#16785=DIRECTION('',(0.,1.,0.));
#16786=DIRECTION('',(0.,0.,1.));
#16787=DIRECTION('',(-0.99144486137381,0.,-0.130526192220051));
#16788=DIRECTION('',(0.608761429008719,0.,-0.793353340291237));
#16789=DIRECTION('',(0.,1.,0.));
#16790=DIRECTION('',(0.,0.,1.));
#16791=DIRECTION('',(-0.965925826289068,0.,-0.258819045102521));
#16792=DIRECTION('',(0.707106781186546,0.,-0.707106781186549));
#16793=DIRECTION('',(0.,1.,0.));
#16794=DIRECTION('',(0.,0.,1.));
#16795=DIRECTION('',(-0.923879532511287,0.,-0.38268343236509));
#16796=DIRECTION('',(0.793353340291234,0.,-0.608761429008723));
#16797=DIRECTION('',(0.,1.,0.));
#16798=DIRECTION('',(0.,0.,1.));
#16799=DIRECTION('',(-0.866025403784438,0.,-0.5));
#16800=DIRECTION('',(0.,-1.,0.));
#16801=DIRECTION('',(0.,0.,-1.));
#16802=DIRECTION('',(0.,1.,0.));
#16803=DIRECTION('',(0.,0.,1.));
#16804=DIRECTION('',(0.86602540378444,0.,-0.5));
#16805=DIRECTION('',(-0.866025403784438,0.,-0.5));
#16806=DIRECTION('',(0.,1.,0.));
#16807=DIRECTION('',(0.,0.,1.));
#16808=DIRECTION('',(0.793353340291234,0.,-0.608761429008723));
#16809=DIRECTION('',(-0.923879532511287,0.,-0.38268343236509));
#16810=DIRECTION('',(0.,1.,0.));
#16811=DIRECTION('',(0.,0.,1.));
#16812=DIRECTION('',(0.707106781186546,0.,-0.707106781186549));
#16813=DIRECTION('',(-0.965925826289068,0.,-0.258819045102521));
#16814=DIRECTION('',(0.,1.,0.));
#16815=DIRECTION('',(0.,0.,1.));
#16816=DIRECTION('',(0.608761429008719,0.,-0.793353340291237));
#16817=DIRECTION('',(-0.99144486137381,0.,-0.130526192220051));
#16818=DIRECTION('',(0.,1.,0.));
#16819=DIRECTION('',(0.,0.,1.));
#16820=DIRECTION('',(0.5,0.,-0.866025403784439));
#16821=DIRECTION('',(-1.,0.,-7.36963889557082E-16));
#16822=DIRECTION('',(0.382476066482387,0.,-0.923965399010245));
#16823=DIRECTION('',(-0.99144486137381,0.,0.130526192220052));
#16824=DIRECTION('',(0.,1.,0.));
#16825=DIRECTION('',(0.,0.,1.));
#16826=DIRECTION('',(0.258819045102519,0.,-0.965925826289069));
#16827=DIRECTION('',(-0.965925826289068,0.,0.258819045102521));
#16828=DIRECTION('',(0.,1.,0.));
#16829=DIRECTION('',(0.,0.,1.));
#16830=DIRECTION('',(0.13052619222005,0.,-0.991444861373811));
#16831=DIRECTION('',(-0.923879532511287,0.,0.382683432365091));
#16832=DIRECTION('',(0.,1.,0.));
#16833=DIRECTION('',(0.,0.,1.));
#16834=DIRECTION('',(-2.21089166867125E-15,0.,-1.));
#16835=DIRECTION('',(-0.866025403784439,0.,0.5));
#16836=DIRECTION('',(0.,1.,0.));
#16837=DIRECTION('',(0.,0.,1.));
#16838=DIRECTION('',(-0.130526192220053,0.,-0.99144486137381));
#16839=DIRECTION('',(-0.793353340291235,0.,0.608761429008721));
#16840=DIRECTION('',(0.,1.,0.));
#16841=DIRECTION('',(0.,0.,1.));
#16842=DIRECTION('',(-0.258819045102522,0.,-0.965925826289068));
#16843=DIRECTION('',(-0.707106781186548,0.,0.707106781186548));
#16844=DIRECTION('',(0.,1.,0.));
#16845=DIRECTION('',(0.,0.,1.));
#16846=DIRECTION('',(-0.382683432365092,0.,-0.923879532511286));
#16847=DIRECTION('',(-0.608761429008721,0.,0.793353340291235));
#16848=DIRECTION('',(0.,1.,0.));
#16849=DIRECTION('',(0.,0.,1.));
#16850=DIRECTION('',(-0.5,0.,-0.866025403784438));
#16851=DIRECTION('',(-0.5,0.,0.866025403784439));
#16852=DIRECTION('',(0.,1.,0.));
#16853=DIRECTION('',(0.,0.,1.));
#16854=DIRECTION('',(-0.608761429008723,0.,-0.793353340291234));
#16855=DIRECTION('',(-0.38268343236509,0.,0.923879532511287));
#16856=DIRECTION('',(0.,1.,0.));
#16857=DIRECTION('',(0.,0.,1.));
#16858=DIRECTION('',(-0.707106781186549,0.,-0.707106781186546));
#16859=DIRECTION('',(-0.25881904510252,0.,0.965925826289068));
#16860=DIRECTION('',(0.,1.,0.));
#16861=DIRECTION('',(0.,0.,1.));
#16862=DIRECTION('',(-0.793353340291236,0.,-0.608761429008719));
#16863=DIRECTION('',(-0.130526192220052,0.,0.99144486137381));
#16864=DIRECTION('',(0.,1.,0.));
#16865=DIRECTION('',(0.,0.,1.));
#16866=DIRECTION('',(-0.86602540378444,0.,-0.5));
#16867=DIRECTION('',(-7.36963889557083E-16,0.,1.));
#16868=DIRECTION('',(0.,1.,0.));
#16869=DIRECTION('',(0.,0.,1.));
#16870=DIRECTION('',(-0.923879532511288,0.,-0.382683432365088));
#16871=DIRECTION('',(0.130526192220052,0.,0.99144486137381));
#16872=DIRECTION('',(0.,1.,0.));
#16873=DIRECTION('',(0.,0.,1.));
#16874=DIRECTION('',(-0.965925826289069,0.,-0.258819045102519));
#16875=DIRECTION('',(0.258819045102521,0.,0.965925826289068));
#16876=DIRECTION('',(0.,1.,0.));
#16877=DIRECTION('',(0.,0.,1.));
#16878=DIRECTION('',(-0.991444861373811,0.,-0.130526192220051));
#16879=DIRECTION('',(0.38268343236509,0.,0.923879532511287));
#16880=DIRECTION('',(0.,1.,0.));
#16881=DIRECTION('',(0.,0.,1.));
#16882=DIRECTION('',(-1.,0.,1.47392777911416E-15));
#16883=DIRECTION('',(0.5,0.,0.866025403784439));
#16884=DIRECTION('',(0.,1.,0.));
#16885=DIRECTION('',(0.,0.,1.));
#16886=DIRECTION('',(-0.99144486137381,0.,0.130526192220053));
#16887=DIRECTION('',(0.608761429008721,0.,0.793353340291235));
#16888=DIRECTION('',(0.,1.,0.));
#16889=DIRECTION('',(0.,0.,1.));
#16890=DIRECTION('',(-0.965925826289068,0.,0.258819045102523));
#16891=DIRECTION('',(0.707106781186548,0.,0.707106781186547));
#16892=DIRECTION('',(0.,1.,0.));
#16893=DIRECTION('',(0.,0.,1.));
#16894=DIRECTION('',(-0.923879532511286,0.,0.382683432365092));
#16895=DIRECTION('',(0.793353340291235,0.,0.608761429008722));
#16896=DIRECTION('',(0.,1.,0.));
#16897=DIRECTION('',(0.,0.,1.));
#16898=DIRECTION('',(-0.866025403784438,0.,0.5));
#16899=DIRECTION('',(0.866025403784439,0.,0.5));
#16900=DIRECTION('',(0.,1.,0.));
#16901=DIRECTION('',(0.,0.,1.));
#16902=DIRECTION('',(-0.793353340291235,0.,0.608761429008721));
#16903=DIRECTION('',(0.923879532511287,0.,0.382683432365089));
#16904=DIRECTION('',(0.,1.,0.));
#16905=DIRECTION('',(0.,0.,1.));
#16906=DIRECTION('',(-0.707106781186546,0.,0.707106781186549));
#16907=DIRECTION('',(0.965925826289068,0.,0.258819045102521));
#16908=DIRECTION('',(0.,1.,0.));
#16909=DIRECTION('',(0.,0.,1.));
#16910=DIRECTION('',(-0.608761429008719,0.,0.793353340291236));
#16911=DIRECTION('',(0.99144486137381,0.,0.130526192220052));
#16912=DIRECTION('',(0.,1.,0.));
#16913=DIRECTION('',(0.,0.,1.));
#16914=DIRECTION('',(-0.5,0.,0.86602540378444));
#16915=DIRECTION('',(1.,0.,0.));
#16916=DIRECTION('',(0.,1.,0.));
#16917=DIRECTION('',(0.,0.,1.));
#16918=DIRECTION('',(-0.382683432365088,0.,0.923879532511288));
#16919=DIRECTION('',(0.99144486137381,0.,-0.130526192220052));
#16920=DIRECTION('',(0.,1.,0.));
#16921=DIRECTION('',(0.,0.,1.));
#16922=DIRECTION('',(-0.258819045102519,0.,0.965925826289069));
#16923=DIRECTION('',(0.965925826289068,0.,-0.258819045102521));
#16924=DIRECTION('',(0.,1.,0.));
#16925=DIRECTION('',(0.,0.,1.));
#16926=DIRECTION('',(-0.130526192220051,0.,0.991444861373811));
#16927=DIRECTION('',(0.923879532511287,0.,-0.38268343236509));
#16928=DIRECTION('',(0.,1.,0.));
#16929=DIRECTION('',(0.,0.,1.));
#16930=DIRECTION('',(1.47392777911416E-15,0.,1.));
#16931=DIRECTION('',(0.866025403784439,0.,-0.5));
#16932=DIRECTION('',(0.,1.,0.));
#16933=DIRECTION('',(0.,0.,1.));
#16934=DIRECTION('',(0.130526192220053,0.,0.99144486137381));
#16935=DIRECTION('',(0.793353340291235,0.,-0.608761429008721));
#16936=DIRECTION('',(0.,1.,0.));
#16937=DIRECTION('',(0.,0.,1.));
#16938=DIRECTION('',(0.258819045102522,0.,0.965925826289068));
#16939=DIRECTION('',(0.707106781186548,0.,-0.707106781186548));
#16940=DIRECTION('',(0.,1.,0.));
#16941=DIRECTION('',(0.,0.,1.));
#16942=DIRECTION('',(0.382683432365091,0.,0.923879532511286));
#16943=DIRECTION('',(0.608761429008722,0.,-0.793353340291234));
#16944=DIRECTION('',(0.,1.,0.));
#16945=DIRECTION('',(0.,0.,1.));
#16946=DIRECTION('',(0.5,0.,0.866025403784438));
#16947=DIRECTION('',(0.5,0.,-0.866025403784439));
#16948=DIRECTION('',(0.,1.,0.));
#16949=DIRECTION('',(0.,0.,1.));
#16950=DIRECTION('',(0.608761429008721,0.,0.793353340291235));
#16951=DIRECTION('',(0.38268343236509,0.,-0.923879532511287));
#16952=DIRECTION('',(0.,1.,0.));
#16953=DIRECTION('',(0.,0.,1.));
#16954=DIRECTION('',(0.707106781186549,0.,0.707106781186547));
#16955=DIRECTION('',(0.258819045102521,0.,-0.965925826289068));
#16956=DIRECTION('',(0.,1.,0.));
#16957=DIRECTION('',(0.,0.,1.));
#16958=DIRECTION('',(0.793353340291236,0.,0.608761429008719));
#16959=DIRECTION('',(0.130526192220052,0.,-0.99144486137381));
#16960=DIRECTION('',(0.,1.,0.));
#16961=DIRECTION('',(0.,0.,1.));
#16962=DIRECTION('',(0.866025403784439,0.,0.5));
#16963=DIRECTION('',(7.36963889557083E-16,0.,-1.));
#16964=DIRECTION('',(0.,1.,0.));
#16965=DIRECTION('',(0.,0.,1.));
#16966=DIRECTION('',(0.923879532511287,0.,0.382683432365089));
#16967=DIRECTION('',(-0.130526192220051,0.,-0.99144486137381));
#16968=DIRECTION('',(0.,1.,0.));
#16969=DIRECTION('',(0.,0.,1.));
#16970=DIRECTION('',(0.965925826289069,0.,0.25881904510252));
#16971=DIRECTION('',(-0.258819045102521,0.,-0.965925826289068));
#16972=DIRECTION('',(0.,1.,0.));
#16973=DIRECTION('',(0.,0.,1.));
#16974=DIRECTION('',(0.991444861373811,0.,0.130526192220051));
#16975=DIRECTION('',(-0.382683432365089,0.,-0.923879532511287));
#16976=DIRECTION('',(0.,1.,0.));
#16977=DIRECTION('',(0.,0.,1.));
#16978=DIRECTION('',(1.,0.,-1.47392777911416E-15));
#16979=DIRECTION('',(-0.5,0.,-0.866025403784439));
#16980=DIRECTION('',(0.,1.,0.));
#16981=DIRECTION('',(0.,0.,1.));
#16982=DIRECTION('',(0.99144486137381,0.,-0.130526192220053));
#16983=DIRECTION('',(-0.60876142900872,0.,-0.793353340291235));
#16984=DIRECTION('',(0.,1.,0.));
#16985=DIRECTION('',(0.,0.,1.));
#16986=DIRECTION('',(0.965925826289068,0.,-0.258819045102522));
#16987=DIRECTION('',(-0.707106781186548,0.,-0.707106781186548));
#16988=DIRECTION('',(0.,1.,0.));
#16989=DIRECTION('',(0.,0.,1.));
#16990=DIRECTION('',(0.923879532511287,0.,-0.382683432365091));
#16991=DIRECTION('',(-0.793353340291235,0.,-0.608761429008721));
#16992=DIRECTION('',(0.,1.,0.));
#16993=DIRECTION('',(0.,0.,1.));
#16994=DIRECTION('',(0.,1.,0.));
#16995=DIRECTION('',(0.,0.,1.));
#16996=DIRECTION('',(0.,-1.,0.));
#16997=DIRECTION('',(0.,0.,-1.));
#16998=DIRECTION('',(0.,-1.,0.));
#16999=DIRECTION('',(0.,-1.,0.));
#17000=DIRECTION('',(-0.608761429008719,0.,0.793353340291236));
#17001=DIRECTION('',(0.793353340291236,0.,0.608761429008719));
#17002=DIRECTION('',(0.,-1.,0.));
#17003=DIRECTION('',(-0.38268343236509,0.,-0.923879532511287));
#17004=DIRECTION('',(-0.923879532511287,0.,0.38268343236509));
#17005=DIRECTION('',(0.,-1.,0.));
#17006=DIRECTION('',(0.,-1.,0.));
#17007=DIRECTION('',(0.,0.,-1.));
#17008=DIRECTION('',(0.,-1.,0.));
#17009=DIRECTION('',(-0.707106781186548,0.,0.707106781186548));
#17010=DIRECTION('',(0.707106781186548,0.,0.707106781186548));
#17011=DIRECTION('',(0.,-1.,0.));
#17012=DIRECTION('',(-0.258819045102521,0.,-0.965925826289068));
#17013=DIRECTION('',(-0.965925826289068,0.,0.258819045102521));
#17014=DIRECTION('',(0.,-1.,0.));
#17015=DIRECTION('',(0.,-1.,0.));
#17016=DIRECTION('',(0.,0.,-1.));
#17017=DIRECTION('',(0.,-1.,0.));
#17018=DIRECTION('',(-0.793353340291234,0.,0.608761429008723));
#17019=DIRECTION('',(0.608761429008723,0.,0.793353340291234));
#17020=DIRECTION('',(0.,-1.,0.));
#17021=DIRECTION('',(-0.130526192220052,0.,-0.99144486137381));
#17022=DIRECTION('',(-0.99144486137381,0.,0.130526192220052));
#17023=DIRECTION('',(0.,-1.,0.));
#17024=DIRECTION('',(0.,-1.,0.));
#17025=DIRECTION('',(0.,0.,-1.));
#17026=DIRECTION('',(0.,-1.,0.));
#17027=DIRECTION('',(-0.866025403784438,0.,0.5));
#17028=DIRECTION('',(0.5,0.,0.866025403784438));
#17029=DIRECTION('',(0.,-1.,0.));
#17030=DIRECTION('',(0.,0.,-1.));
#17031=DIRECTION('',(-1.,0.,0.));
#17032=DIRECTION('',(0.,-1.,0.));
#17033=DIRECTION('',(0.,-1.,0.));
#17034=DIRECTION('',(0.,0.,-1.));
#17035=DIRECTION('',(0.,-1.,0.));
#17036=DIRECTION('',(-0.923879532511286,0.,0.382683432365092));
#17037=DIRECTION('',(0.382683432365092,0.,0.923879532511286));
#17038=DIRECTION('',(0.,-1.,0.));
#17039=DIRECTION('',(0.130526192220052,0.,-0.99144486137381));
#17040=DIRECTION('',(-0.99144486137381,0.,-0.130526192220052));
#17041=DIRECTION('',(0.,-1.,0.));
#17042=DIRECTION('',(0.,-1.,0.));
#17043=DIRECTION('',(0.,0.,-1.));
#17044=DIRECTION('',(0.,-1.,0.));
#17045=DIRECTION('',(-0.965925826289068,0.,0.258819045102521));
#17046=DIRECTION('',(0.258819045102521,0.,0.965925826289068));
#17047=DIRECTION('',(0.,-1.,0.));
#17048=DIRECTION('',(0.258819045102521,0.,-0.965925826289068));
#17049=DIRECTION('',(-0.965925826289068,0.,-0.258819045102521));
#17050=DIRECTION('',(0.,-1.,0.));
#17051=DIRECTION('',(0.,-1.,0.));
#17052=DIRECTION('',(0.,0.,-1.));
#17053=DIRECTION('',(0.,-1.,0.));
#17054=DIRECTION('',(-0.99144486137381,0.,0.130526192220051));
#17055=DIRECTION('',(0.130526192220051,0.,0.99144486137381));
#17056=DIRECTION('',(0.,-1.,0.));
#17057=DIRECTION('',(0.382683432365089,0.,-0.923879532511287));
#17058=DIRECTION('',(-0.923879532511287,0.,-0.382683432365089));
#17059=DIRECTION('',(0.,-1.,0.));
#17060=DIRECTION('',(0.,-1.,0.));
#17061=DIRECTION('',(0.,0.,-1.));
#17062=DIRECTION('',(0.,-1.,0.));
#17063=DIRECTION('',(-1.,0.,0.));
#17064=DIRECTION('',(0.,0.,1.));
#17065=DIRECTION('',(0.,-1.,0.));
#17066=DIRECTION('',(0.5,0.,-0.866025403784439));
#17067=DIRECTION('',(-0.866025403784439,0.,-0.5));
#17068=DIRECTION('',(0.,-1.,0.));
#17069=DIRECTION('',(0.,-1.,0.));
#17070=DIRECTION('',(0.,0.,-1.));
#17071=DIRECTION('',(0.,-1.,0.));
#17072=DIRECTION('',(-0.99144486137381,0.,-0.130526192220052));
#17073=DIRECTION('',(-0.130526192220052,0.,0.99144486137381));
#17074=DIRECTION('',(0.,-1.,0.));
#17075=DIRECTION('',(0.608761429008722,0.,-0.793353340291235));
#17076=DIRECTION('',(-0.793353340291235,0.,-0.608761429008722));
#17077=DIRECTION('',(0.,-1.,0.));
#17078=DIRECTION('',(0.,-1.,0.));
#17079=DIRECTION('',(0.,0.,-1.));
#17080=DIRECTION('',(0.,-1.,0.));
#17081=DIRECTION('',(-0.965925826289068,0.,-0.258819045102521));
#17082=DIRECTION('',(-0.258819045102521,0.,0.965925826289068));
#17083=DIRECTION('',(0.,-1.,0.));
#17084=DIRECTION('',(0.707106781186548,0.,-0.707106781186548));
#17085=DIRECTION('',(-0.707106781186548,0.,-0.707106781186548));
#17086=DIRECTION('',(0.,-1.,0.));
#17087=DIRECTION('',(0.,-1.,0.));
#17088=DIRECTION('',(0.,0.,-1.));
#17089=DIRECTION('',(0.,-1.,0.));
#17090=DIRECTION('',(-0.923879532511287,0.,-0.38268343236509));
#17091=DIRECTION('',(-0.38268343236509,0.,0.923879532511287));
#17092=DIRECTION('',(0.,-1.,0.));
#17093=DIRECTION('',(0.793353340291235,0.,-0.608761429008721));
#17094=DIRECTION('',(-0.608761429008721,0.,-0.793353340291235));
#17095=DIRECTION('',(0.,-1.,0.));
#17096=DIRECTION('',(0.,-1.,0.));
#17097=DIRECTION('',(0.,0.,-1.));
#17098=DIRECTION('',(0.,-1.,0.));
#17099=DIRECTION('',(-0.866025403784439,0.,-0.5));
#17100=DIRECTION('',(-0.5,0.,0.866025403784439));
#17101=DIRECTION('',(0.,-1.,0.));
#17102=DIRECTION('',(0.866025403784439,0.,-0.5));
#17103=DIRECTION('',(-0.5,0.,-0.866025403784439));
#17104=DIRECTION('',(0.,-1.,0.));
#17105=DIRECTION('',(0.,-1.,0.));
#17106=DIRECTION('',(0.,0.,-1.));
#17107=DIRECTION('',(0.,-1.,0.));
#17108=DIRECTION('',(-0.793353340291234,0.,-0.608761429008722));
#17109=DIRECTION('',(-0.608761429008722,0.,0.793353340291234));
#17110=DIRECTION('',(0.,-1.,0.));
#17111=DIRECTION('',(0.923879532511287,0.,-0.38268343236509));
#17112=DIRECTION('',(-0.38268343236509,0.,-0.923879532511287));
#17113=DIRECTION('',(0.,-1.,0.));
#17114=DIRECTION('',(0.,-1.,0.));
#17115=DIRECTION('',(0.,0.,-1.));
#17116=DIRECTION('',(0.,-1.,0.));
#17117=DIRECTION('',(-0.707106781186548,0.,-0.707106781186548));
#17118=DIRECTION('',(-0.707106781186548,0.,0.707106781186548));
#17119=DIRECTION('',(0.,-1.,0.));
#17120=DIRECTION('',(0.965925826289068,0.,-0.258819045102522));
#17121=DIRECTION('',(-0.258819045102522,0.,-0.965925826289068));
#17122=DIRECTION('',(0.,-1.,0.));
#17123=DIRECTION('',(0.,-1.,0.));
#17124=DIRECTION('',(0.,0.,-1.));
#17125=DIRECTION('',(0.,-1.,0.));
#17126=DIRECTION('',(-0.608761429008721,0.,-0.793353340291235));
#17127=DIRECTION('',(-0.793353340291235,0.,0.608761429008721));
#17128=DIRECTION('',(0.,-1.,0.));
#17129=DIRECTION('',(0.99144486137381,0.,-0.130526192220053));
#17130=DIRECTION('',(-0.130526192220053,0.,-0.99144486137381));
#17131=DIRECTION('',(0.,-1.,0.));
#17132=DIRECTION('',(0.,-1.,0.));
#17133=DIRECTION('',(0.,0.,-1.));
#17134=DIRECTION('',(0.,-1.,0.));
#17135=DIRECTION('',(-0.5,0.,-0.866025403784439));
#17136=DIRECTION('',(-0.866025403784439,0.,0.5));
#17137=DIRECTION('',(0.,-1.,0.));
#17138=DIRECTION('',(1.,0.,0.));
#17139=DIRECTION('',(0.,0.,-1.));
#17140=DIRECTION('',(0.,-1.,0.));
#17141=DIRECTION('',(0.,-1.,0.));
#17142=DIRECTION('',(0.,0.,-1.));
#17143=DIRECTION('',(0.,-1.,0.));
#17144=DIRECTION('',(-0.38268343236509,0.,-0.923879532511287));
#17145=DIRECTION('',(-0.923879532511287,0.,0.38268343236509));
#17146=DIRECTION('',(0.,-1.,0.));
#17147=DIRECTION('',(0.991444861373811,0.,0.130526192220051));
#17148=DIRECTION('',(0.130526192220051,0.,-0.991444861373811));
#17149=DIRECTION('',(0.,-1.,0.));
#17150=DIRECTION('',(0.,-1.,0.));
#17151=DIRECTION('',(0.,0.,-1.));
#17152=DIRECTION('',(0.,-1.,0.));
#17153=DIRECTION('',(-0.258819045102521,0.,-0.965925826289068));
#17154=DIRECTION('',(-0.965925826289068,0.,0.258819045102521));
#17155=DIRECTION('',(0.,-1.,0.));
#17156=DIRECTION('',(0.965925826289069,0.,0.258819045102519));
#17157=DIRECTION('',(0.258819045102519,0.,-0.965925826289069));
#17158=DIRECTION('',(0.,-1.,0.));
#17159=DIRECTION('',(0.,-1.,0.));
#17160=DIRECTION('',(0.,0.,-1.));
#17161=DIRECTION('',(0.,-1.,0.));
#17162=DIRECTION('',(-0.130526192220052,0.,-0.99144486137381));
#17163=DIRECTION('',(-0.99144486137381,0.,0.130526192220052));
#17164=DIRECTION('',(0.,-1.,0.));
#17165=DIRECTION('',(0.923879532511288,0.,0.382683432365088));
#17166=DIRECTION('',(0.382683432365088,0.,-0.923879532511288));
#17167=DIRECTION('',(0.,-1.,0.));
#17168=DIRECTION('',(0.,-1.,0.));
#17169=DIRECTION('',(0.,0.,-1.));
#17170=DIRECTION('',(0.,-1.,0.));
#17171=DIRECTION('',(0.,0.,-1.));
#17172=DIRECTION('',(-1.,0.,0.));
#17173=DIRECTION('',(0.,-1.,0.));
#17174=DIRECTION('',(0.86602540378444,0.,0.5));
#17175=DIRECTION('',(0.5,0.,-0.86602540378444));
#17176=DIRECTION('',(0.,-1.,0.));
#17177=DIRECTION('',(0.,-1.,0.));
#17178=DIRECTION('',(0.,0.,-1.));
#17179=DIRECTION('',(0.,-1.,0.));
#17180=DIRECTION('',(0.130526192220052,0.,-0.99144486137381));
#17181=DIRECTION('',(-0.99144486137381,0.,-0.130526192220052));
#17182=DIRECTION('',(0.,-1.,0.));
#17183=DIRECTION('',(0.793353340291236,0.,0.608761429008719));
#17184=DIRECTION('',(0.608761429008719,0.,-0.793353340291236));
#17185=DIRECTION('',(0.,-1.,0.));
#17186=DIRECTION('',(0.,-1.,0.));
#17187=DIRECTION('',(0.,0.,-1.));
#17188=DIRECTION('',(0.,-1.,0.));
#17189=DIRECTION('',(0.258819045102521,0.,-0.965925826289068));
#17190=DIRECTION('',(-0.965925826289068,0.,-0.258819045102521));
#17191=DIRECTION('',(0.,-1.,0.));
#17192=DIRECTION('',(0.707106781186549,0.,0.707106781186546));
#17193=DIRECTION('',(0.707106781186546,0.,-0.707106781186549));
#17194=DIRECTION('',(0.,-1.,0.));
#17195=DIRECTION('',(0.,-1.,0.));
#17196=DIRECTION('',(0.,0.,-1.));
#17197=DIRECTION('',(0.,-1.,0.));
#17198=DIRECTION('',(0.382683432365089,0.,-0.923879532511287));
#17199=DIRECTION('',(-0.923879532511287,0.,-0.382683432365089));
#17200=DIRECTION('',(0.,-1.,0.));
#17201=DIRECTION('',(0.608761429008721,0.,0.793353340291235));
#17202=DIRECTION('',(0.793353340291235,0.,-0.608761429008721));
#17203=DIRECTION('',(0.,-1.,0.));
#17204=DIRECTION('',(0.,-1.,0.));
#17205=DIRECTION('',(0.,0.,-1.));
#17206=DIRECTION('',(0.,-1.,0.));
#17207=DIRECTION('',(0.5,0.,-0.866025403784439));
#17208=DIRECTION('',(-0.866025403784439,0.,-0.5));
#17209=DIRECTION('',(0.,-1.,0.));
#17210=DIRECTION('',(0.5,0.,0.866025403784438));
#17211=DIRECTION('',(0.866025403784438,0.,-0.5));
#17212=DIRECTION('',(0.,-1.,0.));
#17213=DIRECTION('',(0.,-1.,0.));
#17214=DIRECTION('',(0.,0.,-1.));
#17215=DIRECTION('',(0.,-1.,0.));
#17216=DIRECTION('',(0.608761429008722,0.,-0.793353340291235));
#17217=DIRECTION('',(-0.793353340291235,0.,-0.608761429008722));
#17218=DIRECTION('',(0.,-1.,0.));
#17219=DIRECTION('',(0.382683432365092,0.,0.923879532511286));
#17220=DIRECTION('',(0.923879532511286,0.,-0.382683432365092));
#17221=DIRECTION('',(0.,-1.,0.));
#17222=DIRECTION('',(0.,-1.,0.));
#17223=DIRECTION('',(0.,0.,-1.));
#17224=DIRECTION('',(0.,-1.,0.));
#17225=DIRECTION('',(0.707106781186548,0.,-0.707106781186548));
#17226=DIRECTION('',(-0.707106781186548,0.,-0.707106781186548));
#17227=DIRECTION('',(0.,-1.,0.));
#17228=DIRECTION('',(0.258819045102523,0.,0.965925826289068));
#17229=DIRECTION('',(0.965925826289068,0.,-0.258819045102523));
#17230=DIRECTION('',(0.,-1.,0.));
#17231=DIRECTION('',(0.,-1.,0.));
#17232=DIRECTION('',(0.,0.,-1.));
#17233=DIRECTION('',(0.,-1.,0.));
#17234=DIRECTION('',(0.793353340291235,0.,-0.608761429008721));
#17235=DIRECTION('',(-0.608761429008721,0.,-0.793353340291235));
#17236=DIRECTION('',(0.,-1.,0.));
#17237=DIRECTION('',(0.130526192220053,0.,0.99144486137381));
#17238=DIRECTION('',(0.99144486137381,0.,-0.130526192220053));
#17239=DIRECTION('',(0.,-1.,0.));
#17240=DIRECTION('',(0.,-1.,0.));
#17241=DIRECTION('',(0.,0.,-1.));
#17242=DIRECTION('',(0.,-1.,0.));
#17243=DIRECTION('',(0.866025403784439,0.,-0.5));
#17244=DIRECTION('',(-0.5,0.,-0.866025403784439));
#17245=DIRECTION('',(0.,-1.,0.));
#17246=DIRECTION('',(0.,0.,1.));
#17247=DIRECTION('',(1.,0.,0.));
#17248=DIRECTION('',(0.,-1.,0.));
#17249=DIRECTION('',(0.,-1.,0.));
#17250=DIRECTION('',(0.,0.,-1.));
#17251=DIRECTION('',(0.,-1.,0.));
#17252=DIRECTION('',(0.923879532511287,0.,-0.38268343236509));
#17253=DIRECTION('',(-0.38268343236509,0.,-0.923879532511287));
#17254=DIRECTION('',(0.,-1.,0.));
#17255=DIRECTION('',(-0.130526192220051,0.,0.991444861373811));
#17256=DIRECTION('',(0.991444861373811,0.,0.130526192220051));
#17257=DIRECTION('',(0.,-1.,0.));
#17258=DIRECTION('',(0.,-1.,0.));
#17259=DIRECTION('',(0.,0.,-1.));
#17260=DIRECTION('',(0.,-1.,0.));
#17261=DIRECTION('',(0.965925826289068,0.,-0.258819045102522));
#17262=DIRECTION('',(-0.258819045102522,0.,-0.965925826289068));
#17263=DIRECTION('',(0.,-1.,0.));
#17264=DIRECTION('',(-0.258819045102519,0.,0.965925826289069));
#17265=DIRECTION('',(0.965925826289069,0.,0.258819045102519));
#17266=DIRECTION('',(0.,-1.,0.));
#17267=DIRECTION('',(0.,-1.,0.));
#17268=DIRECTION('',(0.,0.,-1.));
#17269=DIRECTION('',(0.,-1.,0.));
#17270=DIRECTION('',(0.99144486137381,0.,-0.130526192220053));
#17271=DIRECTION('',(-0.130526192220053,0.,-0.99144486137381));
#17272=DIRECTION('',(0.,-1.,0.));
#17273=DIRECTION('',(-0.382683432365088,0.,0.923879532511288));
#17274=DIRECTION('',(0.923879532511288,0.,0.382683432365088));
#17275=DIRECTION('',(0.,-1.,0.));
#17276=DIRECTION('',(0.,-1.,0.));
#17277=DIRECTION('',(0.,0.,-1.));
#17278=DIRECTION('',(0.,-1.,0.));
#17279=DIRECTION('',(1.,0.,0.));
#17280=DIRECTION('',(0.,0.,-1.));
#17281=DIRECTION('',(0.,-1.,0.));
#17282=DIRECTION('',(-0.5,0.,0.86602540378444));
#17283=DIRECTION('',(0.86602540378444,0.,0.5));
#17284=DIRECTION('',(0.,-1.,0.));
#17285=DIRECTION('',(0.,-1.,0.));
#17286=DIRECTION('',(0.,0.,-1.));
#17287=DIRECTION('',(0.,-1.,0.));
#17288=DIRECTION('',(0.991444861373811,0.,0.130526192220051));
#17289=DIRECTION('',(0.130526192220051,0.,-0.991444861373811));
#17290=DIRECTION('',(0.,-1.,0.));
#17291=DIRECTION('',(-0.608761429008719,0.,0.793353340291236));
#17292=DIRECTION('',(0.793353340291236,0.,0.608761429008719));
#17293=DIRECTION('',(0.,-1.,0.));
#17294=DIRECTION('',(0.,-1.,0.));
#17295=DIRECTION('',(0.,0.,-1.));
#17296=DIRECTION('',(0.,-1.,0.));
#17297=DIRECTION('',(0.965925826289069,0.,0.258819045102519));
#17298=DIRECTION('',(0.258819045102519,0.,-0.965925826289069));
#17299=DIRECTION('',(0.,-1.,0.));
#17300=DIRECTION('',(-0.707106781186548,0.,0.707106781186548));
#17301=DIRECTION('',(0.707106781186548,0.,0.707106781186548));
#17302=DIRECTION('',(0.,-1.,0.));
#17303=DIRECTION('',(0.,-1.,0.));
#17304=DIRECTION('',(0.,0.,-1.));
#17305=DIRECTION('',(0.,-1.,0.));
#17306=DIRECTION('',(0.923879532511288,0.,0.382683432365088));
#17307=DIRECTION('',(0.382683432365088,0.,-0.923879532511288));
#17308=DIRECTION('',(0.,-1.,0.));
#17309=DIRECTION('',(-0.793353340291234,0.,0.608761429008723));
#17310=DIRECTION('',(0.608761429008723,0.,0.793353340291234));
#17311=DIRECTION('',(0.,-1.,0.));
#17312=DIRECTION('',(0.,-1.,0.));
#17313=DIRECTION('',(0.,0.,-1.));
#17314=DIRECTION('',(0.,-1.,0.));
#17315=DIRECTION('',(0.86602540378444,0.,0.5));
#17316=DIRECTION('',(0.5,0.,-0.86602540378444));
#17317=DIRECTION('',(0.,-1.,0.));
#17318=DIRECTION('',(-0.866025403784438,0.,0.5));
#17319=DIRECTION('',(0.5,0.,0.866025403784438));
#17320=DIRECTION('',(0.,-1.,0.));
#17321=DIRECTION('',(0.,-1.,0.));
#17322=DIRECTION('',(0.,0.,-1.));
#17323=DIRECTION('',(0.,-1.,0.));
#17324=DIRECTION('',(0.793353340291236,0.,0.608761429008719));
#17325=DIRECTION('',(0.608761429008719,0.,-0.793353340291236));
#17326=DIRECTION('',(0.,-1.,0.));
#17327=DIRECTION('',(-0.923879532511286,0.,0.382683432365092));
#17328=DIRECTION('',(0.382683432365092,0.,0.923879532511286));
#17329=DIRECTION('',(0.,-1.,0.));
#17330=DIRECTION('',(0.,-1.,0.));
#17331=DIRECTION('',(0.,0.,-1.));
#17332=DIRECTION('',(0.,-1.,0.));
#17333=DIRECTION('',(0.707106781186549,0.,0.707106781186546));
#17334=DIRECTION('',(0.707106781186546,0.,-0.707106781186549));
#17335=DIRECTION('',(0.,-1.,0.));
#17336=DIRECTION('',(-0.965925826289068,0.,0.258819045102521));
#17337=DIRECTION('',(0.258819045102521,0.,0.965925826289068));
#17338=DIRECTION('',(0.,-1.,0.));
#17339=DIRECTION('',(0.,-1.,0.));
#17340=DIRECTION('',(0.,0.,-1.));
#17341=DIRECTION('',(0.,-1.,0.));
#17342=DIRECTION('',(0.608761429008721,0.,0.793353340291235));
#17343=DIRECTION('',(0.793353340291235,0.,-0.608761429008721));
#17344=DIRECTION('',(0.,-1.,0.));
#17345=DIRECTION('',(-0.99144486137381,0.,0.130526192220051));
#17346=DIRECTION('',(0.130526192220051,0.,0.99144486137381));
#17347=DIRECTION('',(0.,-1.,0.));
#17348=DIRECTION('',(0.,-1.,0.));
#17349=DIRECTION('',(0.,0.,-1.));
#17350=DIRECTION('',(0.,-1.,0.));
#17351=DIRECTION('',(0.5,0.,0.866025403784438));
#17352=DIRECTION('',(0.866025403784438,0.,-0.5));
#17353=DIRECTION('',(0.,-1.,0.));
#17354=DIRECTION('',(-1.,0.,0.));
#17355=DIRECTION('',(0.,0.,1.));
#17356=DIRECTION('',(0.,-1.,0.));
#17357=DIRECTION('',(0.,-1.,0.));
#17358=DIRECTION('',(0.,0.,-1.));
#17359=DIRECTION('',(0.,-1.,0.));
#17360=DIRECTION('',(0.382683432365092,0.,0.923879532511286));
#17361=DIRECTION('',(0.923879532511286,0.,-0.382683432365092));
#17362=DIRECTION('',(0.,-1.,0.));
#17363=DIRECTION('',(-0.99144486137381,0.,-0.130526192220052));
#17364=DIRECTION('',(-0.130526192220052,0.,0.99144486137381));
#17365=DIRECTION('',(0.,-1.,0.));
#17366=DIRECTION('',(0.,-1.,0.));
#17367=DIRECTION('',(0.,0.,-1.));
#17368=DIRECTION('',(0.,-1.,0.));
#17369=DIRECTION('',(0.258819045102523,0.,0.965925826289068));
#17370=DIRECTION('',(0.965925826289068,0.,-0.258819045102523));
#17371=DIRECTION('',(0.,-1.,0.));
#17372=DIRECTION('',(-0.965925826289068,0.,-0.258819045102521));
#17373=DIRECTION('',(-0.258819045102521,0.,0.965925826289068));
#17374=DIRECTION('',(0.,-1.,0.));
#17375=DIRECTION('',(0.,-1.,0.));
#17376=DIRECTION('',(0.,0.,-1.));
#17377=DIRECTION('',(0.,-1.,0.));
#17378=DIRECTION('',(0.130526192220053,0.,0.99144486137381));
#17379=DIRECTION('',(0.99144486137381,0.,-0.130526192220053));
#17380=DIRECTION('',(0.,-1.,0.));
#17381=DIRECTION('',(-0.923965399010245,0.,-0.382476066482387));
#17382=DIRECTION('',(-0.382476066482387,0.,0.923965399010245));
#17383=DIRECTION('',(0.,-1.,0.));
#17384=DIRECTION('',(0.,0.,1.));
#17385=DIRECTION('',(1.,0.,0.));
#17386=DIRECTION('',(0.,-1.,0.));
#17387=DIRECTION('',(-0.866025403784439,0.,-0.5));
#17388=DIRECTION('',(-0.5,0.,0.866025403784439));
#17389=DIRECTION('',(0.,-1.,0.));
#17390=DIRECTION('',(0.,-1.,0.));
#17391=DIRECTION('',(0.,0.,-1.));
#17392=DIRECTION('',(0.,-1.,0.));
#17393=DIRECTION('',(-0.130526192220051,0.,0.991444861373811));
#17394=DIRECTION('',(0.991444861373811,0.,0.130526192220051));
#17395=DIRECTION('',(0.,-1.,0.));
#17396=DIRECTION('',(-0.793353340291234,0.,-0.608761429008722));
#17397=DIRECTION('',(-0.608761429008722,0.,0.793353340291234));
#17398=DIRECTION('',(0.,-1.,0.));
#17399=DIRECTION('',(0.,-1.,0.));
#17400=DIRECTION('',(0.,0.,-1.));
#17401=DIRECTION('',(0.,-1.,0.));
#17402=DIRECTION('',(-0.258819045102519,0.,0.965925826289069));
#17403=DIRECTION('',(0.965925826289069,0.,0.258819045102519));
#17404=DIRECTION('',(0.,-1.,0.));
#17405=DIRECTION('',(-0.707106781186548,0.,-0.707106781186548));
#17406=DIRECTION('',(-0.707106781186548,0.,0.707106781186548));
#17407=DIRECTION('',(0.,-1.,0.));
#17408=DIRECTION('',(0.,-1.,0.));
#17409=DIRECTION('',(0.,0.,-1.));
#17410=DIRECTION('',(0.,-1.,0.));
#17411=DIRECTION('',(-0.382683432365088,0.,0.923879532511288));
#17412=DIRECTION('',(0.923879532511288,0.,0.382683432365088));
#17413=DIRECTION('',(0.,-1.,0.));
#17414=DIRECTION('',(-0.608761429008721,0.,-0.793353340291235));
#17415=DIRECTION('',(-0.793353340291235,0.,0.608761429008721));
#17416=DIRECTION('',(0.,-1.,0.));
#17417=DIRECTION('',(0.,-1.,0.));
#17418=DIRECTION('',(0.,0.,-1.));
#17419=DIRECTION('',(0.,-1.,0.));
#17420=DIRECTION('',(-0.5,0.,0.86602540378444));
#17421=DIRECTION('',(0.86602540378444,0.,0.5));
#17422=DIRECTION('',(0.,-1.,0.));
#17423=DIRECTION('',(-0.5,0.,-0.866025403784439));
#17424=DIRECTION('',(-0.866025403784439,0.,0.5));
#17425=DIRECTION('',(0.,1.,0.));
#17426=DIRECTION('',(0.,0.,1.));
#17427=DIRECTION('',(0.,1.,0.));
#17428=DIRECTION('',(0.,0.,1.));
#17429=DIRECTION('',(0.,1.,0.));
#17430=DIRECTION('',(0.,0.,1.));
#17431=DIRECTION('',(0.,-1.,0.));
#17432=DIRECTION('',(0.,0.,-1.));
#17433=DIRECTION('',(0.,-1.,0.));
#17434=DIRECTION('',(0.,0.,-1.));
#17435=DIRECTION('',(0.,-1.,0.));
#17436=DIRECTION('',(0.,0.,-1.));
#17437=DIRECTION('',(0.,1.,0.));
#17438=DIRECTION('',(0.,0.,1.));
#17439=DIRECTION('',(0.,-1.,0.));
#17440=DIRECTION('',(0.,0.,-1.));
#17441=DIRECTION('',(0.,1.,0.));
#17442=DIRECTION('',(0.,0.,1.));
#17443=DIRECTION('',(0.,1.,0.));
#17444=DIRECTION('',(0.,0.,1.));
#17445=DIRECTION('',(0.,1.,0.));
#17446=DIRECTION('',(0.,0.,1.));
#17447=DIRECTION('',(0.437393956694974,-0.899269996523133,-8.80267118231464E-31));
#17448=DIRECTION('',(-0.899269996523133,-0.437393956694974,-5.24956088737378E-32));
#17449=DIRECTION('',(0.,0.,-1.));
#17450=DIRECTION('',(-1.,0.,0.));
#17451=DIRECTION('',(0.,0.,-1.));
#17452=DIRECTION('',(-1.,0.,0.));
#17453=DIRECTION('',(0.,0.,-1.));
#17454=DIRECTION('',(-1.,0.,0.));
#17455=DIRECTION('',(0.,0.,-1.));
#17456=DIRECTION('',(-1.,0.,0.));
#17457=DIRECTION('',(0.,0.,-1.));
#17458=DIRECTION('',(-1.,0.,0.));
#17459=DIRECTION('',(0.,0.,-1.));
#17460=DIRECTION('',(-1.,0.,0.));
#17461=DIRECTION('',(0.,0.,-1.));
#17462=DIRECTION('',(-1.,0.,0.));
#17463=DIRECTION('',(0.,0.,-1.));
#17464=DIRECTION('',(-1.,0.,0.));
#17465=DIRECTION('',(-1.13070633445762E-16,-1.69503277670118E-16,1.));
#17466=DIRECTION('',(-0.384099299390922,0.923291789310077,1.13070633445761E-16));
#17467=DIRECTION('',(0.,0.,1.));
#17468=DIRECTION('',(1.,0.,0.));
#17469=DIRECTION('',(0.,0.,1.));
#17470=DIRECTION('',(1.,0.,0.));
#17471=DIRECTION('',(0.,0.,1.));
#17472=DIRECTION('',(1.,0.,0.));
#17473=DIRECTION('',(0.,0.,1.));
#17474=DIRECTION('',(1.,0.,0.));
#17475=DIRECTION('',(0.,0.,1.));
#17476=DIRECTION('',(1.,0.,0.));
#17477=DIRECTION('',(0.,0.,1.));
#17478=DIRECTION('',(1.,0.,0.));
#17479=DIRECTION('',(0.,0.,-1.));
#17480=DIRECTION('',(-1.,0.,0.));
#17481=DIRECTION('',(0.,0.,-1.));
#17482=DIRECTION('',(-1.,0.,0.));
#17483=DIRECTION('',(0.,0.,1.));
#17484=DIRECTION('',(1.,0.,0.));
#17485=DIRECTION('',(1.,0.,0.));
#17486=DIRECTION('',(0.,0.,-1.));
#17487=DIRECTION('',(0.,0.,1.));
#17488=DIRECTION('',(1.,0.,0.));
#17489=DIRECTION('',(0.,0.,-1.));
#17490=DIRECTION('',(1.,0.,0.));
#17491=DIRECTION('',(0.,0.,-1.));
#17492=DIRECTION('',(1.,0.,0.));
#17493=DIRECTION('',(0.,0.,-1.));
#17494=DIRECTION('',(1.,0.,0.));
#17495=DIRECTION('',(0.,0.,1.));
#17496=DIRECTION('',(1.,0.,0.));
#17497=DIRECTION('',(0.,0.,-1.));
#17498=DIRECTION('',(-1.,0.,0.));
#17499=DIRECTION('',(0.,0.,-1.));
#17500=DIRECTION('',(1.,0.,0.));
#17501=DIRECTION('',(0.,0.,-1.));
#17502=DIRECTION('',(0.,0.,-1.));
#17503=DIRECTION('',(0.,0.,-1.));
#17504=DIRECTION('',(-1.,0.,0.));
#17505=DIRECTION('',(0.,0.,-1.));
#17506=DIRECTION('',(1.,0.,0.));
#17507=DIRECTION('',(0.,0.,-1.));
#17508=DIRECTION('',(0.,0.,-1.));
#17509=DIRECTION('',(0.,0.,1.));
#17510=DIRECTION('',(1.,0.,0.));
#17511=DIRECTION('',(0.,0.,-1.));
#17512=DIRECTION('',(-1.,0.,0.));
#17513=DIRECTION('',(0.,0.,1.));
#17514=DIRECTION('',(-1.,0.,0.));
#17515=DIRECTION('',(0.,0.,-1.));
#17516=DIRECTION('',(-1.,0.,0.));
#17517=DIRECTION('',(0.,0.,-1.));
#17518=DIRECTION('',(-1.,0.,0.));
#17519=DIRECTION('',(0.,0.,-1.));
#17520=DIRECTION('',(-1.,0.,0.));
#17521=DIRECTION('',(0.,0.,-1.));
#17522=DIRECTION('',(-1.,0.,0.));
#17523=DIRECTION('',(0.,0.,-1.));
#17524=DIRECTION('',(0.,0.,-1.));
#17525=DIRECTION('',(0.,0.,-1.));
#17526=DIRECTION('',(-1.,0.,0.));
#17527=DIRECTION('',(0.,0.,1.));
#17528=DIRECTION('',(-1.,0.,0.));
#17529=DIRECTION('',(0.,0.,-1.));
#17530=DIRECTION('',(0.,0.,-1.));
#17531=DIRECTION('',(0.,0.,-1.));
#17532=DIRECTION('',(-1.,0.,0.));
#17533=DIRECTION('',(0.,0.,-1.));
#17534=DIRECTION('',(-1.,0.,0.));
#17535=DIRECTION('',(0.,0.,-1.));
#17536=DIRECTION('',(-1.,0.,0.));
#17537=DIRECTION('',(0.,0.,-1.));
#17538=DIRECTION('',(-1.,0.,0.));
#17539=DIRECTION('',(0.,0.,-1.));
#17540=DIRECTION('',(-1.,0.,0.));
#17541=DIRECTION('',(0.,0.,-1.));
#17542=DIRECTION('',(1.,0.,0.));
#17543=DIRECTION('',(0.,0.,1.));
#17544=DIRECTION('',(1.,0.,0.));
#17545=DIRECTION('',(0.,0.,-1.));
#17546=DIRECTION('',(-1.,0.,0.));
#17547=DIRECTION('',(0.,0.,-1.));
#17548=DIRECTION('',(-1.,0.,0.));
#17549=DIRECTION('',(0.,0.,-1.));
#17550=DIRECTION('',(-1.,0.,0.));
#17551=DIRECTION('',(0.,0.,-1.));
#17552=DIRECTION('',(-1.,0.,0.));
#17553=DIRECTION('',(0.,0.,-1.));
#17554=DIRECTION('',(-1.,0.,0.));
#17555=DIRECTION('',(0.,0.,1.));
#17556=DIRECTION('',(1.,0.,0.));
#17557=DIRECTION('',(0.,0.,-1.));
#17558=DIRECTION('',(-1.,0.,0.));
#17559=DIRECTION('',(0.,0.,-1.));
#17560=DIRECTION('',(-1.,0.,0.));
#17561=DIRECTION('',(0.,0.,-1.));
#17562=DIRECTION('',(-1.,0.,0.));
#17563=DIRECTION('',(0.,0.,-1.));
#17564=DIRECTION('',(-1.,0.,0.));
#17565=DIRECTION('',(1.07158798064712E-18,1.57189229981047E-17,1.));
#17566=DIRECTION('',(0.990748195963547,-0.135712977253382,1.0715879806471E-18));
#17567=DIRECTION('',(0.,-1.,0.));
#17568=DIRECTION('',(1.,0.,0.));
#17569=DIRECTION('',(0.,0.,-1.));
#17570=DIRECTION('',(0.697641315020716,-0.716447203620872,0.));
#17571=DIRECTION('',(0.,1.,0.));
#17572=DIRECTION('',(-1.,0.,0.));
#17573=DIRECTION('',(0.,0.,1.));
#17574=DIRECTION('',(-1.,-7.27196081129478E-15,0.));
#17575=DIRECTION('',(0.,0.,1.));
#17576=DIRECTION('',(-1.,-7.27196081129478E-15,0.));
#17577=DIRECTION('',(0.,0.,1.));
#17578=DIRECTION('',(1.,0.,0.));
#17579=DIRECTION('',(0.,0.,1.));
#17580=DIRECTION('',(-0.5,0.866025403784436,0.));
#17581=DIRECTION('',(0.,0.,1.));
#17582=DIRECTION('',(0.,0.,1.));
#17583=DIRECTION('',(1.,0.,0.));
#17584=DIRECTION('',(0.,-1.,0.));
#17585=DIRECTION('',(1.,0.,0.));
#17586=DIRECTION('',(1.,7.66053886991358E-15,0.));
#17587=DIRECTION('',(0.,0.,1.));
#17588=DIRECTION('',(1.,7.66053886991358E-15,0.));
#17589=DIRECTION('',(-0.866025403784433,-0.50000000000001,0.));
#17590=DIRECTION('',(0.50000000000001,-0.866025403784433,0.));
#17591=DIRECTION('',(0.,0.,1.));
#17592=DIRECTION('',(0.50000000000001,-0.866025403784433,0.));
#17593=DIRECTION('',(0.,0.,1.));
#17594=DIRECTION('',(0.50000000000001,-0.866025403784433,0.));
#17595=DIRECTION('',(0.866025403784433,0.500000000000011,0.));
#17596=DIRECTION('',(-0.500000000000011,0.866025403784433,0.));
#17597=DIRECTION('',(0.,0.,1.));
#17598=DIRECTION('',(-0.500000000000011,0.866025403784433,0.));
#17599=DIRECTION('',(0.,0.,1.));
#17600=DIRECTION('',(-0.500000000000011,0.866025403784433,0.));
#17601=DIRECTION('',(0.,0.,1.));
#17602=DIRECTION('',(1.,0.,0.));
#17603=DIRECTION('',(0.,0.,1.));
#17604=DIRECTION('',(-0.499999999999993,-0.866025403784443,0.));
#17605=DIRECTION('',(0.,0.,1.));
#17606=DIRECTION('',(1.,0.,0.));
#17607=DIRECTION('',(0.86602540378444,-0.5,0.));
#17608=DIRECTION('',(0.5,0.86602540378444,0.));
#17609=DIRECTION('',(0.,0.,1.));
#17610=DIRECTION('',(0.5,0.86602540378444,0.));
#17611=DIRECTION('',(0.,0.,1.));
#17612=DIRECTION('',(0.5,0.86602540378444,0.));
#17613=DIRECTION('',(-0.86602540378444,0.5,0.));
#17614=DIRECTION('',(-0.5,-0.86602540378444,0.));
#17615=DIRECTION('',(0.,0.,1.));
#17616=DIRECTION('',(-0.5,-0.86602540378444,0.));
#17617=DIRECTION('',(0.,0.,1.));
#17618=DIRECTION('',(-0.5,-0.86602540378444,0.));
#17619=DIRECTION('',(0.,0.,1.));
#17620=DIRECTION('',(1.,0.,0.));
#17621=DIRECTION('',(0.,0.,1.));
#17622=DIRECTION('',(1.,0.,0.));
#17623=DIRECTION('',(0.,0.,1.));
#17624=DIRECTION('',(1.,0.,0.));
#17625=DIRECTION('',(0.,0.,-1.));
#17626=DIRECTION('',(-1.,0.,0.));
#17627=DIRECTION('',(0.,0.,1.));
#17628=DIRECTION('',(1.,0.,0.));
#17629=DIRECTION('',(0.,0.,1.));
#17630=DIRECTION('',(1.,0.,0.));
#17631=DIRECTION('',(0.,0.,-1.));
#17632=DIRECTION('',(-1.,0.,0.));
#17633=DIRECTION('',(0.,0.,1.));
#17634=DIRECTION('',(1.,0.,0.));
#17635=DIRECTION('',(0.,0.,1.));
#17636=DIRECTION('',(1.,0.,0.));
#17637=DIRECTION('',(0.,0.,-1.));
#17638=DIRECTION('',(-1.,0.,0.));
#17639=DIRECTION('',(0.,0.,1.));
#17640=DIRECTION('',(1.,0.,0.));
#17641=DIRECTION('',(0.,0.,1.));
#17642=DIRECTION('',(1.,0.,0.));
#17643=DIRECTION('',(0.,0.,1.));
#17644=DIRECTION('',(1.,0.,0.));
#17645=DIRECTION('',(0.,0.,1.));
#17646=DIRECTION('',(1.,0.,0.));
#17647=DIRECTION('',(0.,0.,1.));
#17648=DIRECTION('',(1.,0.,0.));
#17649=DIRECTION('',(0.,0.,1.));
#17650=DIRECTION('',(1.,0.,0.));
#17651=DIRECTION('',(0.,0.,1.));
#17652=DIRECTION('',(1.,0.,0.));
#17653=DIRECTION('',(0.,0.,1.));
#17654=DIRECTION('',(-0.499999999999993,-0.866025403784443,0.));
#17655=DIRECTION('',(0.,0.,1.));
#17656=DIRECTION('',(-0.5,0.866025403784436,0.));
#17657=DIRECTION('',(0.,0.,-1.));
#17658=DIRECTION('',(1.,0.,0.));
#17659=DIRECTION('',(0.,0.,1.));
#17660=DIRECTION('',(1.,0.,0.));
#17661=DIRECTION('',(0.,0.,1.));
#17662=DIRECTION('',(1.,0.,0.));
#17663=DIRECTION('',(0.,0.,1.));
#17664=DIRECTION('',(1.,0.,0.));
#17665=DIRECTION('',(0.,0.,1.));
#17666=DIRECTION('',(1.,0.,0.));
#17667=DIRECTION('',(0.,0.,1.));
#17668=DIRECTION('',(1.,0.,0.));
#17669=DIRECTION('',(0.,0.,1.));
#17670=DIRECTION('',(1.,0.,0.));
#17671=DIRECTION('',(0.,0.,1.));
#17672=DIRECTION('',(1.,0.,0.));
#17673=DIRECTION('',(0.,0.,1.));
#17674=DIRECTION('',(1.,0.,0.));
#17675=DIRECTION('',(0.,0.,-1.));
#17676=DIRECTION('',(1.,0.,0.));
#17677=DIRECTION('',(0.,0.,1.));
#17678=DIRECTION('',(1.,0.,0.));
#17679=DIRECTION('',(0.,0.,1.));
#17680=DIRECTION('',(1.,0.,0.));
#17681=DIRECTION('',(0.,0.,-1.));
#17682=DIRECTION('',(1.,0.,0.));
#17683=DIRECTION('',(0.,0.,1.));
#17684=DIRECTION('',(1.,0.,0.));
#17685=DIRECTION('',(0.,0.,1.));
#17686=DIRECTION('',(1.,0.,0.));
#17687=DIRECTION('',(0.,0.,1.));
#17688=DIRECTION('',(1.,0.,0.));
#17689=DIRECTION('',(0.,0.,-1.));
#17690=DIRECTION('',(1.,0.,0.));
#17691=DIRECTION('',(0.,0.,1.));
#17692=DIRECTION('',(1.,0.,0.));
#17693=DIRECTION('',(0.,0.,1.));
#17694=DIRECTION('',(1.,0.,0.));
#17695=DIRECTION('',(0.,0.,1.));
#17696=DIRECTION('',(1.,0.,0.));
#17697=DIRECTION('',(0.,0.,1.));
#17698=DIRECTION('',(1.,0.,0.));
#17699=DIRECTION('',(0.,0.,1.));
#17700=DIRECTION('',(1.,0.,0.));
#17701=DIRECTION('',(0.,0.,1.));
#17702=DIRECTION('',(1.,0.,0.));
#17703=DIRECTION('',(0.,0.,1.));
#17704=DIRECTION('',(1.,0.,0.));
#17705=DIRECTION('',(0.,0.,1.));
#17706=DIRECTION('',(1.,0.,0.));
#17707=DIRECTION('',(0.,0.,1.));
#17708=DIRECTION('',(1.,0.,0.));
#17709=DIRECTION('',(0.,0.,1.));
#17710=DIRECTION('',(1.,0.,0.));
#17711=DIRECTION('',(0.,0.,1.));
#17712=DIRECTION('',(1.,0.,0.));
#17713=DIRECTION('',(0.,0.,1.));
#17714=DIRECTION('',(1.,0.,0.));
#17715=DIRECTION('',(0.,0.,1.));
#17716=DIRECTION('',(1.,0.,0.));
#17717=DIRECTION('',(0.,0.,1.));
#17718=DIRECTION('',(1.,0.,0.));
#17719=DIRECTION('',(0.,-1.,0.));
#17720=DIRECTION('',(-1.,0.,0.));
#17721=DIRECTION('',(3.32320936955295E-16,1.15768974892334E-16,1.));
#17722=DIRECTION('',(0.523310781999508,0.8521419045224,-2.72558724142245E-16));
#17723=DIRECTION('',(1.,0.,0.));
#17724=DIRECTION('',(0.,0.,-1.));
#17725=DIRECTION('',(1.08360590852881E-26,-2.80884663399331E-26,1.));
#17726=DIRECTION('',(-0.825729003788358,0.564067028200272,2.47914260085562E-26));
#17727=DIRECTION('',(0.,0.,1.));
#17728=DIRECTION('',(1.,0.,0.));
#17729=DIRECTION('',(0.,0.,-1.));
#17730=DIRECTION('',(-0.499999999999991,-0.866025403784444,0.));
#17731=DIRECTION('',(0.500000000000011,-0.866025403784433,0.));
#17732=DIRECTION('',(0.,0.,-1.));
#17733=DIRECTION('',(-0.499999999999993,-0.866025403784443,0.));
#17734=DIRECTION('',(-0.50000000000001,0.866025403784433,0.));
#17735=DIRECTION('',(-0.866025403784433,-0.50000000000001,0.));
#17736=DIRECTION('',(0.50000000000001,-0.866025403784433,0.));
#17737=DIRECTION('',(0.,0.,1.));
#17738=DIRECTION('',(0.50000000000001,-0.866025403784433,0.));
#17739=DIRECTION('',(0.,0.,1.));
#17740=DIRECTION('',(0.866025403784433,0.500000000000011,0.));
#17741=DIRECTION('',(-0.500000000000011,0.866025403784433,0.));
#17742=DIRECTION('',(0.,0.,1.));
#17743=DIRECTION('',(-0.500000000000011,0.866025403784433,0.));
#17744=DIRECTION('',(0.,0.,1.));
#17745=DIRECTION('',(0.,0.,1.));
#17746=DIRECTION('',(-0.499999999999993,-0.866025403784443,0.));
#17747=DIRECTION('',(0.,0.,1.));
#17748=DIRECTION('',(-0.499999999999993,-0.866025403784443,0.));
#17749=DIRECTION('',(0.,0.,1.));
#17750=DIRECTION('',(1.,0.,0.));
#17751=DIRECTION('',(0.,0.,-1.));
#17752=DIRECTION('',(-0.5,0.866025403784436,0.));
#17753=DIRECTION('',(-1.,-7.66053886991358E-15,0.));
#17754=DIRECTION('',(0.,0.,-1.));
#17755=DIRECTION('',(-0.5,0.866025403784437,0.));
#17756=DIRECTION('',(1.,7.27196081129478E-15,0.));
#17757=DIRECTION('',(0.,1.,0.));
#17758=DIRECTION('',(-1.,0.,0.));
#17759=DIRECTION('',(0.,0.,1.));
#17760=DIRECTION('',(-1.,-7.27196081129478E-15,0.));
#17761=DIRECTION('',(0.,0.,1.));
#17762=DIRECTION('',(0.,-1.,0.));
#17763=DIRECTION('',(1.,0.,0.));
#17764=DIRECTION('',(0.,0.,1.));
#17765=DIRECTION('',(1.,7.66053886991358E-15,0.));
#17766=DIRECTION('',(0.,0.,1.));
#17767=DIRECTION('',(0.,0.,1.));
#17768=DIRECTION('',(-0.5,0.866025403784436,0.));
#17769=DIRECTION('',(0.,0.,1.));
#17770=DIRECTION('',(-0.5,0.866025403784436,0.));
#17771=DIRECTION('',(0.,0.,1.));
#17772=DIRECTION('',(1.,0.,0.));
#17773=DIRECTION('',(0.,0.,-1.));
#17774=DIRECTION('',(1.,3.46944695195361E-15,0.));
#17775=DIRECTION('',(0.5,0.86602540378444,0.));
#17776=DIRECTION('',(0.,0.,-1.));
#17777=DIRECTION('',(1.,0.,0.));
#17778=DIRECTION('',(-0.5,-0.86602540378444,0.));
#17779=DIRECTION('',(0.86602540378444,-0.5,0.));
#17780=DIRECTION('',(0.5,0.86602540378444,0.));
#17781=DIRECTION('',(0.,0.,1.));
#17782=DIRECTION('',(0.5,0.86602540378444,0.));
#17783=DIRECTION('',(0.,0.,1.));
#17784=DIRECTION('',(-0.86602540378444,0.5,0.));
#17785=DIRECTION('',(-0.5,-0.86602540378444,0.));
#17786=DIRECTION('',(0.,0.,1.));
#17787=DIRECTION('',(-0.5,-0.86602540378444,0.));
#17788=DIRECTION('',(0.,0.,1.));
#17789=DIRECTION('',(0.,0.,1.));
#17790=DIRECTION('',(1.,0.,0.));
#17791=DIRECTION('',(0.,0.,1.));
#17792=DIRECTION('',(1.,0.,0.));
#17793=DIRECTION('',(0.,0.,1.));
#17794=DIRECTION('',(1.,0.,0.));
#17795=DIRECTION('',(0.,0.,1.));
#17796=DIRECTION('',(1.,0.,0.));
#17797=DIRECTION('',(0.,0.,1.));
#17798=DIRECTION('',(1.,0.,0.));
#17799=DIRECTION('',(0.,0.,1.));
#17800=DIRECTION('',(1.,0.,0.));
#17801=DIRECTION('',(0.,0.,1.));
#17802=DIRECTION('',(-0.5,0.866025403784436,0.));
#17803=DIRECTION('',(0.,0.,1.));
#17804=DIRECTION('',(-0.499999999999993,-0.866025403784443,0.));
#17805=DIRECTION('',(0.,0.,1.));
#17806=DIRECTION('',(1.,0.,0.));
#17807=DIRECTION('',(0.,0.,1.));
#17808=DIRECTION('',(1.,0.,0.));
#17809=DIRECTION('',(0.,0.,1.));
#17810=DIRECTION('',(1.,0.,0.));
#17811=DIRECTION('',(0.,0.,-1.));
#17812=DIRECTION('',(-1.,0.,0.));
#17813=DIRECTION('',(0.,0.,-1.));
#17814=DIRECTION('',(-1.,0.,0.));
#17815=DIRECTION('',(0.,0.,1.));
#17816=DIRECTION('',(1.,0.,0.));
#17817=DIRECTION('',(0.,0.,1.));
#17818=DIRECTION('',(-0.5,0.866025403784436,0.));
#17819=DIRECTION('',(0.,0.,1.));
#17820=DIRECTION('',(-0.499999999999993,-0.866025403784443,0.));
#17821=DIRECTION('',(0.,0.,1.));
#17822=DIRECTION('',(1.,0.,0.));
#17823=DIRECTION('',(-0.573576436351044,0.819152044288994,0.));
#17824=DIRECTION('',(-0.819152044288994,-0.573576436351044,0.));
#17825=DIRECTION('',(-0.819152044288993,-0.573576436351045,0.));
#17826=DIRECTION('',(0.,0.,1.));
#17827=DIRECTION('',(0.819152044288993,0.573576436351045,0.));
#17828=DIRECTION('',(0.,0.,1.));
#17829=DIRECTION('',(0.573576436351045,0.819152044288993,0.));
#17830=DIRECTION('',(-0.819152044288993,0.573576436351045,0.));
#17831=DIRECTION('',(-0.819152044288994,0.573576436351044,0.));
#17832=DIRECTION('',(0.,0.,1.));
#17833=DIRECTION('',(0.819152044288994,-0.573576436351044,0.));
#17834=DIRECTION('',(0.,0.,1.));
#17835=DIRECTION('',(-0.573576436351044,0.819152044288994,0.));
#17836=DIRECTION('',(-0.819152044288994,-0.573576436351044,0.));
#17837=DIRECTION('',(0.819152044288994,0.573576436351044,0.));
#17838=DIRECTION('',(0.,0.,1.));
#17839=DIRECTION('',(-0.819152044288994,-0.573576436351044,0.));
#17840=DIRECTION('',(0.,0.,1.));
#17841=DIRECTION('',(0.573576436351045,0.819152044288993,0.));
#17842=DIRECTION('',(-0.819152044288993,0.573576436351045,0.));
#17843=DIRECTION('',(0.819152044288993,-0.573576436351045,0.));
#17844=DIRECTION('',(0.,0.,1.));
#17845=DIRECTION('',(-0.819152044288993,0.573576436351045,0.));
#17846=DIRECTION('',(0.,0.,1.));
#17847=DIRECTION('',(0.,0.,1.));
#17848=DIRECTION('',(1.,0.,0.));
#17849=DIRECTION('',(0.,0.,-1.));
#17850=DIRECTION('',(1.,0.,0.));
#17851=DIRECTION('',(0.,0.,-1.));
#17852=DIRECTION('',(1.,0.,0.));
#17853=DIRECTION('',(0.,0.,-1.));
#17854=DIRECTION('',(1.,0.,0.));
#17855=DIRECTION('',(0.,0.,1.));
#17856=DIRECTION('',(1.,0.,0.));
#17857=DIRECTION('',(0.,0.,-1.));
#17858=DIRECTION('',(-1.,0.,0.));
#17859=DIRECTION('',(0.,0.,-1.));
#17860=DIRECTION('',(1.,0.,0.));
#17861=DIRECTION('',(0.,0.,-1.));
#17862=DIRECTION('',(0.,0.,-1.));
#17863=DIRECTION('',(0.,0.,-1.));
#17864=DIRECTION('',(-1.,0.,0.));
#17865=DIRECTION('',(0.,0.,-1.));
#17866=DIRECTION('',(1.,0.,0.));
#17867=DIRECTION('',(0.,0.,-1.));
#17868=DIRECTION('',(0.,0.,-1.));
#17869=DIRECTION('',(0.,0.,1.));
#17870=DIRECTION('',(1.,0.,0.));
#17871=DIRECTION('',(0.,0.,-1.));
#17872=DIRECTION('',(-1.,0.,0.));
#17873=DIRECTION('',(0.,0.,1.));
#17874=DIRECTION('',(-1.,0.,0.));
#17875=DIRECTION('',(0.,0.,-1.));
#17876=DIRECTION('',(-1.,0.,0.));
#17877=DIRECTION('',(0.,0.,-1.));
#17878=DIRECTION('',(-1.,0.,0.));
#17879=DIRECTION('',(0.,0.,-1.));
#17880=DIRECTION('',(-1.,0.,0.));
#17881=DIRECTION('',(0.,0.,-1.));
#17882=DIRECTION('',(-1.,0.,0.));
#17883=DIRECTION('',(0.,0.,-1.));
#17884=DIRECTION('',(0.,0.,-1.));
#17885=DIRECTION('',(0.,0.,-1.));
#17886=DIRECTION('',(-1.,0.,0.));
#17887=DIRECTION('',(0.,0.,1.));
#17888=DIRECTION('',(-1.,0.,0.));
#17889=DIRECTION('',(0.,0.,-1.));
#17890=DIRECTION('',(0.,0.,-1.));
#17891=DIRECTION('',(0.,0.,-1.));
#17892=DIRECTION('',(-1.,0.,0.));
#17893=DIRECTION('',(0.,0.,1.));
#17894=DIRECTION('',(-1.,0.,0.));
#17895=DIRECTION('',(0.,0.,-1.));
#17896=DIRECTION('',(-1.,0.,0.));
#17897=DIRECTION('',(0.,0.,1.));
#17898=DIRECTION('',(-1.,0.,0.));
#17899=DIRECTION('',(0.,0.,-1.));
#17900=DIRECTION('',(-1.,0.,0.));
#17901=DIRECTION('',(0.,0.,-1.));
#17902=DIRECTION('',(-1.,0.,0.));
#17903=DIRECTION('',(0.,0.,-1.));
#17904=DIRECTION('',(-1.,0.,0.));
#17905=DIRECTION('',(0.,0.,-1.));
#17906=DIRECTION('',(-1.,0.,0.));
#17907=DIRECTION('',(0.,0.,-1.));
#17908=DIRECTION('',(-1.,0.,0.));
#17909=DIRECTION('',(0.,0.,-1.));
#17910=DIRECTION('',(-1.,0.,0.));
#17911=DIRECTION('',(0.,0.,-1.));
#17912=DIRECTION('',(-1.,0.,0.));
#17913=DIRECTION('',(0.,0.,-1.));
#17914=DIRECTION('',(-1.,0.,0.));
#17915=DIRECTION('',(0.,0.,1.));
#17916=DIRECTION('',(1.,0.,0.));
#17917=DIRECTION('',(0.,0.,-1.));
#17918=DIRECTION('',(-1.,0.,0.));
#17919=DIRECTION('',(0.,0.,-1.));
#17920=DIRECTION('',(-1.,0.,0.));
#17921=DIRECTION('',(0.,0.,-1.));
#17922=DIRECTION('',(-1.,0.,0.));
#17923=DIRECTION('',(0.,0.,-1.));
#17924=DIRECTION('',(1.,0.,0.));
#17925=DIRECTION('',(0.,0.,1.));
#17926=DIRECTION('',(1.,0.,0.));
#17927=DIRECTION('',(0.,0.,-1.));
#17928=DIRECTION('',(-1.,0.,0.));
#17929=DIRECTION('',(0.,0.,1.));
#17930=DIRECTION('',(1.,0.,0.));
#17931=DIRECTION('',(0.,0.,-1.));
#17932=DIRECTION('',(-1.,0.,0.));
#17933=DIRECTION('',(0.,0.,-1.));
#17934=DIRECTION('',(-1.,0.,0.));
#17935=DIRECTION('',(0.,0.,-1.));
#17936=DIRECTION('',(-1.,0.,0.));
#17937=DIRECTION('',(0.,0.,-1.));
#17938=DIRECTION('',(-1.,0.,0.));
#17939=DIRECTION('',(0.,0.,1.));
#17940=DIRECTION('',(0.990748195963547,-0.135712977253381,0.));
#17941=DIRECTION('',(0.,0.,1.));
#17942=DIRECTION('',(1.,0.,0.));
#17943=DIRECTION('',(0.,0.,1.));
#17944=DIRECTION('',(1.,0.,0.));
#17945=DIRECTION('',(0.,0.,1.));
#17946=DIRECTION('',(1.,0.,0.));
#17947=DIRECTION('',(0.,0.,-1.));
#17948=DIRECTION('',(-1.,0.,0.));
#17949=DIRECTION('',(0.,0.,1.));
#17950=DIRECTION('',(-1.,0.,0.));
#17951=DIRECTION('',(0.,0.,-1.));
#17952=DIRECTION('',(0.,0.,-1.));
#17953=DIRECTION('',(-1.,0.,0.));
#17954=DIRECTION('',(0.,0.,1.));
#17955=DIRECTION('',(0.,0.,-1.));
#17956=DIRECTION('',(-1.04744440165294E-14,1.,0.));
#17957=DIRECTION('',(0.,0.,-1.));
#17958=DIRECTION('',(-1.,0.,0.));
#17959=DIRECTION('',(0.,0.,-1.));
#17960=DIRECTION('',(-1.,0.,0.));
#17961=DIRECTION('',(0.,-1.,0.));
#17962=DIRECTION('',(0.,0.,-1.));
#17963=DIRECTION('',(-1.,0.,0.));
#17964=DIRECTION('',(-0.998092281178314,0.061739762327613,0.));
#17965=DIRECTION('',(0.,0.,-1.));
#17966=DIRECTION('',(-1.,0.,0.));
#17967=DIRECTION('',(0.,0.,-1.));
#17968=DIRECTION('',(-1.,0.,0.));
#17969=DIRECTION('',(-0.998092281178314,-0.0617397623276126,0.));
#17970=DIRECTION('',(0.,0.,-1.));
#17971=DIRECTION('',(-1.,0.,0.));
#17972=DIRECTION('',(0.,0.,1.));
#17973=DIRECTION('',(-1.,0.,0.));
#17974=DIRECTION('',(0.,0.,-1.));
#17975=DIRECTION('',(0.,0.,1.));
#17976=DIRECTION('',(0.,0.,-1.));
#17977=DIRECTION('',(-1.04744440165294E-14,1.,0.));
#17978=DIRECTION('',(0.,0.,-1.));
#17979=DIRECTION('',(-1.,0.,0.));
#17980=DIRECTION('',(0.,0.,-1.));
#17981=DIRECTION('',(-1.,0.,0.));
#17982=DIRECTION('',(-0.998092281178314,-0.0617397623276126,0.));
#17983=DIRECTION('',(0.,0.,-1.));
#17984=DIRECTION('',(-1.,0.,0.));
#17985=DIRECTION('',(-0.998092281178314,0.061739762327613,0.));
#17986=DIRECTION('',(0.,0.,-1.));
#17987=DIRECTION('',(-1.,0.,0.));
#17988=DIRECTION('',(0.,-1.,0.));
#17989=DIRECTION('',(0.,0.,-1.));
#17990=DIRECTION('',(-1.04744440165294E-14,1.,0.));
#17991=DIRECTION('',(0.,0.,-1.));
#17992=DIRECTION('',(3.49148133884314E-15,-1.,0.));
#17993=DIRECTION('',(0.,0.,-1.));
#17994=DIRECTION('',(3.46944695195361E-15,-1.,0.));
#17995=DIRECTION('',(1.,3.49148133884314E-15,0.));
#17996=DIRECTION('',(0.,0.,-1.));
#17997=DIRECTION('',(3.46944695195361E-15,-1.,0.));
#17998=DIRECTION('',(-0.0617397623276095,-0.998092281178314,0.));
#17999=DIRECTION('',(0.,0.,-1.));
#18000=DIRECTION('',(-1.,0.,0.));
#18001=DIRECTION('',(0.,0.,-1.));
#18002=DIRECTION('',(3.49148133884314E-15,-1.,0.));
#18003=DIRECTION('',(0.,0.,-1.));
#18004=DIRECTION('',(-1.,0.,0.));
#18005=DIRECTION('',(0.0617397623276161,-0.998092281178314,0.));
#18006=DIRECTION('',(0.,0.,-1.));
#18007=DIRECTION('',(-1.,0.,0.));
#18008=DIRECTION('',(0.,0.,1.));
#18009=DIRECTION('',(-1.,-1.38777878078145E-15,0.));
#18010=DIRECTION('',(0.,0.,-1.));
#18011=DIRECTION('',(0.,0.,1.));
#18012=DIRECTION('',(0.,0.,-1.));
#18013=DIRECTION('',(-1.04744440165294E-14,1.,0.));
#18014=DIRECTION('',(0.,0.,-1.));
#18015=DIRECTION('',(3.49148133884314E-15,-1.,0.));
#18016=DIRECTION('',(0.,0.,-1.));
#18017=DIRECTION('',(3.46944695195361E-15,-1.,0.));
#18018=DIRECTION('',(0.0617397623276161,-0.998092281178314,0.));
#18019=DIRECTION('',(0.,0.,1.));
#18020=DIRECTION('',(-1.,0.,0.));
#18021=DIRECTION('',(0.,0.,-1.));
#18022=DIRECTION('',(3.49148133884314E-15,-1.,0.));
#18023=DIRECTION('',(-0.0617397623276095,-0.998092281178314,0.));
#18024=DIRECTION('',(0.,0.,-1.));
#18025=DIRECTION('',(3.46944695195361E-15,-1.,0.));
#18026=DIRECTION('',(1.,3.49148133884314E-15,0.));
#18027=DIRECTION('',(0.,0.,-1.));
#18028=DIRECTION('',(-1.,0.,0.));
#18029=DIRECTION('',(0.,0.,-1.));
#18030=DIRECTION('',(0.,0.,1.));
#18031=DIRECTION('',(0.,0.,-1.));
#18032=DIRECTION('',(-1.04744440165294E-14,1.,0.));
#18033=DIRECTION('',(0.,0.,-1.));
#18034=DIRECTION('',(1.,0.,0.));
#18035=DIRECTION('',(0.,0.,-1.));
#18036=DIRECTION('',(1.,0.,0.));
#18037=DIRECTION('',(0.,1.,0.));
#18038=DIRECTION('',(0.,0.,-1.));
#18039=DIRECTION('',(1.,0.,0.));
#18040=DIRECTION('',(0.998092281178314,-0.061739762327613,0.));
#18041=DIRECTION('',(0.,0.,-1.));
#18042=DIRECTION('',(-1.,0.,0.));
#18043=DIRECTION('',(0.,0.,-1.));
#18044=DIRECTION('',(1.,0.,0.));
#18045=DIRECTION('',(0.,0.,-1.));
#18046=DIRECTION('',(-1.,0.,0.));
#18047=DIRECTION('',(0.998092281178314,0.0617397623276126,0.));
#18048=DIRECTION('',(0.,0.,-1.));
#18049=DIRECTION('',(-1.04744440165294E-14,1.,0.));
#18050=DIRECTION('',(0.,0.,-1.));
#18051=DIRECTION('',(1.,0.,0.));
#18052=DIRECTION('',(0.,0.,-1.));
#18053=DIRECTION('',(1.,0.,0.));
#18054=DIRECTION('',(0.998092281178314,0.0617397623276126,0.));
#18055=DIRECTION('',(0.,0.,1.));
#18056=DIRECTION('',(-1.,0.,0.));
#18057=DIRECTION('',(0.,0.,-1.));
#18058=DIRECTION('',(1.,0.,0.));
#18059=DIRECTION('',(0.,0.,1.));
#18060=DIRECTION('',(-1.,-5.20417042793043E-15,0.));
#18061=DIRECTION('',(0.998092281178314,-0.061739762327613,0.));
#18062=DIRECTION('',(0.,0.,-1.));
#18063=DIRECTION('',(1.,0.,0.));
#18064=DIRECTION('',(0.,1.,0.));
#18065=DIRECTION('',(0.,0.,-1.));
#18066=DIRECTION('',(-1.04744440165294E-14,1.,0.));
#18067=DIRECTION('',(0.,0.,-1.));
#18068=DIRECTION('',(-1.04744440165294E-14,1.,0.));
#18069=DIRECTION('',(0.,0.,-1.));
#18070=DIRECTION('',(-1.04083408558608E-14,1.,0.));
#18071=DIRECTION('',(-1.,-1.04744440165294E-14,0.));
#18072=DIRECTION('',(0.,0.,-1.));
#18073=DIRECTION('',(-1.04083408558608E-14,1.,0.));
#18074=DIRECTION('',(0.0617397623276026,0.998092281178314,0.));
#18075=DIRECTION('',(0.,0.,-1.));
#18076=DIRECTION('',(-1.,0.,0.));
#18077=DIRECTION('',(0.,0.,-1.));
#18078=DIRECTION('',(-1.04744440165294E-14,1.,0.));
#18079=DIRECTION('',(0.,0.,-1.));
#18080=DIRECTION('',(-1.,0.,0.));
#18081=DIRECTION('',(-0.061739762327623,0.998092281178313,0.));
#18082=DIRECTION('',(0.,0.,-1.));
#18083=DIRECTION('',(-1.,0.,0.));
#18084=DIRECTION('',(0.,0.,1.));
#18085=DIRECTION('',(-1.,1.38777878078145E-15,0.));
#18086=DIRECTION('',(0.,0.,-1.));
#18087=DIRECTION('',(0.,0.,1.));
#18088=DIRECTION('',(0.,0.,-1.));
#18089=DIRECTION('',(-1.04744440165294E-14,1.,0.));
#18090=DIRECTION('',(0.,0.,-1.));
#18091=DIRECTION('',(-1.04744440165294E-14,1.,0.));
#18092=DIRECTION('',(0.,0.,-1.));
#18093=DIRECTION('',(-1.04083408558608E-14,1.,0.));
#18094=DIRECTION('',(-0.061739762327623,0.998092281178313,0.));
#18095=DIRECTION('',(0.,0.,1.));
#18096=DIRECTION('',(-1.,0.,0.));
#18097=DIRECTION('',(0.,0.,-1.));
#18098=DIRECTION('',(-1.04744440165294E-14,1.,0.));
#18099=DIRECTION('',(0.0617397623276026,0.998092281178314,0.));
#18100=DIRECTION('',(0.,0.,-1.));
#18101=DIRECTION('',(-1.04083408558608E-14,1.,0.));
#18102=DIRECTION('',(-1.,-1.04744440165294E-14,0.));
#18103=DIRECTION('',(0.,0.,-1.));
#18104=DIRECTION('',(-1.,0.,0.));
#18105=DIRECTION('',(0.,0.,-1.));
#18106=DIRECTION('',(0.,0.,1.));
#18107=DIRECTION('',(-0.0617397623276126,0.998092281178314,0.));
#18108=DIRECTION('',(-0.998092281178314,-0.0617397623276126,0.));
#18109=DIRECTION('',(0.,0.,1.));
#18110=DIRECTION('',(0.,0.,1.));
#18111=DIRECTION('',(1.,0.,0.));
#18112=DIRECTION('',(0.,0.,1.));
#18113=DIRECTION('',(-1.,0.,0.));
#18114=DIRECTION('',(0.,0.,1.));
#18115=DIRECTION('',(0.,0.,1.));
#18116=DIRECTION('',(0.,0.,1.));
#18117=DIRECTION('',(1.,0.,0.));
#18118=DIRECTION('',(0.,0.,1.));
#18119=DIRECTION('',(0.061739762327613,0.998092281178314,0.));
#18120=DIRECTION('',(-0.998092281178314,0.061739762327613,0.));
#18121=DIRECTION('',(0.,0.,1.));
#18122=DIRECTION('',(-3.46944695195361E-15,1.,0.));
#18123=DIRECTION('',(0.,0.,1.));
#18124=DIRECTION('',(0.,0.,1.));
#18125=DIRECTION('',(0.,-1.,0.));
#18126=DIRECTION('',(0.,0.,1.));
#18127=DIRECTION('',(0.,0.,1.));
#18128=DIRECTION('',(0.,0.,1.));
#18129=DIRECTION('',(-3.46944695195361E-15,1.,0.));
#18130=DIRECTION('',(0.,0.,1.));
#18131=DIRECTION('',(-0.998092281178314,0.0617397623276096,0.));
#18132=DIRECTION('',(-0.0617397623276096,-0.998092281178314,0.));
#18133=DIRECTION('',(-0.998092281178314,-0.0617397623276161,0.));
#18134=DIRECTION('',(0.0617397623276161,-0.998092281178314,0.));
#18135=DIRECTION('',(0.,0.,1.));
#18136=DIRECTION('',(-1.,0.,0.));
#18137=DIRECTION('',(0.,0.,1.));
#18138=DIRECTION('',(0.,0.,1.));
#18139=DIRECTION('',(1.,0.,0.));
#18140=DIRECTION('',(0.,0.,1.));
#18141=DIRECTION('',(0.,0.,1.));
#18142=DIRECTION('',(0.,0.,1.));
#18143=DIRECTION('',(-1.,0.,0.));
#18144=DIRECTION('',(0.,0.,1.));
#18145=DIRECTION('',(-0.061739762327613,-0.998092281178314,0.));
#18146=DIRECTION('',(0.998092281178314,-0.061739762327613,0.));
#18147=DIRECTION('',(0.,0.,1.));
#18148=DIRECTION('',(0.0617397623276126,-0.998092281178314,0.));
#18149=DIRECTION('',(0.998092281178314,0.0617397623276126,0.));
#18150=DIRECTION('',(0.,0.,-1.));
#18151=DIRECTION('',(0.,0.,1.));
#18152=DIRECTION('',(1.04083408558608E-14,-1.,0.));
#18153=DIRECTION('',(0.,0.,1.));
#18154=DIRECTION('',(0.,0.,1.));
#18155=DIRECTION('',(0.,1.,0.));
#18156=DIRECTION('',(0.,0.,1.));
#18157=DIRECTION('',(0.,0.,1.));
#18158=DIRECTION('',(0.,0.,1.));
#18159=DIRECTION('',(1.04083408558608E-14,-1.,0.));
#18160=DIRECTION('',(0.,0.,1.));
#18161=DIRECTION('',(0.998092281178314,-0.0617397623276026,0.));
#18162=DIRECTION('',(0.0617397623276026,0.998092281178314,0.));
#18163=DIRECTION('',(0.998092281178313,0.061739762327623,0.));
#18164=DIRECTION('',(-0.061739762327623,0.998092281178313,0.));
#18165=DIRECTION('',(0.,0.,-1.));
#18166=DIRECTION('',(-1.,0.,0.));
#18167=DIRECTION('',(0.,0.,-1.));
#18168=DIRECTION('',(-1.,0.,0.));
#18169=DIRECTION('',(-0.866025403784441,0.,0.5));
#18170=DIRECTION('',(0.866025403784441,0.,-0.5));
#18171=DIRECTION('',(0.866025403784439,0.,0.5));
#18172=DIRECTION('',(-0.866025403784439,0.,-0.5));
#18173=DIRECTION('',(0.,0.,1.));
#18174=DIRECTION('',(1.,0.,0.));
#18175=DIRECTION('',(0.,0.,1.));
#18176=DIRECTION('',(0.,0.,-1.));
#18177=DIRECTION('',(0.,1.,0.));
#18178=DIRECTION('',(0.,0.,1.));
#18179=DIRECTION('',(0.,0.,1.));
#18180=DIRECTION('',(0.,1.,0.));
#18181=DIRECTION('',(0.,0.,1.));
#18182=DIRECTION('',(0.,0.,-1.));
#18183=DIRECTION('',(0.,0.,-1.));
#18184=DIRECTION('',(-1.,0.,0.));
#18185=DIRECTION('',(0.,0.,-1.));
#18186=DIRECTION('',(-1.,0.,0.));
#18187=DIRECTION('',(0.,0.,-1.));
#18188=DIRECTION('',(-1.,0.,0.));
#18189=DIRECTION('',(-0.0179359317491036,0.0175778306283821,-0.999684611376354));
#18190=DIRECTION('',(-0.999839088515442,0.,0.0179387033146474));
#18191=DIRECTION('',(0.0205587778800031,-0.295683717505608,0.955064644856119));
#18192=DIRECTION('',(0.595793945716029,-0.763497654096111,-0.249200534585825));
#18193=DIRECTION('',(-0.0175759874682992,0.0179054946361856,-0.99968518941032));
#18194=DIRECTION('',(0.,0.999839634236857,0.0179082609180536));
#18195=DIRECTION('',(0.920446420278218,-0.390077155728526,-0.0248636275663566));
#18196=DIRECTION('',(0.390197784505042,0.92073106223661,0.));
#18197=DIRECTION('',(0.706883616772413,-0.706883616772409,-0.0251217968606994));
#18198=DIRECTION('',(0.707106781186546,0.707106781186549,0.));
#18199=DIRECTION('',(0.706883616772413,-0.706883616772409,-0.0251217968606994));
#18200=DIRECTION('',(0.707106781186546,0.707106781186549,0.));
#18201=DIRECTION('',(0.706883616772383,-0.706883616772439,-0.0251217968606994));
#18202=DIRECTION('',(0.707106157141816,0.707107404359837,-3.50945448125777E-5));
#18203=DIRECTION('',(0.706883616772383,-0.70688361677244,-0.0251217968606994));
#18204=DIRECTION('',(0.707106157141816,0.707107404359837,-3.50945448118755E-5));
#18205=DIRECTION('',(0.,0.,1.));
#18206=DIRECTION('',(1.,0.,0.));
#18207=DIRECTION('',(0.,0.,-1.));
#18208=DIRECTION('',(-1.,0.,0.));
#18209=DIRECTION('',(0.,0.,1.));
#18210=DIRECTION('',(1.,0.,0.));
#18211=DIRECTION('',(0.,0.,1.));
#18212=DIRECTION('',(1.,0.,0.));
#18213=DIRECTION('',(0.,0.,-1.));
#18214=DIRECTION('',(1.,0.,0.));
#18215=DIRECTION('',(0.,0.,-1.));
#18216=DIRECTION('',(-1.,0.,0.));
#18217=DIRECTION('',(0.,0.,-1.));
#18218=DIRECTION('',(-1.,0.,0.));
#18219=DIRECTION('',(0.,0.,-1.));
#18220=DIRECTION('',(-1.,0.,0.));
#18221=DIRECTION('',(0.,0.,1.));
#18222=DIRECTION('',(-1.,0.,0.));
#18223=DIRECTION('',(0.,0.,1.));
#18224=DIRECTION('',(1.,0.,0.));
#18225=DIRECTION('',(0.,0.,1.));
#18226=DIRECTION('',(1.,0.,0.));
#18227=DIRECTION('',(0.,0.,-1.));
#18228=DIRECTION('',(1.,0.,0.));
#18229=DIRECTION('',(0.,0.,-1.));
#18230=DIRECTION('',(1.,0.,0.));
#18231=DIRECTION('',(0.,0.,1.));
#18232=DIRECTION('',(1.,0.,0.));
#18233=DIRECTION('',(0.,0.,1.));
#18234=DIRECTION('',(1.,0.,0.));
#18235=DIRECTION('',(0.,0.,-1.));
#18236=DIRECTION('',(-1.,0.,0.));
#18237=DIRECTION('',(0.,0.,-1.));
#18238=DIRECTION('',(-1.,0.,0.));
#18239=DIRECTION('',(0.,0.,1.));
#18240=DIRECTION('',(1.,0.,0.));
#18241=DIRECTION('',(0.,0.,-1.));
#18242=DIRECTION('',(1.,0.,0.));
#18243=DIRECTION('',(0.,0.,-1.));
#18244=DIRECTION('',(-1.,0.,0.));
#18245=DIRECTION('',(0.,0.,-1.));
#18246=DIRECTION('',(-1.,0.,0.));
#18247=DIRECTION('',(0.,0.,1.));
#18248=DIRECTION('',(1.,0.,0.));
#18249=DIRECTION('',(0.,0.,-1.));
#18250=DIRECTION('',(-1.,0.,0.));
#18251=DIRECTION('',(0.,0.,-1.));
#18252=DIRECTION('',(-1.,0.,0.));
#18253=DIRECTION('',(0.,0.,1.));
#18254=DIRECTION('',(-1.,0.,0.));
#18255=DIRECTION('',(0.,0.,-1.));
#18256=DIRECTION('',(-1.,0.,0.));
#18257=DIRECTION('',(0.,0.,-1.));
#18258=DIRECTION('',(-1.,0.,0.));
#18259=DIRECTION('',(0.,0.,1.));
#18260=DIRECTION('',(-1.,0.,0.));
#18261=DIRECTION('',(0.,0.,-1.));
#18262=DIRECTION('',(-1.,0.,0.));
#18263=DIRECTION('',(0.,0.,1.));
#18264=DIRECTION('',(1.,0.,0.));
#18265=DIRECTION('',(0.,0.,1.));
#18266=DIRECTION('',(1.,0.,0.));
#18267=DIRECTION('',(0.,0.,-1.));
#18268=DIRECTION('',(-1.,0.,0.));
#18269=DIRECTION('',(0.,0.,-1.));
#18270=DIRECTION('',(1.,0.,0.));
#18271=DIRECTION('',(0.,0.,1.));
#18272=DIRECTION('',(1.,0.,0.));
#18273=DIRECTION('',(0.,0.,1.));
#18274=DIRECTION('',(1.,0.,0.));
#18275=DIRECTION('',(0.,0.,1.));
#18276=DIRECTION('',(-1.,0.,0.));
#18277=DIRECTION('',(0.,0.,-1.));
#18278=DIRECTION('',(-1.,0.,0.));
#18279=DIRECTION('',(0.,0.,-1.));
#18280=DIRECTION('',(-1.,0.,0.));
#18281=DIRECTION('',(0.,0.,-1.));
#18282=DIRECTION('',(-1.,0.,0.));
#18283=DIRECTION('',(0.,0.,-1.));
#18284=DIRECTION('',(-1.,0.,0.));
#18285=DIRECTION('',(0.,0.,-1.));
#18286=DIRECTION('',(-1.,0.,0.));
#18287=DIRECTION('',(0.,0.,-1.));
#18288=DIRECTION('',(-1.,0.,0.));
#18289=DIRECTION('',(0.,0.,1.));
#18290=DIRECTION('',(1.04744440165294E-14,-1.,0.));
#18291=DIRECTION('',(0.,0.,1.));
#18292=DIRECTION('',(-1.,0.,0.));
#18293=DIRECTION('',(0.,0.,1.));
#18294=DIRECTION('',(-3.49148133884314E-15,1.,0.));
#18295=DIRECTION('',(0.,0.,1.));
#18296=DIRECTION('',(1.,0.,0.));
#18297=DIRECTION('',(0.,0.,-1.));
#18298=DIRECTION('',(-1.,0.,0.));
#18299=DIRECTION('',(0.,0.,-1.));
#18300=DIRECTION('',(-1.,0.,0.));
#18301=DIRECTION('',(0.,0.,1.));
#18302=DIRECTION('',(0.,0.,-1.));
#18303=DIRECTION('',(-1.,0.,0.));
#18304=DIRECTION('',(0.,0.,-1.));
#18305=DIRECTION('',(0.,0.,-1.));
#18306=DIRECTION('',(-1.,0.,0.));
#18307=DIRECTION('',(0.,0.,1.));
#18308=DIRECTION('',(1.,0.,0.));
#18309=DIRECTION('',(-3.03383416892296E-26,5.89829700275599E-27,1.));
#18310=DIRECTION('',(0.901360877752809,0.433068779822195,2.47914260085562E-26));
#18311=DIRECTION('',(0.,0.,1.));
#18312=DIRECTION('',(-0.5,0.866025403784436,0.));
#18313=DIRECTION('',(0.,0.,-1.));
#18314=DIRECTION('',(-0.499999999999993,-0.866025403784443,0.));
#18315=DIRECTION('',(-1.,-7.105427357601E-15,0.));
#18316=DIRECTION('',(0.,0.,-1.));
#18317=DIRECTION('',(-0.499999999999993,-0.866025403784443,0.));
#18318=DIRECTION('',(1.,6.55031584528842E-15,0.));
#18319=DIRECTION('',(0.,1.,0.));
#18320=DIRECTION('',(-1.,0.,0.));
#18321=DIRECTION('',(-1.,-6.55031584528842E-15,0.));
#18322=DIRECTION('',(0.,0.,1.));
#18323=DIRECTION('',(0.,0.,1.));
#18324=DIRECTION('',(0.,-1.,0.));
#18325=DIRECTION('',(1.,0.,0.));
#18326=DIRECTION('',(1.,7.105427357601E-15,0.));
#18327=DIRECTION('',(0.,0.,1.));
#18328=DIRECTION('',(0.,0.,1.));
#18329=DIRECTION('',(0.,0.,1.));
#18330=DIRECTION('',(-0.499999999999993,-0.866025403784443,0.));
#18331=DIRECTION('',(0.,0.,1.));
#18332=DIRECTION('',(-0.499999999999993,-0.866025403784443,0.));
#18333=DIRECTION('',(0.,0.,1.));
#18334=DIRECTION('',(-0.5,0.866025403784436,0.));
#18335=DIRECTION('',(0.,0.,-1.));
#18336=DIRECTION('',(-0.5,0.866025403784439,0.));
#18337=DIRECTION('',(0.5,0.86602540378444,0.));
#18338=DIRECTION('',(0.,0.,-1.));
#18339=DIRECTION('',(-0.5,0.866025403784436,0.));
#18340=DIRECTION('',(-0.5,-0.86602540378444,0.));
#18341=DIRECTION('',(0.86602540378444,-0.5,0.));
#18342=DIRECTION('',(0.5,0.86602540378444,0.));
#18343=DIRECTION('',(0.5,0.86602540378444,0.));
#18344=DIRECTION('',(0.,0.,1.));
#18345=DIRECTION('',(0.,0.,1.));
#18346=DIRECTION('',(-0.86602540378444,0.5,0.));
#18347=DIRECTION('',(-0.5,-0.86602540378444,0.));
#18348=DIRECTION('',(-0.5,-0.86602540378444,0.));
#18349=DIRECTION('',(0.,0.,1.));
#18350=DIRECTION('',(0.,0.,1.));
#18351=DIRECTION('',(0.,0.,1.));
#18352=DIRECTION('',(-0.5,0.866025403784436,0.));
#18353=DIRECTION('',(0.,0.,1.));
#18354=DIRECTION('',(-0.5,0.866025403784436,0.));
#18355=DIRECTION('',(0.,0.,1.));
#18356=DIRECTION('',(-0.5,0.866025403784436,0.));
#18357=DIRECTION('',(0.,0.,-1.));
#18358=DIRECTION('',(1.,0.,0.));
#18359=DIRECTION('',(0.5,-0.86602540378444,0.));
#18360=DIRECTION('',(0.,0.,-1.));
#18361=DIRECTION('',(1.,0.,0.));
#18362=DIRECTION('',(-0.5,0.86602540378444,0.));
#18363=DIRECTION('',(-0.86602540378444,-0.5,0.));
#18364=DIRECTION('',(0.5,-0.86602540378444,0.));
#18365=DIRECTION('',(0.5,-0.86602540378444,0.));
#18366=DIRECTION('',(0.,0.,1.));
#18367=DIRECTION('',(0.,0.,1.));
#18368=DIRECTION('',(0.86602540378444,0.5,0.));
#18369=DIRECTION('',(-0.5,0.86602540378444,0.));
#18370=DIRECTION('',(-0.5,0.86602540378444,0.));
#18371=DIRECTION('',(0.,0.,1.));
#18372=DIRECTION('',(0.,0.,1.));
#18373=DIRECTION('',(0.,0.,1.));
#18374=DIRECTION('',(1.,0.,0.));
#18375=DIRECTION('',(0.,0.,1.));
#18376=DIRECTION('',(1.,0.,0.));
#18377=DIRECTION('',(0.,0.,1.));
#18378=DIRECTION('',(1.,0.,0.));
#18379=DIRECTION('',(0.,0.,-1.));
#18380=DIRECTION('',(1.,0.,0.));
#18381=DIRECTION('',(0.,0.,1.));
#18382=DIRECTION('',(1.,0.,0.));
#18383=DIRECTION('',(0.,0.,-1.));
#18384=DIRECTION('',(1.,0.,0.));
#18385=DIRECTION('',(0.,0.,-1.));
#18386=DIRECTION('',(1.,0.,0.));
#18387=DIRECTION('',(0.,0.,-1.));
#18388=DIRECTION('',(1.,0.,0.));
#18389=DIRECTION('',(0.,0.,1.));
#18390=DIRECTION('',(1.,0.,0.));
#18391=DIRECTION('',(0.,0.,1.));
#18392=DIRECTION('',(-0.5,0.866025403784436,0.));
#18393=DIRECTION('',(0.,0.,1.));
#18394=DIRECTION('',(-0.499999999999993,-0.866025403784443,0.));
#18395=DIRECTION('',(0.,0.,1.));
#18396=DIRECTION('',(1.,0.,0.));
#18397=DIRECTION('',(0.,0.,1.));
#18398=DIRECTION('',(1.,0.,0.));
#18399=DIRECTION('',(0.,0.,-1.));
#18400=DIRECTION('',(1.,0.,0.));
#18401=DIRECTION('',(0.,0.,1.));
#18402=DIRECTION('',(1.,0.,0.));
#18403=DIRECTION('',(0.,0.,-1.));
#18404=DIRECTION('',(1.,0.,0.));
#18405=DIRECTION('',(0.,0.,-1.));
#18406=DIRECTION('',(1.,0.,0.));
#18407=DIRECTION('',(0.,0.,-1.));
#18408=DIRECTION('',(1.,0.,0.));
#18409=DIRECTION('',(0.,0.,1.));
#18410=DIRECTION('',(1.,0.,0.));
#18411=DIRECTION('',(0.,0.,-1.));
#18412=DIRECTION('',(-1.,0.,0.));
#18413=DIRECTION('',(0.,0.,-1.));
#18414=DIRECTION('',(-1.,0.,0.));
#18415=DIRECTION('',(0.,0.,-1.));
#18416=DIRECTION('',(-1.,0.,0.));
#18417=DIRECTION('',(0.,0.,-1.));
#18418=DIRECTION('',(-1.,0.,0.));
#18419=DIRECTION('',(0.,0.,-1.));
#18420=DIRECTION('',(-1.,0.,0.));
#18421=DIRECTION('',(0.,0.,1.));
#18422=DIRECTION('',(1.,0.,0.));
#18423=DIRECTION('',(0.,0.,1.));
#18424=DIRECTION('',(-0.5,0.866025403784436,0.));
#18425=DIRECTION('',(0.,0.,1.));
#18426=DIRECTION('',(-0.499999999999993,-0.866025403784443,0.));
#18427=DIRECTION('',(0.,0.,1.));
#18428=DIRECTION('',(1.,0.,0.));
#18429=DIRECTION('',(0.,0.,1.));
#18430=DIRECTION('',(1.,0.,0.));
#18431=DIRECTION('',(0.86602540378444,-0.5,0.));
#18432=DIRECTION('',(-0.544728586009151,0.500000000000186,0.673253865628921));
#18433=DIRECTION('',(-0.86602540378444,-0.5,0.));
#18434=DIRECTION('',(0.544718486834211,0.499999449874283,-0.673262445281527));
#18435=DIRECTION('',(0.,-1.,0.));
#18436=DIRECTION('',(1.74897406310451E-5,0.99999999974693,1.41509078327272E-5));
#18437=DIRECTION('',(0.777406601108932,0.,0.628998391533919));
#18438=DIRECTION('',(0.628998391533919,0.,-0.777406601108932));
#18439=DIRECTION('',(0.,-1.,0.));
#18440=DIRECTION('',(0.,0.,1.));
#18441=DIRECTION('',(1.,0.,0.));
#18442=DIRECTION('',(0.,1.,0.));
#18443=DIRECTION('',(0.841253532831189,0.,0.540640817455586));
#18444=DIRECTION('',(0.540640817455586,0.,-0.841253532831189));
#18445=DIRECTION('',(0.,1.,0.));
#18446=DIRECTION('',(0.540640817455586,0.,-0.841253532831189));
#18447=DIRECTION('',(0.,1.,0.));
#18448=DIRECTION('',(-0.540640817455586,0.,0.841253532831189));
#18449=DIRECTION('',(0.540640817455586,0.,-0.841253532831189));
#18450=DIRECTION('',(-0.841253532831189,0.,-0.540640817455586));
#18451=DIRECTION('',(0.841253532831189,0.,0.540640817455586));
#18452=DIRECTION('',(-0.841253532831189,0.,-0.540640817455586));
#18453=DIRECTION('',(0.,1.,0.));
#18454=DIRECTION('',(-0.841253532831189,0.,-0.540640817455586));
#18455=DIRECTION('',(-0.540640817455586,0.,0.841253532831189));
#18456=DIRECTION('',(0.,-1.,0.));
#18457=DIRECTION('',(0.540640817455586,0.,-0.841253532831189));
#18458=DIRECTION('',(-0.540640817455586,0.,0.841253532831189));
#18459=DIRECTION('',(0.415415013001897,0.,0.909631995354513));
#18460=DIRECTION('',(0.909631995354513,0.,-0.415415013001897));
#18461=DIRECTION('',(0.,1.,0.));
#18462=DIRECTION('',(0.909631995354513,0.,-0.415415013001897));
#18463=DIRECTION('',(0.,1.,0.));
#18464=DIRECTION('',(-0.909631995354513,0.,0.415415013001897));
#18465=DIRECTION('',(0.909631995354513,0.,-0.415415013001897));
#18466=DIRECTION('',(-0.415415013001897,0.,-0.909631995354513));
#18467=DIRECTION('',(0.415415013001897,0.,0.909631995354513));
#18468=DIRECTION('',(-0.415415013001897,0.,-0.909631995354513));
#18469=DIRECTION('',(0.,1.,0.));
#18470=DIRECTION('',(-0.415415013001897,0.,-0.909631995354513));
#18471=DIRECTION('',(-0.909631995354513,0.,0.415415013001897));
#18472=DIRECTION('',(0.,-1.,0.));
#18473=DIRECTION('',(0.909631995354513,0.,-0.415415013001897));
#18474=DIRECTION('',(-0.909631995354513,0.,0.415415013001897));
#18475=DIRECTION('',(-0.142314838273275,0.,0.989821441880934));
#18476=DIRECTION('',(0.989821441880934,0.,0.142314838273275));
#18477=DIRECTION('',(0.,1.,0.));
#18478=DIRECTION('',(0.989821441880934,0.,0.142314838273275));
#18479=DIRECTION('',(0.,1.,0.));
#18480=DIRECTION('',(-0.989821441880934,0.,-0.142314838273275));
#18481=DIRECTION('',(0.989821441880934,0.,0.142314838273275));
#18482=DIRECTION('',(0.142314838273275,0.,-0.989821441880934));
#18483=DIRECTION('',(-0.142314838273275,0.,0.989821441880934));
#18484=DIRECTION('',(0.142314838273275,0.,-0.989821441880934));
#18485=DIRECTION('',(0.,1.,0.));
#18486=DIRECTION('',(0.142314838273275,0.,-0.989821441880934));
#18487=DIRECTION('',(-0.989821441880934,0.,-0.142314838273275));
#18488=DIRECTION('',(0.,-1.,0.));
#18489=DIRECTION('',(0.989821441880934,0.,0.142314838273275));
#18490=DIRECTION('',(-0.989821441880934,0.,-0.142314838273275));
#18491=DIRECTION('',(-0.654860733945278,0.,0.755749574354264));
#18492=DIRECTION('',(0.755749574354264,0.,0.654860733945278));
#18493=DIRECTION('',(0.,1.,0.));
#18494=DIRECTION('',(0.755749574354264,0.,0.654860733945278));
#18495=DIRECTION('',(0.,1.,0.));
#18496=DIRECTION('',(-0.755749574354264,0.,-0.654860733945278));
#18497=DIRECTION('',(0.755749574354264,0.,0.654860733945278));
#18498=DIRECTION('',(0.654860733945278,0.,-0.755749574354264));
#18499=DIRECTION('',(-0.654860733945278,0.,0.755749574354264));
#18500=DIRECTION('',(0.654860733945278,0.,-0.755749574354264));
#18501=DIRECTION('',(0.,1.,0.));
#18502=DIRECTION('',(0.654860733945278,0.,-0.755749574354264));
#18503=DIRECTION('',(-0.755749574354264,0.,-0.654860733945278));
#18504=DIRECTION('',(0.,-1.,0.));
#18505=DIRECTION('',(0.755749574354264,0.,0.654860733945278));
#18506=DIRECTION('',(-0.755749574354264,0.,-0.654860733945278));
#18507=DIRECTION('',(-0.959492973614495,0.,0.281732556841437));
#18508=DIRECTION('',(0.281732556841437,0.,0.959492973614495));
#18509=DIRECTION('',(0.,1.,0.));
#18510=DIRECTION('',(0.281732556841437,0.,0.959492973614495));
#18511=DIRECTION('',(0.,1.,0.));
#18512=DIRECTION('',(-0.281732556841437,0.,-0.959492973614495));
#18513=DIRECTION('',(0.281732556841437,0.,0.959492973614495));
#18514=DIRECTION('',(0.959492973614495,0.,-0.281732556841437));
#18515=DIRECTION('',(-0.959492973614495,0.,0.281732556841437));
#18516=DIRECTION('',(0.959492973614495,0.,-0.281732556841437));
#18517=DIRECTION('',(0.,1.,0.));
#18518=DIRECTION('',(0.959492973614495,0.,-0.281732556841437));
#18519=DIRECTION('',(-0.281732556841437,0.,-0.959492973614495));
#18520=DIRECTION('',(0.,-1.,0.));
#18521=DIRECTION('',(0.281732556841437,0.,0.959492973614495));
#18522=DIRECTION('',(-0.281732556841437,0.,-0.959492973614495));
#18523=DIRECTION('',(-0.959492973614499,0.,-0.281732556841423));
#18524=DIRECTION('',(-0.281732556841423,0.,0.959492973614499));
#18525=DIRECTION('',(0.,1.,0.));
#18526=DIRECTION('',(-0.281732556841423,0.,0.959492973614499));
#18527=DIRECTION('',(0.,1.,0.));
#18528=DIRECTION('',(0.281732556841423,0.,-0.959492973614499));
#18529=DIRECTION('',(-0.281732556841424,0.,0.959492973614499));
#18530=DIRECTION('',(0.959492973614499,0.,0.281732556841424));
#18531=DIRECTION('',(-0.959492973614499,0.,-0.281732556841424));
#18532=DIRECTION('',(0.959492973614499,0.,0.281732556841424));
#18533=DIRECTION('',(0.,1.,0.));
#18534=DIRECTION('',(0.959492973614499,0.,0.281732556841423));
#18535=DIRECTION('',(0.281732556841423,0.,-0.959492973614499));
#18536=DIRECTION('',(0.,-1.,0.));
#18537=DIRECTION('',(-0.281732556841423,0.,0.959492973614499));
#18538=DIRECTION('',(0.281732556841423,0.,-0.959492973614499));
#18539=DIRECTION('',(-0.654860733945289,0.,-0.755749574354255));
#18540=DIRECTION('',(-0.755749574354255,0.,0.654860733945289));
#18541=DIRECTION('',(0.,1.,0.));
#18542=DIRECTION('',(-0.755749574354255,0.,0.654860733945289));
#18543=DIRECTION('',(0.,1.,0.));
#18544=DIRECTION('',(0.755749574354255,0.,-0.654860733945289));
#18545=DIRECTION('',(-0.755749574354255,0.,0.654860733945289));
#18546=DIRECTION('',(0.654860733945289,0.,0.755749574354255));
#18547=DIRECTION('',(-0.654860733945289,0.,-0.755749574354255));
#18548=DIRECTION('',(0.654860733945289,0.,0.755749574354255));
#18549=DIRECTION('',(0.,1.,0.));
#18550=DIRECTION('',(0.654860733945289,0.,0.755749574354255));
#18551=DIRECTION('',(0.755749574354255,0.,-0.654860733945289));
#18552=DIRECTION('',(0.,-1.,0.));
#18553=DIRECTION('',(-0.755749574354255,0.,0.654860733945289));
#18554=DIRECTION('',(0.755749574354255,0.,-0.654860733945289));
#18555=DIRECTION('',(-0.142314838273289,0.,-0.989821441880932));
#18556=DIRECTION('',(-0.989821441880932,0.,0.142314838273289));
#18557=DIRECTION('',(0.,1.,0.));
#18558=DIRECTION('',(-0.989821441880932,0.,0.142314838273289));
#18559=DIRECTION('',(0.,1.,0.));
#18560=DIRECTION('',(0.989821441880932,0.,-0.142314838273289));
#18561=DIRECTION('',(-0.989821441880932,0.,0.142314838273289));
#18562=DIRECTION('',(0.142314838273289,0.,0.989821441880932));
#18563=DIRECTION('',(-0.142314838273289,0.,-0.989821441880932));
#18564=DIRECTION('',(0.142314838273289,0.,0.989821441880932));
#18565=DIRECTION('',(0.,1.,0.));
#18566=DIRECTION('',(0.142314838273289,0.,0.989821441880932));
#18567=DIRECTION('',(0.989821441880932,0.,-0.142314838273289));
#18568=DIRECTION('',(0.,-1.,0.));
#18569=DIRECTION('',(-0.989821441880932,0.,0.142314838273289));
#18570=DIRECTION('',(0.989821441880932,0.,-0.142314838273289));
#18571=DIRECTION('',(0.415415013001884,0.,-0.90963199535452));
#18572=DIRECTION('',(-0.90963199535452,0.,-0.415415013001884));
#18573=DIRECTION('',(0.,1.,0.));
#18574=DIRECTION('',(-0.909631995354519,0.,-0.415415013001884));
#18575=DIRECTION('',(0.,1.,0.));
#18576=DIRECTION('',(0.909631995354519,0.,0.415415013001884));
#18577=DIRECTION('',(-0.909631995354519,0.,-0.415415013001884));
#18578=DIRECTION('',(-0.415415013001884,0.,0.909631995354519));
#18579=DIRECTION('',(0.415415013001884,0.,-0.909631995354519));
#18580=DIRECTION('',(-0.415415013001884,0.,0.909631995354519));
#18581=DIRECTION('',(0.,1.,0.));
#18582=DIRECTION('',(-0.415415013001884,0.,0.90963199535452));
#18583=DIRECTION('',(0.90963199535452,0.,0.415415013001884));
#18584=DIRECTION('',(0.,-1.,0.));
#18585=DIRECTION('',(-0.90963199535452,0.,-0.415415013001884));
#18586=DIRECTION('',(0.90963199535452,0.,0.415415013001884));
#18587=DIRECTION('',(0.84125353283118,0.,-0.540640817455599));
#18588=DIRECTION('',(-0.540640817455599,0.,-0.84125353283118));
#18589=DIRECTION('',(0.,1.,0.));
#18590=DIRECTION('',(-0.540640817455599,0.,-0.84125353283118));
#18591=DIRECTION('',(0.,1.,0.));
#18592=DIRECTION('',(0.540640817455599,0.,0.84125353283118));
#18593=DIRECTION('',(-0.540640817455599,0.,-0.841253532831181));
#18594=DIRECTION('',(-0.841253532831181,0.,0.540640817455599));
#18595=DIRECTION('',(0.84125353283118,0.,-0.540640817455599));
#18596=DIRECTION('',(-0.84125353283118,0.,0.540640817455599));
#18597=DIRECTION('',(0.,1.,0.));
#18598=DIRECTION('',(-0.84125353283118,0.,0.540640817455599));
#18599=DIRECTION('',(0.540640817455599,0.,0.84125353283118));
#18600=DIRECTION('',(0.,-1.,0.));
#18601=DIRECTION('',(-0.540640817455599,0.,-0.84125353283118));
#18602=DIRECTION('',(0.540640817455599,0.,0.84125353283118));
#18603=DIRECTION('',(1.,0.,0.));
#18604=DIRECTION('',(0.,0.,-1.));
#18605=DIRECTION('',(0.,1.,0.));
#18606=DIRECTION('',(-1.14373924909521E-16,0.,-1.));
#18607=DIRECTION('',(0.,1.,0.));
#18608=DIRECTION('',(1.14373924909521E-16,0.,1.));
#18609=DIRECTION('',(0.,0.,-1.));
#18610=DIRECTION('',(-1.,0.,0.));
#18611=DIRECTION('',(1.,0.,0.));
#18612=DIRECTION('',(-1.,0.,0.));
#18613=DIRECTION('',(0.,1.,0.));
#18614=DIRECTION('',(-1.,0.,0.));
#18615=DIRECTION('',(0.,0.,1.));
#18616=DIRECTION('',(0.,-1.,0.));
#18617=DIRECTION('',(-1.71560887364281E-16,0.,-1.));
#18618=DIRECTION('',(1.71560887364281E-16,0.,1.));
#18619=DIRECTION('',(0.,1.,0.));
#18620=DIRECTION('',(0.,0.,1.));
#18621=DIRECTION('',(0.,1.,0.));
#18622=DIRECTION('',(0.,0.,1.));
#18623=DIRECTION('',(0.,1.,0.));
#18624=DIRECTION('',(0.,0.,1.));
#18625=DIRECTION('',(0.,1.,0.));
#18626=DIRECTION('',(0.,0.,1.));
#18627=DIRECTION('',(0.,1.,0.));
#18628=DIRECTION('',(0.,0.,1.));
#18629=DIRECTION('',(0.,1.,0.));
#18630=DIRECTION('',(0.,0.,1.));
#18631=DIRECTION('',(0.,1.,0.));
#18632=DIRECTION('',(0.,0.,1.));
#18633=DIRECTION('',(0.,1.,0.));
#18634=DIRECTION('',(0.,0.,1.));
#18635=DIRECTION('',(0.,1.,0.));
#18636=DIRECTION('',(0.,0.,1.));
#18637=DIRECTION('',(0.,1.,0.));
#18638=DIRECTION('',(0.,0.,1.));
#18639=DIRECTION('',(0.,1.,0.));
#18640=DIRECTION('',(0.,0.,1.));
#18641=DIRECTION('',(0.,1.,0.));
#18642=DIRECTION('',(0.,0.,1.));
#18643=DIRECTION('',(0.,1.,0.));
#18644=DIRECTION('',(0.,0.,1.));
#18645=DIRECTION('',(0.,1.,0.));
#18646=DIRECTION('',(0.,0.,1.));
#18647=DIRECTION('',(0.,1.,0.));
#18648=DIRECTION('',(0.,0.,1.));
#18649=DIRECTION('',(0.,1.,0.));
#18650=DIRECTION('',(0.,0.,1.));
#18651=DIRECTION('',(0.,1.,0.));
#18652=DIRECTION('',(0.,0.,1.));
#18653=DIRECTION('',(0.,1.,0.));
#18654=DIRECTION('',(0.,0.,1.));
#18655=DIRECTION('',(0.,1.,0.));
#18656=DIRECTION('',(0.,0.,1.));
#18657=DIRECTION('',(0.,1.,0.));
#18658=DIRECTION('',(0.,0.,1.));
#18659=DIRECTION('',(0.,1.,0.));
#18660=DIRECTION('',(0.,0.,1.));
#18661=DIRECTION('',(0.,1.,0.));
#18662=DIRECTION('',(0.,0.,1.));
#18663=DIRECTION('',(0.,1.,0.));
#18664=DIRECTION('',(0.,0.,1.));
#18665=DIRECTION('',(0.,1.,0.));
#18666=DIRECTION('',(0.,0.,1.));
#18667=DIRECTION('',(0.,1.,0.));
#18668=DIRECTION('',(0.,0.,1.));
#18669=DIRECTION('',(0.,1.,0.));
#18670=DIRECTION('',(0.,0.,1.));
#18671=DIRECTION('',(0.,1.,0.));
#18672=DIRECTION('',(0.,0.,1.));
#18673=DIRECTION('',(0.,1.,0.));
#18674=DIRECTION('',(0.,0.,1.));
#18675=DIRECTION('',(0.,1.,0.));
#18676=DIRECTION('',(0.,0.,1.));
#18677=DIRECTION('',(0.,1.,0.));
#18678=DIRECTION('',(0.,0.,1.));
#18679=DIRECTION('',(0.,1.,0.));
#18680=DIRECTION('',(0.,0.,1.));
#18681=DIRECTION('',(0.,1.,0.));
#18682=DIRECTION('',(0.,0.,1.));
#18683=DIRECTION('',(0.,1.,0.));
#18684=DIRECTION('',(0.,0.,1.));
#18685=DIRECTION('',(0.,1.,0.));
#18686=DIRECTION('',(0.,0.,1.));
#18687=DIRECTION('',(0.,1.,0.));
#18688=DIRECTION('',(0.,0.,1.));
#18689=DIRECTION('',(0.,1.,0.));
#18690=DIRECTION('',(0.,0.,1.));
#18691=DIRECTION('',(0.,1.,0.));
#18692=DIRECTION('',(0.,0.,1.));
#18693=DIRECTION('',(0.,1.,0.));
#18694=DIRECTION('',(0.,0.,1.));
#18695=DIRECTION('',(0.,1.,0.));
#18696=DIRECTION('',(0.,0.,1.));
#18697=DIRECTION('',(0.,1.,0.));
#18698=DIRECTION('',(0.,0.,1.));
#18699=DIRECTION('',(0.,-1.,0.));
#18700=DIRECTION('',(0.,0.,-1.));
#18701=DIRECTION('',(0.,1.,0.));
#18702=DIRECTION('',(0.,0.,1.));
#18703=DIRECTION('',(-0.537043061103973,0.,0.843554829587309));
#18704=DIRECTION('',(0.843554829587309,0.,0.537043061103973));
#18705=DIRECTION('',(0.905139725284673,-0.425114193731034,0.));
#18706=DIRECTION('',(0.,0.,-1.));
#18707=DIRECTION('',(0.,0.,1.));
#18708=DIRECTION('',(1.,0.,0.));
#18709=DIRECTION('',(0.,0.,1.));
#18710=DIRECTION('',(-1.,0.,0.));
#18711=DIRECTION('',(0.,0.,-1.));
#18712=DIRECTION('',(-1.,0.,0.));
#18713=DIRECTION('',(0.,0.,-1.));
#18714=DIRECTION('',(-1.,0.,0.));
#18715=DIRECTION('',(0.,0.,-1.));
#18716=DIRECTION('',(-1.,0.,0.));
#18717=DIRECTION('',(0.,0.,-1.));
#18718=DIRECTION('',(-1.,0.,0.));
#18719=DIRECTION('',(0.,0.,-1.));
#18720=DIRECTION('',(-1.,0.,0.));
#18721=DIRECTION('',(0.,0.,-1.));
#18722=DIRECTION('',(0.,0.,-1.));
#18723=DIRECTION('',(0.,0.,-1.));
#18724=DIRECTION('',(-1.,0.,0.));
#18725=DIRECTION('',(0.,0.,1.));
#18726=DIRECTION('',(-1.,0.,0.));
#18727=DIRECTION('',(0.,0.,-1.));
#18728=DIRECTION('',(0.,0.,-1.));
#18729=DIRECTION('',(0.,0.,1.));
#18730=DIRECTION('',(1.,0.,0.));
#18731=DIRECTION('',(0.,0.,-1.));
#18732=DIRECTION('',(1.,0.,0.));
#18733=DIRECTION('',(0.,0.,1.));
#18734=DIRECTION('',(1.,0.,0.));
#18735=DIRECTION('',(0.,0.,-1.));
#18736=DIRECTION('',(1.,0.,0.));
#18737=DIRECTION('',(0.,0.,-1.));
#18738=DIRECTION('',(1.,0.,0.));
#18739=DIRECTION('',(0.,0.,-1.));
#18740=DIRECTION('',(-1.,0.,0.));
#18741=DIRECTION('',(0.,0.,-1.));
#18742=DIRECTION('',(1.,0.,0.));
#18743=DIRECTION('',(0.,0.,-1.));
#18744=DIRECTION('',(0.,0.,-1.));
#18745=DIRECTION('',(0.,0.,-1.));
#18746=DIRECTION('',(-1.,0.,0.));
#18747=DIRECTION('',(0.,0.,-1.));
#18748=DIRECTION('',(1.,0.,0.));
#18749=DIRECTION('',(0.,0.,-1.));
#18750=DIRECTION('',(0.,0.,-1.));
#18751=DIRECTION('',(0.,0.,-1.));
#18752=DIRECTION('',(-1.,0.,0.));
#18753=DIRECTION('',(-1.,0.,0.));
#18754=DIRECTION('',(0.,0.,1.));
#18755=DIRECTION('',(-1.,0.,0.));
#18756=DIRECTION('',(0.,0.,-1.));
#18757=DIRECTION('',(-1.,0.,0.));
#18758=DIRECTION('',(0.,0.,1.));
#18759=DIRECTION('',(-1.,1.25767452008318E-14,0.));
#18760=DIRECTION('',(1.,0.,0.));
#18761=DIRECTION('',(0.,0.,-1.));
#18762=DIRECTION('',(-1.,0.,0.));
#18763=DIRECTION('',(-0.866025403784441,0.,0.5));
#18764=DIRECTION('',(0.866025403784441,0.,-0.5));
#18765=DIRECTION('',(0.866025403784439,0.,0.5));
#18766=DIRECTION('',(-0.866025403784439,0.,-0.5));
#18767=DIRECTION('',(0.,0.,1.));
#18768=DIRECTION('',(1.,0.,0.));
#18769=DIRECTION('',(0.,0.,1.));
#18770=DIRECTION('',(0.,0.,-1.));
#18771=DIRECTION('',(0.,1.,0.));
#18772=DIRECTION('',(0.,0.,1.));
#18773=DIRECTION('',(0.,0.,1.));
#18774=DIRECTION('',(0.,1.,0.));
#18775=DIRECTION('',(0.,0.,1.));
#18776=DIRECTION('',(0.,0.,-1.));
#18777=DIRECTION('',(0.,0.,1.));
#18778=DIRECTION('',(1.,0.,0.));
#18779=DIRECTION('',(1.15824759844129E-16,0.,1.));
#18780=DIRECTION('',(1.15824759844129E-16,0.,1.));
#18781=DIRECTION('',(1.,0.,0.));
#18782=DIRECTION('',(-1.15824759844129E-16,0.,-1.));
#18783=DIRECTION('',(0.,0.,-1.));
#18784=DIRECTION('',(-1.,0.,0.));
#18785=DIRECTION('',(0.,0.,-1.));
#18786=DIRECTION('',(-1.,0.,0.));
#18787=DIRECTION('',(0.,0.,1.));
#18788=DIRECTION('',(-1.,0.,0.));
#18789=DIRECTION('',(1.15824759844129E-16,0.,1.));
#18790=DIRECTION('',(1.,0.,0.));
#18791=DIRECTION('',(0.,0.,1.));
#18792=DIRECTION('',(1.,0.,0.));
#18793=DIRECTION('',(0.,0.,-1.));
#18794=DIRECTION('',(0.,0.,-1.));
#18795=DIRECTION('',(-1.,0.,0.));
#18796=DIRECTION('',(0.,0.,1.));
#18797=DIRECTION('',(0.,0.,1.));
#18798=DIRECTION('',(0.,0.,1.));
#18799=DIRECTION('',(1.,0.,0.));
#18800=DIRECTION('',(0.,0.,1.));
#18801=DIRECTION('',(0.,0.,-1.));
#18802=DIRECTION('',(-1.,0.,0.));
#18803=DIRECTION('',(0.,0.,1.));
#18804=DIRECTION('',(1.,0.,0.));
#18805=DIRECTION('',(0.,0.,-1.));
#18806=DIRECTION('',(-1.,0.,0.));
#18807=DIRECTION('',(-1.,0.,0.));
#18808=DIRECTION('',(0.,0.,1.));
#18809=DIRECTION('',(1.,0.,0.));
#18810=DIRECTION('',(1.,0.,0.));
#18811=DIRECTION('',(0.,-1.,0.));
#18812=DIRECTION('',(0.,0.,-1.));
#18813=DIRECTION('',(0.,0.,1.));
#18814=DIRECTION('',(0.,1.,0.));
#18815=DIRECTION('',(0.,0.,1.));
#18816=DIRECTION('',(0.,0.,1.));
#18817=DIRECTION('',(0.,0.,1.));
#18818=DIRECTION('',(1.,0.,0.));
#18819=DIRECTION('',(0.,0.,-1.));
#18820=DIRECTION('',(-1.,0.,0.));
#18821=DIRECTION('',(0.,0.,-1.));
#18822=DIRECTION('',(-1.,0.,0.));
#18823=DIRECTION('',(0.,0.,-1.));
#18824=DIRECTION('',(-1.,0.,0.));
#18825=DIRECTION('',(0.,0.,-1.));
#18826=DIRECTION('',(-1.,0.,0.));
#18827=DIRECTION('',(0.,0.,-1.));
#18828=DIRECTION('',(-1.,0.,0.));
#18829=DIRECTION('',(0.,0.,-1.));
#18830=DIRECTION('',(-1.,0.,0.));
#18831=DIRECTION('',(0.,0.,-1.));
#18832=DIRECTION('',(1.,0.,0.));
#18833=DIRECTION('',(0.,0.,1.));
#18834=DIRECTION('',(1.,0.,0.));
#18835=DIRECTION('',(0.,0.,-1.));
#18836=DIRECTION('',(-1.,0.,0.));
#18837=DIRECTION('',(0.,0.,1.));
#18838=DIRECTION('',(1.,0.,0.));
#18839=DIRECTION('',(0.,0.,1.));
#18840=DIRECTION('',(1.,0.,0.));
#18841=DIRECTION('',(0.,0.,1.));
#18842=DIRECTION('',(1.,0.,0.));
#18843=DIRECTION('',(1.15824759844129E-16,0.,1.));
#18844=DIRECTION('',(1.,0.,0.));
#18845=DIRECTION('',(0.,0.,-1.));
#18846=DIRECTION('',(-1.,0.,0.));
#18847=DIRECTION('',(0.,0.,-1.));
#18848=DIRECTION('',(-1.,0.,0.));
#18849=DIRECTION('',(0.,0.,-1.));
#18850=DIRECTION('',(-1.,0.,0.));
#18851=DIRECTION('',(0.,0.,-1.));
#18852=DIRECTION('',(-1.,0.,0.));
#18853=DIRECTION('',(0.,0.,-1.));
#18854=DIRECTION('',(-1.,0.,0.));
#18855=DIRECTION('',(0.,0.,-1.));
#18856=DIRECTION('',(-1.,0.,0.));
#18857=DIRECTION('',(1.07158798064712E-18,1.57189229981047E-17,1.));
#18858=DIRECTION('',(0.990748195963547,-0.135712977253382,1.0715879806471E-18));
#18859=DIRECTION('',(-0.173648177666933,0.984807753012207,0.));
#18860=DIRECTION('',(-0.984807753012207,-0.173648177666933,0.));
#18861=DIRECTION('',(-0.463976173764915,-0.0818115178406352,-0.882061781128216));
#18862=DIRECTION('',(0.,0.,1.));
#18863=DIRECTION('',(0.984807753012207,0.173648177666933,0.));
#18864=DIRECTION('',(0.463976173764915,0.0818115178406351,0.882061781128216));
#18865=DIRECTION('',(0.,0.,1.));
#18866=DIRECTION('',(0.,0.,1.));
#18867=DIRECTION('',(1.,0.,0.));
#18868=DIRECTION('',(0.,0.,1.));
#18869=DIRECTION('',(1.,0.,0.));
#18870=DIRECTION('',(0.,0.,1.));
#18871=DIRECTION('',(0.,0.,-1.));
#18872=DIRECTION('',(-1.,0.,0.));
#18873=DIRECTION('',(0.98480775301221,-0.17364817766692,0.));
#18874=DIRECTION('',(0.17364817766692,0.98480775301221,0.));
#18875=DIRECTION('',(0.0818115178406285,0.463976173764916,0.882061781128216));
#18876=DIRECTION('',(0.,0.,1.));
#18877=DIRECTION('',(-0.0818115178406284,-0.463976173764916,-0.882061781128216));
#18878=DIRECTION('',(-0.17364817766692,-0.98480775301221,0.));
#18879=DIRECTION('',(0.,0.,1.));
#18880=DIRECTION('',(1.,0.,0.));
#18881=DIRECTION('',(0.,0.,-1.));
#18882=DIRECTION('',(-1.,0.,0.));
#18883=DIRECTION('',(0.,0.,-1.));
#18884=DIRECTION('',(1.,0.,0.));
#18885=DIRECTION('',(-0.173648177666933,0.984807753012207,0.));
#18886=DIRECTION('',(-0.984807753012207,-0.173648177666933,0.));
#18887=DIRECTION('',(0.463976173764915,0.0818115178406386,-0.882061781128216));
#18888=DIRECTION('',(0.,0.,1.));
#18889=DIRECTION('',(-0.984807753012206,-0.173648177666941,0.));
#18890=DIRECTION('',(-0.463976173764914,-0.0818115178406385,0.882061781128216));
#18891=DIRECTION('',(0.,0.,1.));
#18892=DIRECTION('',(0.,0.,1.));
#18893=DIRECTION('',(1.,0.,0.));
#18894=DIRECTION('',(0.,0.,1.));
#18895=DIRECTION('',(1.,0.,0.));
#18896=DIRECTION('',(0.,0.,1.));
#18897=DIRECTION('',(0.,0.,-1.));
#18898=DIRECTION('',(-1.,0.,0.));
#18899=DIRECTION('',(0.98480775301221,-0.17364817766692,0.));
#18900=DIRECTION('',(0.17364817766692,0.98480775301221,0.));
#18901=DIRECTION('',(-0.0818115178406318,-0.463976173764916,0.882061781128216));
#18902=DIRECTION('',(0.,0.,1.));
#18903=DIRECTION('',(0.0818115178406318,0.463976173764915,-0.882061781128216));
#18904=DIRECTION('',(0.173648177666927,0.984807753012209,0.));
#18905=DIRECTION('',(0.,0.,1.));
#18906=DIRECTION('',(1.,0.,0.));
#18907=DIRECTION('',(0.,0.,-1.));
#18908=DIRECTION('',(-1.,0.,0.));
#18909=DIRECTION('',(0.,0.,-1.));
#18910=DIRECTION('',(1.,0.,0.));
#18911=DIRECTION('',(-0.984807753012206,-0.173648177666945,0.));
#18912=DIRECTION('',(0.173648177666945,-0.984807753012206,0.));
#18913=DIRECTION('',(0.0818115178406402,-0.463976173764914,-0.882061781128216));
#18914=DIRECTION('',(0.,0.,1.));
#18915=DIRECTION('',(-0.173648177666945,0.984807753012206,0.));
#18916=DIRECTION('',(-0.0818115178406402,0.463976173764914,0.882061781128216));
#18917=DIRECTION('',(0.,0.,1.));
#18918=DIRECTION('',(0.,0.,1.));
#18919=DIRECTION('',(1.,0.,0.));
#18920=DIRECTION('',(0.,0.,1.));
#18921=DIRECTION('',(1.,0.,0.));
#18922=DIRECTION('',(0.,0.,1.));
#18923=DIRECTION('',(0.,0.,-1.));
#18924=DIRECTION('',(-1.,0.,0.));
#18925=DIRECTION('',(-0.17364817766693,-0.984807753012208,0.));
#18926=DIRECTION('',(0.984807753012208,-0.17364817766693,0.));
#18927=DIRECTION('',(-0.463976173764916,0.0818115178406334,0.882061781128216));
#18928=DIRECTION('',(0.,0.,1.));
#18929=DIRECTION('',(0.463976173764915,-0.0818115178406334,-0.882061781128216));
#18930=DIRECTION('',(0.984807753012208,-0.17364817766693,0.));
#18931=DIRECTION('',(0.,0.,1.));
#18932=DIRECTION('',(1.,0.,0.));
#18933=DIRECTION('',(0.,0.,-1.));
#18934=DIRECTION('',(-1.,0.,0.));
#18935=DIRECTION('',(0.,0.,-1.));
#18936=DIRECTION('',(1.,0.,0.));
#18937=DIRECTION('',(-0.984807753012206,-0.173648177666945,0.));
#18938=DIRECTION('',(0.173648177666945,-0.984807753012206,0.));
#18939=DIRECTION('',(-0.0818115178406369,0.463976173764915,-0.882061781128216));
#18940=DIRECTION('',(0.,0.,1.));
#18941=DIRECTION('',(0.173648177666938,-0.984807753012207,0.));
#18942=DIRECTION('',(0.0818115178406368,-0.463976173764915,0.882061781128216));
#18943=DIRECTION('',(0.,0.,1.));
#18944=DIRECTION('',(0.,0.,1.));
#18945=DIRECTION('',(1.,0.,0.));
#18946=DIRECTION('',(0.,0.,-1.));
#18947=DIRECTION('',(-1.,0.,0.));
#18948=DIRECTION('',(0.,0.,1.));
#18949=DIRECTION('',(0.,0.,-1.));
#18950=DIRECTION('',(-1.,0.,0.));
#18951=DIRECTION('',(-0.17364817766693,-0.984807753012208,0.));
#18952=DIRECTION('',(0.984807753012208,-0.17364817766693,0.));
#18953=DIRECTION('',(0.463976173764916,-0.0818115178406335,0.882061781128216));
#18954=DIRECTION('',(0.,0.,1.));
#18955=DIRECTION('',(-0.463976173764915,0.0818115178406334,-0.882061781128216));
#18956=DIRECTION('',(-0.984807753012208,0.17364817766693,0.));
#18957=DIRECTION('',(0.,0.,1.));
#18958=DIRECTION('',(1.,0.,0.));
#18959=DIRECTION('',(0.,0.,-1.));
#18960=DIRECTION('',(-1.,0.,0.));
#18961=DIRECTION('',(0.,0.,-1.));
#18962=DIRECTION('',(-1.,0.,0.));
#18963=DIRECTION('',(0.,0.,-1.));
#18964=DIRECTION('',(-1.,0.,0.));
#18965=DIRECTION('',(0.,0.,-1.));
#18966=DIRECTION('',(-1.,0.,0.));
#18967=DIRECTION('',(0.,0.,-1.));
#18968=DIRECTION('',(-1.,0.,0.));
#18969=DIRECTION('',(0.,0.,-1.));
#18970=DIRECTION('',(-1.,0.,0.));
#18971=DIRECTION('',(0.,0.,-1.));
#18972=DIRECTION('',(-1.,0.,0.));
#18973=DIRECTION('',(0.,0.,-1.));
#18974=DIRECTION('',(-1.,0.,0.));
#18975=DIRECTION('',(0.,0.,-1.));
#18976=DIRECTION('',(-1.,0.,0.));
#18977=DIRECTION('',(0.,0.,-1.));
#18978=DIRECTION('',(-1.,0.,0.));
#18979=DIRECTION('',(0.,0.,-1.));
#18980=DIRECTION('',(-1.,0.,0.));
#18981=DIRECTION('',(0.,0.,-1.));
#18982=DIRECTION('',(-1.,0.,0.));
#18983=DIRECTION('',(0.,0.,-1.));
#18984=DIRECTION('',(-1.,0.,0.));
#18985=DIRECTION('',(0.,0.,-1.));
#18986=DIRECTION('',(-1.,0.,0.));
#18987=DIRECTION('',(0.,0.,1.));
#18988=DIRECTION('',(1.,0.,0.));
#18989=DIRECTION('',(0.,0.,-1.));
#18990=DIRECTION('',(-1.,0.,0.));
#18991=DIRECTION('',(0.,0.,-1.));
#18992=DIRECTION('',(-1.,0.,0.));
#18993=DIRECTION('',(0.,0.,-1.));
#18994=DIRECTION('',(-1.,0.,0.));
#18995=DIRECTION('',(0.,0.,-1.));
#18996=DIRECTION('',(-1.,0.,0.));
#18997=DIRECTION('',(0.,0.,-1.));
#18998=DIRECTION('',(-1.,0.,0.));
#18999=DIRECTION('',(0.,0.,1.));
#19000=DIRECTION('',(1.,0.,0.));
#19001=DIRECTION('',(0.,0.,-1.));
#19002=DIRECTION('',(-1.,0.,0.));
#19003=DIRECTION('',(0.,0.,-1.));
#19004=DIRECTION('',(-1.,0.,0.));
#19005=DIRECTION('',(0.,0.,-1.));
#19006=DIRECTION('',(-1.,0.,0.));
#19007=DIRECTION('',(0.,0.,-1.));
#19008=DIRECTION('',(-1.,0.,0.));
#19009=DIRECTION('',(0.,0.,-1.));
#19010=DIRECTION('',(-1.,0.,0.));
#19011=DIRECTION('',(0.,0.,-1.));
#19012=DIRECTION('',(-1.,0.,0.));
#19013=DIRECTION('',(0.,0.,-1.));
#19014=DIRECTION('',(-1.,0.,0.));
#19015=DIRECTION('',(0.,0.,-1.));
#19016=DIRECTION('',(-1.,0.,0.));
#19017=DIRECTION('',(0.,0.,-1.));
#19018=DIRECTION('',(-1.,0.,0.));
#19019=DIRECTION('',(0.,0.,-1.));
#19020=DIRECTION('',(-1.,0.,0.));
#19021=DIRECTION('',(0.,0.,-1.));
#19022=DIRECTION('',(-1.,0.,0.));
#19023=DIRECTION('',(0.,0.,-1.));
#19024=DIRECTION('',(-1.,0.,0.));
#19025=DIRECTION('',(0.,0.,-1.));
#19026=DIRECTION('',(-1.,0.,0.));
#19027=DIRECTION('',(0.,0.,-1.));
#19028=DIRECTION('',(-1.,0.,0.));
#19029=DIRECTION('',(0.,0.,-1.));
#19030=DIRECTION('',(-1.,0.,0.));
#19031=DIRECTION('',(0.,0.,-1.));
#19032=DIRECTION('',(-1.,0.,0.));
#19033=DIRECTION('',(0.,0.,-1.));
#19034=DIRECTION('',(-1.,0.,0.));
#19035=DIRECTION('',(0.,0.,1.));
#19036=DIRECTION('',(0.850162458347549,0.526520459637089,0.));
#19037=DIRECTION('',(-0.692749665477858,0.211756051343751,0.689389059747556));
#19038=DIRECTION('',(0.647043889936958,0.604649334921695,0.46447108227962));
#19039=DIRECTION('',(1.,0.,0.));
#19040=DIRECTION('',(0.,0.,-1.));
#19041=DIRECTION('',(1.,0.,0.));
#19042=DIRECTION('',(0.,0.,-1.));
#19043=DIRECTION('',(-0.718059051153575,0.231804019712156,-0.656245453699845));
#19044=DIRECTION('',(0.297719501993842,0.954585044452634,0.0114232674791869));
#19045=DIRECTION('',(0.232156425308651,-0.717834774122639,0.656366232562437));
#19046=DIRECTION('',(0.954423306777422,0.298238056715909,-0.0114110913750513));
#19047=DIRECTION('',(-0.414036995247424,-0.847901151391589,0.331114789816619));
#19048=DIRECTION('',(0.898590191828426,-0.43878886397646,0.));
#19049=DIRECTION('',(1.,0.,0.));
#19050=DIRECTION('',(0.,0.,-1.));
#19051=DIRECTION('',(0.211730516675233,-0.692753880604064,-0.689392666929703));
#19052=DIRECTION('',(0.604625619479393,0.647043750571463,-0.464502147589842));
#19053=DIRECTION('',(-0.0179186792471205,0.0175760353025328,-0.999684952331025));
#19054=DIRECTION('',(-0.999839397961794,0.,0.0179214475809965));
#19055=DIRECTION('',(-0.0175715912801442,0.0178848093900984,-0.999685636974426));
#19056=DIRECTION('',(0.,0.999840004600917,0.0178875710938518));
#19057=DIRECTION('',(0.,0.,-1.));
#19058=DIRECTION('',(-1.,0.,0.));
#19059=DIRECTION('',(0.,0.,-1.));
#19060=DIRECTION('',(-1.,0.,0.));
#19061=DIRECTION('',(0.,0.,1.));
#19062=DIRECTION('',(-1.,0.,0.));
#19063=DIRECTION('',(0.,0.,1.));
#19064=DIRECTION('',(1.,0.,0.));
#19065=DIRECTION('',(0.,0.,-1.));
#19066=DIRECTION('',(1.,0.,0.));
#19067=DIRECTION('',(0.,0.,1.));
#19068=DIRECTION('',(1.,0.,0.));
#19069=DIRECTION('',(0.,0.,1.));
#19070=DIRECTION('',(1.,0.,0.));
#19071=DIRECTION('',(0.,0.,-1.));
#19072=DIRECTION('',(-1.,0.,0.));
#19073=DIRECTION('',(0.,0.,1.));
#19074=DIRECTION('',(1.,0.,0.));
#19075=DIRECTION('',(0.,0.,-1.));
#19076=DIRECTION('',(-1.,0.,0.));
#19077=DIRECTION('',(0.,0.,1.));
#19078=DIRECTION('',(1.,0.,0.));
#19079=DIRECTION('',(0.,0.,-1.));
#19080=DIRECTION('',(1.,0.,0.));
#19081=DIRECTION('',(0.,0.,-1.));
#19082=DIRECTION('',(-1.,0.,0.));
#19083=DIRECTION('',(0.,0.,-1.));
#19084=DIRECTION('',(1.,0.,0.));
#19085=DIRECTION('',(0.,0.,-1.));
#19086=DIRECTION('',(-1.,0.,0.));
#19087=DIRECTION('',(0.,0.,-1.));
#19088=DIRECTION('',(-1.,0.,0.));
#19089=DIRECTION('',(0.,0.,1.));
#19090=DIRECTION('',(1.,0.,0.));
#19091=DIRECTION('',(0.,0.,1.));
#19092=DIRECTION('',(1.,0.,0.));
#19093=DIRECTION('',(0.,0.,1.));
#19094=DIRECTION('',(1.,0.,0.));
#19095=DIRECTION('',(0.,0.,-1.));
#19096=DIRECTION('',(-1.,0.,0.));
#19097=DIRECTION('',(0.,0.,1.));
#19098=DIRECTION('',(0.999932565783082,-0.0116130911674334,0.));
#19099=DIRECTION('',(0.,0.,-1.));
#19100=DIRECTION('',(-1.,0.,0.));
#19101=DIRECTION('',(0.,0.,-1.));
#19102=DIRECTION('',(-1.,0.,0.));
#19103=DIRECTION('',(0.,0.,-1.));
#19104=DIRECTION('',(-1.,0.,0.));
#19105=DIRECTION('',(0.,0.,-1.));
#19106=DIRECTION('',(-1.,0.,0.));
#19107=DIRECTION('',(0.,0.,1.));
#19108=DIRECTION('',(0.986294168521673,0.164996403415776,0.));
#19109=CARTESIAN_POINT('',(0.,0.,0.));
#19110=CARTESIAN_POINT('',(-0.00322675153453757,0.,0.100593750002048));
#19111=CARTESIAN_POINT('',(-0.00322675153453757,0.00133656424801366,0.100500000002048));
#19112=CARTESIAN_POINT('',(-0.00228165789127562,0.00228165789127562,0.100406250002048));
#19113=CARTESIAN_POINT('',(-0.00133656424801366,0.00322675153453757,0.100312500002048));
#19114=CARTESIAN_POINT('',(-1.97581546920762E-19,0.00322675153453757,0.100218750002048));
#19115=CARTESIAN_POINT('',(0.00133656424801366,0.00322675153453757,0.100125000002048));
#19116=CARTESIAN_POINT('',(0.00228165789127562,0.00228165789127562,0.100031250002048));
#19117=CARTESIAN_POINT('',(0.00322675153453757,0.00133656424801366,0.0999375000020484));
#19118=CARTESIAN_POINT('',(0.00322675153453757,3.95163093841525E-19,0.0998437500020484));
#19119=CARTESIAN_POINT('',(0.00322675153453757,-0.00133656424801366,0.0997500000020483));
#19120=CARTESIAN_POINT('',(0.00228165789127562,-0.00228165789127562,0.0996562500020484));
#19121=CARTESIAN_POINT('',(0.00133656424801366,-0.00322675153453757,0.0995625000020484));
#19122=CARTESIAN_POINT('',(5.92744640762287E-19,-0.00322675153453757,0.0994687500020484));
#19123=CARTESIAN_POINT('',(-0.00133656424801366,-0.00322675153453757,0.0993750000020484));
#19124=CARTESIAN_POINT('',(-0.00228165789127562,-0.00228165789127562,0.0992812500020484));
#19125=CARTESIAN_POINT('',(-0.00322675153453757,-0.00133656424801366,0.0991875000020485));
#19126=CARTESIAN_POINT('',(-0.00322675153453757,0.,0.0990937500020484));
#19127=CARTESIAN_POINT('',(-0.00322675153453757,0.00133656424801366,0.0990000000020484));
#19128=CARTESIAN_POINT('',(-0.00228165789127562,0.00228165789127562,0.0989062500020484));
#19129=CARTESIAN_POINT('',(-0.00133656424801366,0.00322675153453757,0.0988125000020484));
#19130=CARTESIAN_POINT('',(-1.97581546920762E-19,0.00322675153453757,0.0987187500020484));
#19131=CARTESIAN_POINT('',(0.00133656424801366,0.00322675153453757,0.0986250000020484));
#19132=CARTESIAN_POINT('',(0.00228165789127562,0.00228165789127562,0.0985312500020484));
#19133=CARTESIAN_POINT('',(0.00322675153453757,0.00133656424801366,0.0984375000020484));
#19134=CARTESIAN_POINT('',(0.00322675153453757,3.95163093841525E-19,0.0983437500020484));
#19135=CARTESIAN_POINT('',(0.00322675153453757,-0.00133656424801366,0.0982500000020484));
#19136=CARTESIAN_POINT('',(0.00228165789127562,-0.00228165789127562,0.0981562500020484));
#19137=CARTESIAN_POINT('',(0.00133656424801366,-0.00322675153453757,0.0980625000020485));
#19138=CARTESIAN_POINT('',(5.92744640762287E-19,-0.00322675153453757,0.0979687500020484));
#19139=CARTESIAN_POINT('',(-0.00133656424801366,-0.00322675153453757,0.0978750000020484));
#19140=CARTESIAN_POINT('',(-0.00228165789127562,-0.00228165789127562,0.0977812500020484));
#19141=CARTESIAN_POINT('',(-0.00322675153453757,-0.00133656424801366,0.0976875000020484));
#19142=CARTESIAN_POINT('',(-0.00322675153453757,0.,0.0975937500020484));
#19143=CARTESIAN_POINT('',(-0.00322675153453757,0.00133656424801366,0.0975000000020484));
#19144=CARTESIAN_POINT('',(-0.00228165789127562,0.00228165789127562,0.0974062500020484));
#19145=CARTESIAN_POINT('',(-0.00133656424801366,0.00322675153453757,0.0973125000020484));
#19146=CARTESIAN_POINT('',(-1.97581546920762E-19,0.00322675153453757,0.0972187500020484));
#19147=CARTESIAN_POINT('',(0.00133656424801366,0.00322675153453757,0.0971250000020484));
#19148=CARTESIAN_POINT('',(0.00228165789127562,0.00228165789127562,0.0970312500020484));
#19149=CARTESIAN_POINT('',(0.00322675153453757,0.00133656424801366,0.0969375000020484));
#19150=CARTESIAN_POINT('',(0.00322675153453757,3.95163093841525E-19,0.0968437500020484));
#19151=CARTESIAN_POINT('',(0.00322675153453757,-0.00133656424801366,0.0967500000020484));
#19152=CARTESIAN_POINT('',(0.00228165789127562,-0.00228165789127562,0.0966562500020484));
#19153=CARTESIAN_POINT('',(0.00133656424801366,-0.00322675153453757,0.0965625000020484));
#19154=CARTESIAN_POINT('',(5.92744640762287E-19,-0.00322675153453757,0.0964687500020484));
#19155=CARTESIAN_POINT('',(-0.00133656424801366,-0.00322675153453757,0.0963750000020484));
#19156=CARTESIAN_POINT('',(-0.00228165789127562,-0.00228165789127562,0.0962812500020484));
#19157=CARTESIAN_POINT('',(-0.00322675153453757,-0.00133656424801366,0.0961875000020484));
#19158=CARTESIAN_POINT('',(-0.00322675153453757,0.,0.0960937500020484));
#19159=CARTESIAN_POINT('',(-0.00322675153453757,0.00133656424801366,0.0960000000020484));
#19160=CARTESIAN_POINT('',(-0.00228165789127562,0.00228165789127562,0.0959062500020484));
#19161=CARTESIAN_POINT('',(-0.00133656424801366,0.00322675153453757,0.0958125000020485));
#19162=CARTESIAN_POINT('',(-1.97581546920762E-19,0.00322675153453757,0.0957187500020484));
#19163=CARTESIAN_POINT('',(0.00133656424801366,0.00322675153453757,0.0956250000020484));
#19164=CARTESIAN_POINT('',(0.00228165789127562,0.00228165789127562,0.0955312500020484));
#19165=CARTESIAN_POINT('',(0.00322675153453757,0.00133656424801366,0.0954375000020484));
#19166=CARTESIAN_POINT('',(0.00322675153453757,3.95163093841525E-19,0.0953437500020484));
#19167=CARTESIAN_POINT('',(-0.00241485272203757,0.,0.100125000004097));
#19168=CARTESIAN_POINT('',(-0.00241485272203757,0.00100026474860155,0.100031250004097));
#19169=CARTESIAN_POINT('',(-0.00170755873531956,0.00170755873531956,0.0999375000040968));
#19170=CARTESIAN_POINT('',(-0.00100026474860155,0.00241485272203757,0.0998437500040967));
#19171=CARTESIAN_POINT('',(-1.47867082822779E-19,0.00241485272203757,0.0997500000040968));
#19172=CARTESIAN_POINT('',(0.00100026474860155,0.00241485272203757,0.0996562500040968));
#19173=CARTESIAN_POINT('',(0.00170755873531956,0.00170755873531956,0.0995625000040968));
#19174=CARTESIAN_POINT('',(0.00241485272203757,0.00100026474860155,0.0994687500040968));
#19175=CARTESIAN_POINT('',(0.00241485272203757,2.95734165645558E-19,0.0993750000040968));
#19176=CARTESIAN_POINT('',(0.00241485272203757,-0.00100026474860155,0.0992812500040967));
#19177=CARTESIAN_POINT('',(0.00170755873531956,-0.00170755873531956,0.0991875000040968));
#19178=CARTESIAN_POINT('',(0.00100026474860155,-0.00241485272203757,0.0990937500040968));
#19179=CARTESIAN_POINT('',(4.43601248468338E-19,-0.00241485272203757,0.0990000000040968));
#19180=CARTESIAN_POINT('',(-0.00100026474860155,-0.00241485272203757,0.0989062500040968));
#19181=CARTESIAN_POINT('',(-0.00170755873531956,-0.00170755873531956,0.0988125000040968));
#19182=CARTESIAN_POINT('',(-0.00241485272203757,-0.00100026474860155,0.0987187500040969));
#19183=CARTESIAN_POINT('',(-0.00241485272203757,0.,0.0986250000040968));
#19184=CARTESIAN_POINT('',(-0.00241485272203757,0.00100026474860155,0.0985312500040968));
#19185=CARTESIAN_POINT('',(-0.00170755873531956,0.00170755873531956,0.0984375000040968));
#19186=CARTESIAN_POINT('',(-0.00100026474860155,0.00241485272203757,0.0983437500040968));
#19187=CARTESIAN_POINT('',(-1.47867082822779E-19,0.00241485272203757,0.0982500000040968));
#19188=CARTESIAN_POINT('',(0.00100026474860155,0.00241485272203757,0.0981562500040967));
#19189=CARTESIAN_POINT('',(0.00170755873531956,0.00170755873531956,0.0980625000040968));
#19190=CARTESIAN_POINT('',(0.00241485272203757,0.00100026474860155,0.0979687500040968));
#19191=CARTESIAN_POINT('',(0.00241485272203757,2.95734165645558E-19,0.0978750000040968));
#19192=CARTESIAN_POINT('',(0.00241485272203757,-0.00100026474860155,0.0977812500040968));
#19193=CARTESIAN_POINT('',(0.00170755873531956,-0.00170755873531956,0.0976875000040968));
#19194=CARTESIAN_POINT('',(0.00100026474860155,-0.00241485272203757,0.0975937500040969));
#19195=CARTESIAN_POINT('',(4.43601248468338E-19,-0.00241485272203757,0.0975000000040968));
#19196=CARTESIAN_POINT('',(-0.00100026474860155,-0.00241485272203757,0.0974062500040968));
#19197=CARTESIAN_POINT('',(-0.00170755873531956,-0.00170755873531956,0.0973125000040968));
#19198=CARTESIAN_POINT('',(-0.00241485272203757,-0.00100026474860155,0.0972187500040968));
#19199=CARTESIAN_POINT('',(-0.00241485272203757,0.,0.0971250000040968));
#19200=CARTESIAN_POINT('',(-0.00241485272203757,0.00100026474860155,0.0970312500040968));
#19201=CARTESIAN_POINT('',(-0.00170755873531956,0.00170755873531956,0.0969375000040968));
#19202=CARTESIAN_POINT('',(-0.00100026474860155,0.00241485272203757,0.0968437500040968));
#19203=CARTESIAN_POINT('',(-1.47867082822779E-19,0.00241485272203757,0.0967500000040968));
#19204=CARTESIAN_POINT('',(0.00100026474860155,0.00241485272203757,0.0966562500040968));
#19205=CARTESIAN_POINT('',(0.00170755873531956,0.00170755873531956,0.0965625000040968));
#19206=CARTESIAN_POINT('',(0.00241485272203757,0.00100026474860155,0.0964687500040968));
#19207=CARTESIAN_POINT('',(0.00241485272203757,2.95734165645558E-19,0.0963750000040968));
#19208=CARTESIAN_POINT('',(0.00241485272203757,-0.00100026474860155,0.0962812500040968));
#19209=CARTESIAN_POINT('',(0.00170755873531956,-0.00170755873531956,0.0961875000040968));
#19210=CARTESIAN_POINT('',(0.00100026474860155,-0.00241485272203757,0.0960937500040968));
#19211=CARTESIAN_POINT('',(4.43601248468338E-19,-0.00241485272203757,0.0960000000040968));
#19212=CARTESIAN_POINT('',(-0.00100026474860155,-0.00241485272203757,0.0959062500040968));
#19213=CARTESIAN_POINT('',(-0.00170755873531956,-0.00170755873531956,0.0958125000040968));
#19214=CARTESIAN_POINT('',(-0.00241485272203757,-0.00100026474860155,0.0957187500040968));
#19215=CARTESIAN_POINT('',(-0.00241485272203757,0.,0.0956250000040968));
#19216=CARTESIAN_POINT('',(-0.00241485272203757,0.00100026474860155,0.0955312500040968));
#19217=CARTESIAN_POINT('',(-0.00170755873531956,0.00170755873531956,0.0954375000040968));
#19218=CARTESIAN_POINT('',(-0.00100026474860155,0.00241485272203757,0.0953437500040968));
#19219=CARTESIAN_POINT('',(-1.47867082822779E-19,0.00241485272203757,0.0952500000040968));
#19220=CARTESIAN_POINT('',(0.00100026474860155,0.00241485272203757,0.0951562500040968));
#19221=CARTESIAN_POINT('',(0.00170755873531956,0.00170755873531956,0.0950625000040968));
#19222=CARTESIAN_POINT('',(0.00241485272203757,0.00100026474860155,0.0949687500040968));
#19223=CARTESIAN_POINT('',(0.00241485272203757,2.95734165645558E-19,0.0948750000040968));
#19224=CARTESIAN_POINT('',(-0.00282080212828757,0.,0.100359375003073));
#19225=CARTESIAN_POINT('',(-0.00322675153453757,0.,0.100593750002048));
#19226=CARTESIAN_POINT('',(-0.00241485272203757,0.,0.100125000004097));
#19227=CARTESIAN_POINT('',(-0.00241485272203757,0.,0.100125000004097));
#19228=CARTESIAN_POINT('',(-0.00241485272203757,0.00100026474860155,0.100031250004097));
#19229=CARTESIAN_POINT('',(-0.00170755873531956,0.00170755873531956,0.0999375000040968));
#19230=CARTESIAN_POINT('',(-0.00100026474860155,0.00241485272203757,0.0998437500040967));
#19231=CARTESIAN_POINT('',(-1.47867082822779E-19,0.00241485272203757,0.0997500000040968));
#19232=CARTESIAN_POINT('',(0.00100026474860155,0.00241485272203757,0.0996562500040968));
#19233=CARTESIAN_POINT('',(0.00170755873531956,0.00170755873531956,0.0995625000040968));
#19234=CARTESIAN_POINT('',(0.00241485272203757,0.00100026474860155,0.0994687500040968));
#19235=CARTESIAN_POINT('',(0.00241485272203757,2.95734165645558E-19,0.0993750000040968));
#19236=CARTESIAN_POINT('',(0.00241485272203757,2.95734165645558E-19,0.0993750000040968));
#19237=CARTESIAN_POINT('',(0.00241485272203757,2.95734165645558E-19,0.0993750000040968));
#19238=CARTESIAN_POINT('',(0.00241485272203757,-0.00100026474860155,0.0992812500040967));
#19239=CARTESIAN_POINT('',(0.00170755873531956,-0.00170755873531956,0.0991875000040968));
#19240=CARTESIAN_POINT('',(0.00100026474860155,-0.00241485272203757,0.0990937500040968));
#19241=CARTESIAN_POINT('',(4.43601248468338E-19,-0.00241485272203757,0.0990000000040968));
#19242=CARTESIAN_POINT('',(-0.00100026474860155,-0.00241485272203757,0.0989062500040968));
#19243=CARTESIAN_POINT('',(-0.00170755873531956,-0.00170755873531956,0.0988125000040968));
#19244=CARTESIAN_POINT('',(-0.00241485272203757,-0.00100026474860155,0.0987187500040969));
#19245=CARTESIAN_POINT('',(-0.00241485272203757,0.,0.0986250000040968));
#19246=CARTESIAN_POINT('',(-0.00241485272203757,0.,0.0986250000040968));
#19247=CARTESIAN_POINT('',(-0.00241485272203757,0.,0.0986250000040968));
#19248=CARTESIAN_POINT('',(-0.00241485272203757,0.00100026474860155,0.0985312500040968));
#19249=CARTESIAN_POINT('',(-0.00170755873531956,0.00170755873531956,0.0984375000040968));
#19250=CARTESIAN_POINT('',(-0.00100026474860155,0.00241485272203757,0.0983437500040968));
#19251=CARTESIAN_POINT('',(-1.47867082822779E-19,0.00241485272203757,0.0982500000040968));
#19252=CARTESIAN_POINT('',(0.00100026474860155,0.00241485272203757,0.0981562500040967));
#19253=CARTESIAN_POINT('',(0.00170755873531956,0.00170755873531956,0.0980625000040968));
#19254=CARTESIAN_POINT('',(0.00241485272203757,0.00100026474860155,0.0979687500040968));
#19255=CARTESIAN_POINT('',(0.00241485272203757,2.95734165645558E-19,0.0978750000040968));
#19256=CARTESIAN_POINT('',(0.00241485272203757,2.95734165645558E-19,0.0978750000040968));
#19257=CARTESIAN_POINT('',(0.00241485272203757,2.95734165645558E-19,0.0978750000040968));
#19258=CARTESIAN_POINT('',(0.00241485272203757,-0.00100026474860154,0.0977812500040968));
#19259=CARTESIAN_POINT('',(0.00170755873531956,-0.00170755873531956,0.0976875000040968));
#19260=CARTESIAN_POINT('',(0.00100026474860155,-0.00241485272203757,0.0975937500040969));
#19261=CARTESIAN_POINT('',(4.43601248468338E-19,-0.00241485272203757,0.0975000000040968));
#19262=CARTESIAN_POINT('',(-0.00100026474860155,-0.00241485272203757,0.0974062500040968));
#19263=CARTESIAN_POINT('',(-0.00170755873531956,-0.00170755873531956,0.0973125000040968));
#19264=CARTESIAN_POINT('',(-0.00241485272203757,-0.00100026474860155,0.0972187500040968));
#19265=CARTESIAN_POINT('',(-0.00241485272203757,0.,0.0971250000040968));
#19266=CARTESIAN_POINT('',(-0.00241485272203757,0.,0.0971250000040968));
#19267=CARTESIAN_POINT('',(-0.00241485272203757,0.,0.0971250000040968));
#19268=CARTESIAN_POINT('',(-0.00241485272203757,0.00100026474860155,0.0970312500040967));
#19269=CARTESIAN_POINT('',(-0.00170755873531956,0.00170755873531956,0.0969375000040968));
#19270=CARTESIAN_POINT('',(-0.00100026474860155,0.00241485272203757,0.0968437500040968));
#19271=CARTESIAN_POINT('',(-1.47867082822779E-19,0.00241485272203757,0.0967500000040968));
#19272=CARTESIAN_POINT('',(0.00100026474860155,0.00241485272203757,0.0966562500040968));
#19273=CARTESIAN_POINT('',(0.00170755873531956,0.00170755873531956,0.0965625000040968));
#19274=CARTESIAN_POINT('',(0.00241485272203757,0.00100026474860155,0.0964687500040968));
#19275=CARTESIAN_POINT('',(0.00241485272203757,2.95734165645558E-19,0.0963750000040968));
#19276=CARTESIAN_POINT('',(0.00241485272203757,2.95734165645558E-19,0.0963750000040968));
#19277=CARTESIAN_POINT('',(0.00241485272203757,2.95734165645558E-19,0.0963750000040968));
#19278=CARTESIAN_POINT('',(0.00241485272203757,-0.00100026474860155,0.0962812500040968));
#19279=CARTESIAN_POINT('',(0.00170755873531956,-0.00170755873531956,0.0961875000040968));
#19280=CARTESIAN_POINT('',(0.00100026474860155,-0.00241485272203757,0.0960937500040968));
#19281=CARTESIAN_POINT('',(4.43601248468338E-19,-0.00241485272203757,0.0960000000040968));
#19282=CARTESIAN_POINT('',(-0.00100026474860155,-0.00241485272203757,0.0959062500040968));
#19283=CARTESIAN_POINT('',(-0.00170755873531956,-0.00170755873531956,0.0958125000040968));
#19284=CARTESIAN_POINT('',(-0.00241485272203757,-0.00100026474860155,0.0957187500040968));
#19285=CARTESIAN_POINT('',(-0.00241485272203757,0.,0.0956250000040968));
#19286=CARTESIAN_POINT('',(-0.00241485272203757,0.,0.0956250000040968));
#19287=CARTESIAN_POINT('',(-0.00241485272203757,0.,0.0956250000040968));
#19288=CARTESIAN_POINT('',(-0.00241485272203757,0.00100026474860155,0.0955312500040968));
#19289=CARTESIAN_POINT('',(-0.00170755873531956,0.00170755873531956,0.0954375000040968));
#19290=CARTESIAN_POINT('',(-0.00100026474860155,0.00241485272203757,0.0953437500040968));
#19291=CARTESIAN_POINT('',(-1.47867082822779E-19,0.00241485272203757,0.0952500000040968));
#19292=CARTESIAN_POINT('',(0.00100026474860155,0.00241485272203757,0.0951562500040968));
#19293=CARTESIAN_POINT('',(0.00170755873531956,0.00170755873531956,0.0950625000040968));
#19294=CARTESIAN_POINT('',(0.00241485272203757,0.00100026474860155,0.0949687500040968));
#19295=CARTESIAN_POINT('',(0.00241485272203757,2.95734165645558E-19,0.0948750000040968));
#19296=CARTESIAN_POINT('',(0.00241485272203757,2.21800624234168E-19,0.0948750000040968));
#19297=CARTESIAN_POINT('',(0.00282080212828757,3.45448629743542E-19,0.0951093750030726));
#19298=CARTESIAN_POINT('',(0.00322675153453757,3.95163093841525E-19,0.0953437500020484));
#19299=CARTESIAN_POINT('',(-0.00322675153453757,0.,0.100593750002048));
#19300=CARTESIAN_POINT('',(-0.00322675153453757,0.00133656424801366,0.100500000002048));
#19301=CARTESIAN_POINT('',(-0.00228165789127562,0.00228165789127562,0.100406250002048));
#19302=CARTESIAN_POINT('',(-0.00133656424801366,0.00322675153453757,0.100312500002048));
#19303=CARTESIAN_POINT('',(-1.97581546920762E-19,0.00322675153453757,0.100218750002048));
#19304=CARTESIAN_POINT('',(0.00133656424801366,0.00322675153453757,0.100125000002048));
#19305=CARTESIAN_POINT('',(0.00228165789127562,0.00228165789127562,0.100031250002048));
#19306=CARTESIAN_POINT('',(0.00322675153453757,0.00133656424801366,0.0999375000020484));
#19307=CARTESIAN_POINT('',(0.00322675153453757,3.95163093841525E-19,0.0998437500020484));
#19308=CARTESIAN_POINT('',(0.00322675153453757,-0.00133656424801366,0.0997500000020483));
#19309=CARTESIAN_POINT('',(0.00228165789127562,-0.00228165789127562,0.0996562500020484));
#19310=CARTESIAN_POINT('',(0.00133656424801366,-0.00322675153453757,0.0995625000020484));
#19311=CARTESIAN_POINT('',(5.92744640762287E-19,-0.00322675153453757,0.0994687500020484));
#19312=CARTESIAN_POINT('',(-0.00133656424801366,-0.00322675153453757,0.0993750000020484));
#19313=CARTESIAN_POINT('',(-0.00228165789127562,-0.00228165789127562,0.0992812500020484));
#19314=CARTESIAN_POINT('',(-0.00322675153453757,-0.00133656424801366,0.0991875000020485));
#19315=CARTESIAN_POINT('',(-0.00322675153453757,0.,0.0990937500020484));
#19316=CARTESIAN_POINT('',(-0.00322675153453757,0.00133656424801366,0.0990000000020484));
#19317=CARTESIAN_POINT('',(-0.00228165789127562,0.00228165789127562,0.0989062500020484));
#19318=CARTESIAN_POINT('',(-0.00133656424801366,0.00322675153453757,0.0988125000020484));
#19319=CARTESIAN_POINT('',(-1.97581546920762E-19,0.00322675153453757,0.0987187500020484));
#19320=CARTESIAN_POINT('',(0.00133656424801366,0.00322675153453757,0.0986250000020484));
#19321=CARTESIAN_POINT('',(0.00228165789127562,0.00228165789127562,0.0985312500020484));
#19322=CARTESIAN_POINT('',(0.00322675153453757,0.00133656424801366,0.0984375000020484));
#19323=CARTESIAN_POINT('',(0.00322675153453757,3.95163093841525E-19,0.0983437500020484));
#19324=CARTESIAN_POINT('',(0.00322675153453757,-0.00133656424801366,0.0982500000020484));
#19325=CARTESIAN_POINT('',(0.00228165789127562,-0.00228165789127562,0.0981562500020484));
#19326=CARTESIAN_POINT('',(0.00133656424801366,-0.00322675153453757,0.0980625000020485));
#19327=CARTESIAN_POINT('',(5.92744640762287E-19,-0.00322675153453757,0.0979687500020484));
#19328=CARTESIAN_POINT('',(-0.00133656424801366,-0.00322675153453757,0.0978750000020484));
#19329=CARTESIAN_POINT('',(-0.00228165789127562,-0.00228165789127562,0.0977812500020484));
#19330=CARTESIAN_POINT('',(-0.00322675153453757,-0.00133656424801366,0.0976875000020484));
#19331=CARTESIAN_POINT('',(-0.00322675153453757,0.,0.0975937500020484));
#19332=CARTESIAN_POINT('',(-0.00322675153453757,0.00133656424801366,0.0975000000020484));
#19333=CARTESIAN_POINT('',(-0.00228165789127562,0.00228165789127562,0.0974062500020484));
#19334=CARTESIAN_POINT('',(-0.00133656424801366,0.00322675153453757,0.0973125000020484));
#19335=CARTESIAN_POINT('',(-1.97581546920762E-19,0.00322675153453757,0.0972187500020484));
#19336=CARTESIAN_POINT('',(0.00133656424801366,0.00322675153453757,0.0971250000020484));
#19337=CARTESIAN_POINT('',(0.00228165789127562,0.00228165789127562,0.0970312500020484));
#19338=CARTESIAN_POINT('',(0.00322675153453757,0.00133656424801366,0.0969375000020483));
#19339=CARTESIAN_POINT('',(0.00322675153453757,3.95163093841525E-19,0.0968437500020484));
#19340=CARTESIAN_POINT('',(0.00322675153453757,-0.00133656424801366,0.0967500000020484));
#19341=CARTESIAN_POINT('',(0.00228165789127562,-0.00228165789127562,0.0966562500020484));
#19342=CARTESIAN_POINT('',(0.00133656424801366,-0.00322675153453757,0.0965625000020484));
#19343=CARTESIAN_POINT('',(5.92744640762287E-19,-0.00322675153453757,0.0964687500020484));
#19344=CARTESIAN_POINT('',(-0.00133656424801366,-0.00322675153453757,0.0963750000020484));
#19345=CARTESIAN_POINT('',(-0.00228165789127562,-0.00228165789127562,0.0962812500020484));
#19346=CARTESIAN_POINT('',(-0.00322675153453757,-0.00133656424801366,0.0961875000020484));
#19347=CARTESIAN_POINT('',(-0.00322675153453757,0.,0.0960937500020484));
#19348=CARTESIAN_POINT('',(-0.00322675153453757,0.00133656424801366,0.0960000000020484));
#19349=CARTESIAN_POINT('',(-0.00228165789127562,0.00228165789127562,0.0959062500020484));
#19350=CARTESIAN_POINT('',(-0.00133656424801366,0.00322675153453757,0.0958125000020485));
#19351=CARTESIAN_POINT('',(-1.97581546920762E-19,0.00322675153453757,0.0957187500020484));
#19352=CARTESIAN_POINT('',(0.00133656424801366,0.00322675153453757,0.0956250000020484));
#19353=CARTESIAN_POINT('',(0.00228165789127562,0.00228165789127562,0.0955312500020484));
#19354=CARTESIAN_POINT('',(0.00322675153453757,0.00133656424801366,0.0954375000020484));
#19355=CARTESIAN_POINT('',(0.00322675153453757,3.95163093841525E-19,0.0953437500020484));
#19356=CARTESIAN_POINT('',(1.0842021724855E-18,-4.33680868994202E-18,0.0996930389370738));
#19357=CARTESIAN_POINT('',(-0.00322675153453757,0.,0.100687500002048));
#19358=CARTESIAN_POINT('',(-0.00322675153453757,0.,0.100781250002048));
#19359=CARTESIAN_POINT('',(0.00322675153453757,3.95163093841525E-19,0.0954375000020484));
#19360=CARTESIAN_POINT('',(0.00322675153453757,3.95163093841525E-19,0.0955312500020484));
#19361=CARTESIAN_POINT('',(-0.00322675153453757,0.,0.100781250002048));
#19362=CARTESIAN_POINT('',(-0.00322675153453757,0.00133656424801366,0.100687500002048));
#19363=CARTESIAN_POINT('',(-0.00228165789127562,0.00228165789127562,0.100593750002048));
#19364=CARTESIAN_POINT('',(-0.00133656424801366,0.00322675153453757,0.100500000002048));
#19365=CARTESIAN_POINT('',(-1.97581546920762E-19,0.00322675153453757,0.100406250002048));
#19366=CARTESIAN_POINT('',(0.00133656424801366,0.00322675153453757,0.100312500002048));
#19367=CARTESIAN_POINT('',(0.00228165789127562,0.00228165789127562,0.100218750002048));
#19368=CARTESIAN_POINT('',(0.00322675153453757,0.00133656424801366,0.100125000002048));
#19369=CARTESIAN_POINT('',(0.00322675153453757,3.95163093841525E-19,0.100031250002048));
#19370=CARTESIAN_POINT('',(0.00322675153453757,-0.00133656424801366,0.0999375000020484));
#19371=CARTESIAN_POINT('',(0.00228165789127562,-0.00228165789127562,0.0998437500020484));
#19372=CARTESIAN_POINT('',(0.00133656424801366,-0.00322675153453757,0.0997500000020483));
#19373=CARTESIAN_POINT('',(5.92744640762287E-19,-0.00322675153453757,0.0996562500020484));
#19374=CARTESIAN_POINT('',(-0.00133656424801366,-0.00322675153453757,0.0995625000020484));
#19375=CARTESIAN_POINT('',(-0.00228165789127562,-0.00228165789127562,0.0994687500020484));
#19376=CARTESIAN_POINT('',(-0.00322675153453757,-0.00133656424801366,0.0993750000020484));
#19377=CARTESIAN_POINT('',(-0.00322675153453757,0.,0.0992812500020484));
#19378=CARTESIAN_POINT('',(-0.00322675153453757,0.00133656424801366,0.0991875000020483));
#19379=CARTESIAN_POINT('',(-0.00228165789127562,0.00228165789127562,0.0990937500020484));
#19380=CARTESIAN_POINT('',(-0.00133656424801366,0.00322675153453757,0.0990000000020484));
#19381=CARTESIAN_POINT('',(-1.97581546920762E-19,0.00322675153453757,0.0989062500020484));
#19382=CARTESIAN_POINT('',(0.00133656424801366,0.00322675153453757,0.0988125000020484));
#19383=CARTESIAN_POINT('',(0.00228165789127562,0.00228165789127562,0.0987187500020484));
#19384=CARTESIAN_POINT('',(0.00322675153453757,0.00133656424801366,0.0986250000020484));
#19385=CARTESIAN_POINT('',(0.00322675153453757,3.95163093841525E-19,0.0985312500020484));
#19386=CARTESIAN_POINT('',(0.00322675153453757,-0.00133656424801366,0.0984375000020484));
#19387=CARTESIAN_POINT('',(0.00228165789127562,-0.00228165789127562,0.0983437500020484));
#19388=CARTESIAN_POINT('',(0.00133656424801366,-0.00322675153453757,0.0982500000020484));
#19389=CARTESIAN_POINT('',(5.92744640762287E-19,-0.00322675153453757,0.0981562500020484));
#19390=CARTESIAN_POINT('',(-0.00133656424801366,-0.00322675153453757,0.0980625000020483));
#19391=CARTESIAN_POINT('',(-0.00228165789127562,-0.00228165789127562,0.0979687500020484));
#19392=CARTESIAN_POINT('',(-0.00322675153453757,-0.00133656424801366,0.0978750000020484));
#19393=CARTESIAN_POINT('',(-0.00322675153453757,0.,0.0977812500020484));
#19394=CARTESIAN_POINT('',(-0.00322675153453757,0.00133656424801366,0.0976875000020484));
#19395=CARTESIAN_POINT('',(-0.00228165789127562,0.00228165789127562,0.0975937500020484));
#19396=CARTESIAN_POINT('',(-0.00133656424801366,0.00322675153453757,0.0975000000020484));
#19397=CARTESIAN_POINT('',(-1.97581546920762E-19,0.00322675153453757,0.0974062500020484));
#19398=CARTESIAN_POINT('',(0.00133656424801366,0.00322675153453757,0.0973125000020484));
#19399=CARTESIAN_POINT('',(0.00228165789127562,0.00228165789127562,0.0972187500020484));
#19400=CARTESIAN_POINT('',(0.00322675153453757,0.00133656424801366,0.0971250000020484));
#19401=CARTESIAN_POINT('',(0.00322675153453757,3.95163093841525E-19,0.0970312500020484));
#19402=CARTESIAN_POINT('',(0.00322675153453757,-0.00133656424801366,0.0969375000020483));
#19403=CARTESIAN_POINT('',(0.00228165789127562,-0.00228165789127562,0.0968437500020484));
#19404=CARTESIAN_POINT('',(0.00133656424801366,-0.00322675153453757,0.0967500000020484));
#19405=CARTESIAN_POINT('',(5.92744640762287E-19,-0.00322675153453757,0.0966562500020484));
#19406=CARTESIAN_POINT('',(-0.00133656424801366,-0.00322675153453757,0.0965625000020484));
#19407=CARTESIAN_POINT('',(-0.00228165789127562,-0.00228165789127562,0.0964687500020484));
#19408=CARTESIAN_POINT('',(-0.00322675153453757,-0.00133656424801366,0.0963750000020484));
#19409=CARTESIAN_POINT('',(-0.00322675153453757,0.,0.0962812500020484));
#19410=CARTESIAN_POINT('',(-0.00322675153453757,0.00133656424801366,0.0961875000020484));
#19411=CARTESIAN_POINT('',(-0.00228165789127562,0.00228165789127562,0.0960937500020484));
#19412=CARTESIAN_POINT('',(-0.00133656424801366,0.00322675153453757,0.0960000000020484));
#19413=CARTESIAN_POINT('',(-1.97581546920762E-19,0.00322675153453757,0.0959062500020484));
#19414=CARTESIAN_POINT('',(0.00133656424801366,0.00322675153453757,0.0958125000020483));
#19415=CARTESIAN_POINT('',(0.00228165789127562,0.00228165789127562,0.0957187500020484));
#19416=CARTESIAN_POINT('',(0.00322675153453757,0.00133656424801366,0.0956250000020484));
#19417=CARTESIAN_POINT('',(0.00322675153453757,3.95163093841525E-19,0.0955312500020484));
#19418=CARTESIAN_POINT('',(0.00322675153453757,3.95163093841525E-19,0.0953906250020484));
#19419=CARTESIAN_POINT('',(0.00241485272203757,2.95734165645558E-19,0.107));
#19420=CARTESIAN_POINT('',(0.00241485272203757,2.21800624234168E-19,0.096));
#19421=CARTESIAN_POINT('',(0.00282080212828757,3.45448629743542E-19,0.0957656250010242));
#19422=CARTESIAN_POINT('',(-0.00241485272203757,0.,0.10125));
#19423=CARTESIAN_POINT('',(-0.00241485272203757,0.00100026474860155,0.10115625));
#19424=CARTESIAN_POINT('',(-0.00170755873531956,0.00170755873531956,0.1010625));
#19425=CARTESIAN_POINT('',(-0.00100026474860155,0.00241485272203757,0.10096875));
#19426=CARTESIAN_POINT('',(-1.47867082822779E-19,0.00241485272203757,0.100875));
#19427=CARTESIAN_POINT('',(0.00100026474860155,0.00241485272203757,0.10078125));
#19428=CARTESIAN_POINT('',(0.00170755873531956,0.00170755873531956,0.1006875));
#19429=CARTESIAN_POINT('',(0.00241485272203757,0.00100026474860155,0.10059375));
#19430=CARTESIAN_POINT('',(0.00241485272203757,2.95734165645558E-19,0.1005));
#19431=CARTESIAN_POINT('',(0.00241485272203757,-0.00100026474860155,0.10040625));
#19432=CARTESIAN_POINT('',(0.00170755873531956,-0.00170755873531956,0.1003125));
#19433=CARTESIAN_POINT('',(0.00100026474860155,-0.00241485272203757,0.10021875));
#19434=CARTESIAN_POINT('',(4.43601248468338E-19,-0.00241485272203757,0.100125));
#19435=CARTESIAN_POINT('',(-0.00100026474860155,-0.00241485272203757,0.10003125));
#19436=CARTESIAN_POINT('',(-0.00170755873531956,-0.00170755873531956,0.0999375));
#19437=CARTESIAN_POINT('',(-0.00241485272203757,-0.00100026474860155,0.09984375));
#19438=CARTESIAN_POINT('',(-0.00241485272203757,0.,0.09975));
#19439=CARTESIAN_POINT('',(-0.00241485272203757,0.00100026474860155,0.0996562500000001));
#19440=CARTESIAN_POINT('',(-0.00170755873531956,0.00170755873531956,0.0995625));
#19441=CARTESIAN_POINT('',(-0.00100026474860155,0.00241485272203757,0.09946875));
#19442=CARTESIAN_POINT('',(-1.47867082822779E-19,0.00241485272203757,0.099375));
#19443=CARTESIAN_POINT('',(0.00100026474860155,0.00241485272203757,0.09928125));
#19444=CARTESIAN_POINT('',(0.00170755873531956,0.00170755873531956,0.0991875));
#19445=CARTESIAN_POINT('',(0.00241485272203757,0.00100026474860155,0.0990937499999999));
#19446=CARTESIAN_POINT('',(0.00241485272203757,2.95734165645558E-19,0.099));
#19447=CARTESIAN_POINT('',(0.00241485272203757,-0.00100026474860155,0.09890625));
#19448=CARTESIAN_POINT('',(0.00170755873531956,-0.00170755873531956,0.0988125));
#19449=CARTESIAN_POINT('',(0.00100026474860155,-0.00241485272203757,0.09871875));
#19450=CARTESIAN_POINT('',(4.43601248468338E-19,-0.00241485272203757,0.098625));
#19451=CARTESIAN_POINT('',(-0.00100026474860155,-0.00241485272203757,0.09853125));
#19452=CARTESIAN_POINT('',(-0.00170755873531956,-0.00170755873531956,0.0984375));
#19453=CARTESIAN_POINT('',(-0.00241485272203757,-0.00100026474860155,0.09834375));
#19454=CARTESIAN_POINT('',(-0.00241485272203757,0.,0.09825));
#19455=CARTESIAN_POINT('',(-0.00241485272203757,0.00100026474860155,0.09815625));
#19456=CARTESIAN_POINT('',(-0.00170755873531956,0.00170755873531956,0.0980625));
#19457=CARTESIAN_POINT('',(-0.00100026474860155,0.00241485272203757,0.09796875));
#19458=CARTESIAN_POINT('',(-1.47867082822779E-19,0.00241485272203757,0.097875));
#19459=CARTESIAN_POINT('',(0.00100026474860155,0.00241485272203757,0.09778125));
#19460=CARTESIAN_POINT('',(0.00170755873531956,0.00170755873531956,0.0976875));
#19461=CARTESIAN_POINT('',(0.00241485272203757,0.00100026474860155,0.09759375));
#19462=CARTESIAN_POINT('',(0.00241485272203757,2.95734165645558E-19,0.0975));
#19463=CARTESIAN_POINT('',(0.00241485272203757,-0.00100026474860155,0.0974062500000001));
#19464=CARTESIAN_POINT('',(0.00170755873531956,-0.00170755873531956,0.0973125));
#19465=CARTESIAN_POINT('',(0.00100026474860155,-0.00241485272203757,0.09721875));
#19466=CARTESIAN_POINT('',(4.43601248468338E-19,-0.00241485272203757,0.097125));
#19467=CARTESIAN_POINT('',(-0.00100026474860155,-0.00241485272203757,0.09703125));
#19468=CARTESIAN_POINT('',(-0.00170755873531956,-0.00170755873531956,0.0969375));
#19469=CARTESIAN_POINT('',(-0.00241485272203757,-0.00100026474860155,0.09684375));
#19470=CARTESIAN_POINT('',(-0.00241485272203757,0.,0.09675));
#19471=CARTESIAN_POINT('',(-0.00241485272203757,0.00100026474860155,0.09665625));
#19472=CARTESIAN_POINT('',(-0.00170755873531956,0.00170755873531956,0.0965625));
#19473=CARTESIAN_POINT('',(-0.00100026474860155,0.00241485272203757,0.09646875));
#19474=CARTESIAN_POINT('',(-1.47867082822779E-19,0.00241485272203757,0.096375));
#19475=CARTESIAN_POINT('',(0.00100026474860155,0.00241485272203757,0.0962812500000001));
#19476=CARTESIAN_POINT('',(0.00170755873531956,0.00170755873531956,0.0961875));
#19477=CARTESIAN_POINT('',(0.00241485272203757,0.00100026474860155,0.09609375));
#19478=CARTESIAN_POINT('',(0.00241485272203757,2.95734165645558E-19,0.096));
#19479=CARTESIAN_POINT('',(-0.00322675153453757,0.,0.100781250002048));
#19480=CARTESIAN_POINT('',(-0.00322675153453757,0.00133656424801366,0.100687500002048));
#19481=CARTESIAN_POINT('',(-0.00228165789127562,0.00228165789127562,0.100593750002048));
#19482=CARTESIAN_POINT('',(-0.00133656424801366,0.00322675153453757,0.100500000002048));
#19483=CARTESIAN_POINT('',(-1.97581546920762E-19,0.00322675153453757,0.100406250002048));
#19484=CARTESIAN_POINT('',(0.00133656424801366,0.00322675153453757,0.100312500002048));
#19485=CARTESIAN_POINT('',(0.00228165789127562,0.00228165789127562,0.100218750002048));
#19486=CARTESIAN_POINT('',(0.00322675153453757,0.00133656424801366,0.100125000002048));
#19487=CARTESIAN_POINT('',(0.00322675153453757,3.95163093841525E-19,0.100031250002048));
#19488=CARTESIAN_POINT('',(0.00322675153453757,-0.00133656424801366,0.0999375000020484));
#19489=CARTESIAN_POINT('',(0.00228165789127562,-0.00228165789127562,0.0998437500020484));
#19490=CARTESIAN_POINT('',(0.00133656424801366,-0.00322675153453757,0.0997500000020483));
#19491=CARTESIAN_POINT('',(5.92744640762287E-19,-0.00322675153453757,0.0996562500020484));
#19492=CARTESIAN_POINT('',(-0.00133656424801366,-0.00322675153453757,0.0995625000020484));
#19493=CARTESIAN_POINT('',(-0.00228165789127562,-0.00228165789127562,0.0994687500020484));
#19494=CARTESIAN_POINT('',(-0.00322675153453757,-0.00133656424801366,0.0993750000020484));
#19495=CARTESIAN_POINT('',(-0.00322675153453757,0.,0.0992812500020484));
#19496=CARTESIAN_POINT('',(-0.00322675153453757,0.00133656424801366,0.0991875000020483));
#19497=CARTESIAN_POINT('',(-0.00228165789127562,0.00228165789127562,0.0990937500020484));
#19498=CARTESIAN_POINT('',(-0.00133656424801366,0.00322675153453757,0.0990000000020484));
#19499=CARTESIAN_POINT('',(-1.97581546920762E-19,0.00322675153453757,0.0989062500020484));
#19500=CARTESIAN_POINT('',(0.00133656424801366,0.00322675153453757,0.0988125000020484));
#19501=CARTESIAN_POINT('',(0.00228165789127562,0.00228165789127562,0.0987187500020484));
#19502=CARTESIAN_POINT('',(0.00322675153453757,0.00133656424801366,0.0986250000020484));
#19503=CARTESIAN_POINT('',(0.00322675153453757,3.95163093841525E-19,0.0985312500020484));
#19504=CARTESIAN_POINT('',(0.00322675153453757,-0.00133656424801366,0.0984375000020484));
#19505=CARTESIAN_POINT('',(0.00228165789127562,-0.00228165789127562,0.0983437500020484));
#19506=CARTESIAN_POINT('',(0.00133656424801366,-0.00322675153453757,0.0982500000020484));
#19507=CARTESIAN_POINT('',(5.92744640762287E-19,-0.00322675153453757,0.0981562500020484));
#19508=CARTESIAN_POINT('',(-0.00133656424801366,-0.00322675153453757,0.0980625000020485));
#19509=CARTESIAN_POINT('',(-0.00228165789127562,-0.00228165789127562,0.0979687500020484));
#19510=CARTESIAN_POINT('',(-0.00322675153453757,-0.00133656424801366,0.0978750000020484));
#19511=CARTESIAN_POINT('',(-0.00322675153453757,0.,0.0977812500020484));
#19512=CARTESIAN_POINT('',(-0.00322675153453757,0.00133656424801366,0.0976875000020484));
#19513=CARTESIAN_POINT('',(-0.00228165789127562,0.00228165789127562,0.0975937500020484));
#19514=CARTESIAN_POINT('',(-0.00133656424801366,0.00322675153453757,0.0975000000020484));
#19515=CARTESIAN_POINT('',(-1.97581546920762E-19,0.00322675153453757,0.0974062500020484));
#19516=CARTESIAN_POINT('',(0.00133656424801366,0.00322675153453757,0.0973125000020484));
#19517=CARTESIAN_POINT('',(0.00228165789127562,0.00228165789127562,0.0972187500020484));
#19518=CARTESIAN_POINT('',(0.00322675153453757,0.00133656424801366,0.0971250000020484));
#19519=CARTESIAN_POINT('',(0.00322675153453757,3.95163093841525E-19,0.0970312500020484));
#19520=CARTESIAN_POINT('',(0.00322675153453757,-0.00133656424801366,0.0969375000020484));
#19521=CARTESIAN_POINT('',(0.00228165789127562,-0.00228165789127562,0.0968437500020484));
#19522=CARTESIAN_POINT('',(0.00133656424801366,-0.00322675153453757,0.0967500000020484));
#19523=CARTESIAN_POINT('',(5.92744640762287E-19,-0.00322675153453757,0.0966562500020484));
#19524=CARTESIAN_POINT('',(-0.00133656424801366,-0.00322675153453757,0.0965625000020484));
#19525=CARTESIAN_POINT('',(-0.00228165789127562,-0.00228165789127562,0.0964687500020484));
#19526=CARTESIAN_POINT('',(-0.00322675153453757,-0.00133656424801366,0.0963750000020484));
#19527=CARTESIAN_POINT('',(-0.00322675153453757,0.,0.0962812500020484));
#19528=CARTESIAN_POINT('',(-0.00322675153453757,0.00133656424801366,0.0961875000020484));
#19529=CARTESIAN_POINT('',(-0.00228165789127562,0.00228165789127562,0.0960937500020484));
#19530=CARTESIAN_POINT('',(-0.00133656424801366,0.00322675153453757,0.0960000000020484));
#19531=CARTESIAN_POINT('',(-1.97581546920762E-19,0.00322675153453757,0.0959062500020484));
#19532=CARTESIAN_POINT('',(0.00133656424801366,0.00322675153453757,0.0958125000020483));
#19533=CARTESIAN_POINT('',(0.00228165789127562,0.00228165789127562,0.0957187500020484));
#19534=CARTESIAN_POINT('',(0.00322675153453757,0.00133656424801366,0.0956250000020484));
#19535=CARTESIAN_POINT('',(0.00322675153453757,3.95163093841525E-19,0.0955312500020484));
#19536=CARTESIAN_POINT('',(-0.00120116781157934,0.00209492471405489,0.101));
#19537=CARTESIAN_POINT('',(-0.00208526276506858,0.00177414214407331,0.101));
#19538=CARTESIAN_POINT('',(-0.00271974082590136,0.000930774313530578,0.101));
#19539=CARTESIAN_POINT('',(-0.00284786542392977,0.,0.101));
#19540=CARTESIAN_POINT('',(-0.00120116781157934,0.00209492471405489,0.101));
#19541=CARTESIAN_POINT('',(-0.00284786542392979,0.,0.101));
#19542=CARTESIAN_POINT('',(-0.00282080212828757,0.,0.101015625001024));
#19543=CARTESIAN_POINT('',(-0.00241485272203757,0.,0.09675));
#19544=CARTESIAN_POINT('',(-0.00241485272203757,0.00100026474860155,0.09665625));
#19545=CARTESIAN_POINT('',(-0.00170755873531956,0.00170755873531956,0.0965625));
#19546=CARTESIAN_POINT('',(-0.00100026474860155,0.00241485272203757,0.09646875));
#19547=CARTESIAN_POINT('',(-1.47867082822779E-19,0.00241485272203757,0.096375));
#19548=CARTESIAN_POINT('',(0.00100026474860155,0.00241485272203757,0.0962812500000001));
#19549=CARTESIAN_POINT('',(0.00170755873531956,0.00170755873531956,0.0961875));
#19550=CARTESIAN_POINT('',(0.00241485272203757,0.00100026474860155,0.09609375));
#19551=CARTESIAN_POINT('',(0.00241485272203757,2.95734165645558E-19,0.096));
#19552=CARTESIAN_POINT('',(-0.00241485272203757,0.,0.09675));
#19553=CARTESIAN_POINT('',(0.00241485272203757,2.95734165645558E-19,0.0975));
#19554=CARTESIAN_POINT('',(0.00241485272203757,-0.00100026474860155,0.0974062500000001));
#19555=CARTESIAN_POINT('',(0.00170755873531956,-0.00170755873531956,0.0973125));
#19556=CARTESIAN_POINT('',(0.00100026474860155,-0.00241485272203757,0.09721875));
#19557=CARTESIAN_POINT('',(4.43601248468338E-19,-0.00241485272203757,0.097125));
#19558=CARTESIAN_POINT('',(-0.00100026474860155,-0.00241485272203757,0.09703125));
#19559=CARTESIAN_POINT('',(-0.00170755873531956,-0.00170755873531956,0.0969375));
#19560=CARTESIAN_POINT('',(-0.00241485272203757,-0.00100026474860155,0.09684375));
#19561=CARTESIAN_POINT('',(-0.00241485272203757,0.,0.09675));
#19562=CARTESIAN_POINT('',(0.00241485272203757,2.95734165645558E-19,0.0975));
#19563=CARTESIAN_POINT('',(-0.00241485272203757,0.,0.09825));
#19564=CARTESIAN_POINT('',(-0.00241485272203757,0.00100026474860155,0.09815625));
#19565=CARTESIAN_POINT('',(-0.00170755873531956,0.00170755873531956,0.0980625));
#19566=CARTESIAN_POINT('',(-0.00100026474860155,0.00241485272203757,0.09796875));
#19567=CARTESIAN_POINT('',(-1.47867082822779E-19,0.00241485272203757,0.097875));
#19568=CARTESIAN_POINT('',(0.00100026474860155,0.00241485272203757,0.09778125));
#19569=CARTESIAN_POINT('',(0.00170755873531956,0.00170755873531956,0.0976875));
#19570=CARTESIAN_POINT('',(0.00241485272203757,0.00100026474860155,0.09759375));
#19571=CARTESIAN_POINT('',(0.00241485272203757,2.95734165645558E-19,0.0975));
#19572=CARTESIAN_POINT('',(-0.00241485272203757,0.,0.09825));
#19573=CARTESIAN_POINT('',(0.00241485272203757,2.95734165645558E-19,0.099));
#19574=CARTESIAN_POINT('',(0.00241485272203757,-0.00100026474860155,0.09890625));
#19575=CARTESIAN_POINT('',(0.00170755873531956,-0.00170755873531956,0.0988125));
#19576=CARTESIAN_POINT('',(0.00100026474860155,-0.00241485272203757,0.09871875));
#19577=CARTESIAN_POINT('',(4.43601248468338E-19,-0.00241485272203757,0.098625));
#19578=CARTESIAN_POINT('',(-0.00100026474860155,-0.00241485272203757,0.0985312500000001));
#19579=CARTESIAN_POINT('',(-0.00170755873531956,-0.00170755873531956,0.0984375));
#19580=CARTESIAN_POINT('',(-0.00241485272203757,-0.00100026474860155,0.09834375));
#19581=CARTESIAN_POINT('',(-0.00241485272203757,0.,0.09825));
#19582=CARTESIAN_POINT('',(0.00241485272203757,2.95734165645558E-19,0.099));
#19583=CARTESIAN_POINT('',(-0.00241485272203757,0.,0.09975));
#19584=CARTESIAN_POINT('',(-0.00241485272203757,0.00100026474860155,0.0996562500000001));
#19585=CARTESIAN_POINT('',(-0.00170755873531956,0.00170755873531956,0.0995625));
#19586=CARTESIAN_POINT('',(-0.00100026474860155,0.00241485272203757,0.09946875));
#19587=CARTESIAN_POINT('',(-1.47867082822779E-19,0.00241485272203757,0.099375));
#19588=CARTESIAN_POINT('',(0.00100026474860155,0.00241485272203757,0.09928125));
#19589=CARTESIAN_POINT('',(0.00170755873531956,0.00170755873531956,0.0991875));
#19590=CARTESIAN_POINT('',(0.00241485272203757,0.00100026474860155,0.0990937499999999));
#19591=CARTESIAN_POINT('',(0.00241485272203757,2.95734165645558E-19,0.099));
#19592=CARTESIAN_POINT('',(-0.00241485272203757,0.,0.09975));
#19593=CARTESIAN_POINT('',(0.00241485272203757,2.95734165645558E-19,0.1005));
#19594=CARTESIAN_POINT('',(0.00241485272203757,-0.00100026474860155,0.10040625));
#19595=CARTESIAN_POINT('',(0.00170755873531956,-0.00170755873531956,0.1003125));
#19596=CARTESIAN_POINT('',(0.00100026474860155,-0.00241485272203757,0.10021875));
#19597=CARTESIAN_POINT('',(4.43601248468338E-19,-0.00241485272203757,0.100125));
#19598=CARTESIAN_POINT('',(-0.00100026474860155,-0.00241485272203757,0.10003125));
#19599=CARTESIAN_POINT('',(-0.00170755873531956,-0.00170755873531956,0.0999375));
#19600=CARTESIAN_POINT('',(-0.00241485272203757,-0.00100026474860155,0.09984375));
#19601=CARTESIAN_POINT('',(-0.00241485272203757,0.,0.09975));
#19602=CARTESIAN_POINT('',(0.00241485272203757,2.95734165645558E-19,0.1005));
#19603=CARTESIAN_POINT('',(-0.00120116781157934,0.00209492471405489,0.101));
#19604=CARTESIAN_POINT('',(-0.000643189913586848,0.00241485272203757,0.100935283094534));
#19605=CARTESIAN_POINT('',(-1.47867082822779E-19,0.00241485272203757,0.100875));
#19606=CARTESIAN_POINT('',(0.00100026474860155,0.00241485272203757,0.10078125));
#19607=CARTESIAN_POINT('',(0.00170755873531956,0.00170755873531956,0.1006875));
#19608=CARTESIAN_POINT('',(0.00241485272203757,0.00100026474860155,0.10059375));
#19609=CARTESIAN_POINT('',(0.00241485272203757,2.95734165645558E-19,0.1005));
#19610=CARTESIAN_POINT('',(0.00322675153453757,3.95163093841525E-19,0.0953906250020484));
#19611=CARTESIAN_POINT('',(-0.00241485272203757,0.,0.100687500002048));
#19612=CARTESIAN_POINT('',(-0.00241485272203757,9.85780552151861E-20,0.101));
#19613=CARTESIAN_POINT('',(0.,0.,0.101));
#19614=CARTESIAN_POINT('',(0.,0.00455,0.101));
#19615=CARTESIAN_POINT('',(0.,0.,0.101));
#19616=CARTESIAN_POINT('',(-0.00455,0.,0.101));
#19617=CARTESIAN_POINT('',(0.,0.,0.101));
#19618=CARTESIAN_POINT('',(-1.00349973962234E-18,-0.00241485272203757,0.09473856967));
#19619=CARTESIAN_POINT('',(0.00482970544407513,-0.00241485272203757,0.09473856967));
#19620=CARTESIAN_POINT('',(0.00482970544407514,0.00241485272203756,0.09473856967));
#19621=CARTESIAN_POINT('',(2.95093640562077E-18,0.00241485272203757,0.09473856967));
#19622=CARTESIAN_POINT('',(-2.19497575959325E-18,-0.00241485272203757,0.0945272023210931));
#19623=CARTESIAN_POINT('',(0.00482970544407514,-0.00241485272203757,0.094527202321093));
#19624=CARTESIAN_POINT('',(0.00482970544407514,0.00241485272203757,0.094527202321093));
#19625=CARTESIAN_POINT('',(1.2443477489079E-18,0.00241485272203757,0.0945272023210931));
#19626=CARTESIAN_POINT('',(-3.39567156950461E-18,-0.00248323514802505,0.0943272023210931));
#19627=CARTESIAN_POINT('',(0.00496647029605009,-0.00248323514802505,0.0943272023210931));
#19628=CARTESIAN_POINT('',(0.0049664702960501,0.00248323514802504,0.0943272023210931));
#19629=CARTESIAN_POINT('',(-3.49524386054981E-19,0.00248323514802505,0.0943272023210931));
#19630=CARTESIAN_POINT('',(-4.60558716935644E-18,-0.00262,0.09413856967));
#19631=CARTESIAN_POINT('',(0.00524,-0.00262000000000001,0.09413856967));
#19632=CARTESIAN_POINT('',(0.00524000000000001,0.00262,0.09413856967));
#19633=CARTESIAN_POINT('',(-1.83067999926848E-18,0.00262,0.09413856967));
#19634=CARTESIAN_POINT('',(-3.08295813511083E-19,-0.00241485272203757,0.09473856967));
#19635=CARTESIAN_POINT('',(-2.95734165645558E-19,-0.00241485272203757,0.0944215186466397));
#19636=CARTESIAN_POINT('',(-3.20857461376607E-19,-0.00262,0.09413856967));
#19637=CARTESIAN_POINT('',(-3.08295813511083E-19,-0.00241485272203757,0.09473856967));
#19638=CARTESIAN_POINT('',(-3.20857461376607E-19,-0.00262,0.09413856967));
#19639=CARTESIAN_POINT('',(0.,0.,0.09473856967));
#19640=CARTESIAN_POINT('',(0.,0.00241485272203757,0.09473856967));
#19641=CARTESIAN_POINT('',(0.,0.00241485272203757,0.09473856967));
#19642=CARTESIAN_POINT('',(0.,0.00241485272203757,0.0944215186466397));
#19643=CARTESIAN_POINT('',(0.,0.00262,0.09413856967));
#19644=CARTESIAN_POINT('',(0.,0.00262,0.09413856967));
#19645=CARTESIAN_POINT('',(0.,0.,0.09413856967));
#19646=CARTESIAN_POINT('',(0.,0.00262,0.09413856967));
#19647=CARTESIAN_POINT('',(0.,0.,0.09413856967));
#19648=CARTESIAN_POINT('',(0.,0.,0.09413856967));
#19649=CARTESIAN_POINT('',(0.00455,0.,0.09413856967));
#19650=CARTESIAN_POINT('',(0.,0.,0.1029));
#19651=CARTESIAN_POINT('',(0.,0.,0.1029));
#19652=CARTESIAN_POINT('',(0.00455,0.,0.1029));
#19653=CARTESIAN_POINT('',(0.,0.,0.1029));
#19654=CARTESIAN_POINT('',(0.00505,0.,0.1029));
#19655=CARTESIAN_POINT('',(-0.0337929399400243,0.0154689110867544,0.073));
#19656=CARTESIAN_POINT('',(-0.0320429399400243,0.0185,0.083));
#19657=CARTESIAN_POINT('',(-0.0337929399400243,0.0154689110867544,0.083));
#19658=CARTESIAN_POINT('',(-0.0302929399400243,0.0215310889132454,0.083));
#19659=CARTESIAN_POINT('',(-0.0302929399400243,0.0215310889132454,0.073));
#19660=CARTESIAN_POINT('',(-0.0302929399400243,0.0215310889132454,0.081));
#19661=CARTESIAN_POINT('',(-0.0320429399400243,0.0185,0.081));
#19662=CARTESIAN_POINT('',(-0.0337929399400243,0.0154689110867544,0.081));
#19663=CARTESIAN_POINT('',(-0.0337929399400243,0.0154689110867544,0.073));
#19664=CARTESIAN_POINT('',(-0.0355249907475932,0.0164689110867544,0.073));
#19665=CARTESIAN_POINT('',(-0.0337749907475932,0.0195,0.083));
#19666=CARTESIAN_POINT('',(-0.0320249907475932,0.0225310889132454,0.083));
#19667=CARTESIAN_POINT('',(-0.0355249907475932,0.0164689110867544,0.083));
#19668=CARTESIAN_POINT('',(-0.0355249907475932,0.0164689110867544,0.073));
#19669=CARTESIAN_POINT('',(-0.0355249907475932,0.0164689110867544,0.081));
#19670=CARTESIAN_POINT('',(-0.0337749907475932,0.0195,0.081));
#19671=CARTESIAN_POINT('',(-0.0320249907475932,0.0225310889132454,0.081));
#19672=CARTESIAN_POINT('',(-0.0320249907475932,0.0225310889132454,0.073));
#19673=CARTESIAN_POINT('',(-0.0346589653438087,0.0159689110867544,0.073));
#19674=CARTESIAN_POINT('',(-0.0346589653438087,0.0159689110867544,0.083));
#19675=CARTESIAN_POINT('',(-0.0346589653438087,0.0159689110867544,0.081));
#19676=CARTESIAN_POINT('',(0.00350000000000026,-0.037,0.073));
#19677=CARTESIAN_POINT('',(2.393918396848E-16,-0.037,0.083));
#19678=CARTESIAN_POINT('',(0.00350000000000026,-0.037,0.083));
#19679=CARTESIAN_POINT('',(-0.00349999999999974,-0.037,0.083));
#19680=CARTESIAN_POINT('',(-0.00349999999999974,-0.037,0.073));
#19681=CARTESIAN_POINT('',(-0.00349999999999974,-0.037,0.081));
#19682=CARTESIAN_POINT('',(2.393918396848E-16,-0.037,0.081));
#19683=CARTESIAN_POINT('',(0.00350000000000026,-0.037,0.081));
#19684=CARTESIAN_POINT('',(0.00350000000000026,-0.037,0.073));
#19685=CARTESIAN_POINT('',(0.00350000000000027,-0.039,0.073));
#19686=CARTESIAN_POINT('',(2.74086309204335E-16,-0.039,0.083));
#19687=CARTESIAN_POINT('',(-0.00349999999999973,-0.039,0.083));
#19688=CARTESIAN_POINT('',(0.00350000000000028,-0.039,0.083));
#19689=CARTESIAN_POINT('',(0.00350000000000027,-0.039,0.073));
#19690=CARTESIAN_POINT('',(0.00350000000000028,-0.039,0.081));
#19691=CARTESIAN_POINT('',(2.74086309204335E-16,-0.039,0.081));
#19692=CARTESIAN_POINT('',(-0.00349999999999973,-0.039,0.081));
#19693=CARTESIAN_POINT('',(-0.00349999999999972,-0.039,0.073));
#19694=CARTESIAN_POINT('',(0.00350000000000027,-0.038,0.073));
#19695=CARTESIAN_POINT('',(0.00350000000000027,-0.038,0.083));
#19696=CARTESIAN_POINT('',(0.00350000000000027,-0.038,0.081));
#19697=CARTESIAN_POINT('',(0.0302929399400243,0.0215310889132454,0.073));
#19698=CARTESIAN_POINT('',(0.0320429399400243,0.0185,0.083));
#19699=CARTESIAN_POINT('',(0.0302929399400243,0.0215310889132454,0.083));
#19700=CARTESIAN_POINT('',(0.0337929399400242,0.0154689110867544,0.083));
#19701=CARTESIAN_POINT('',(0.0337929399400242,0.0154689110867544,0.073));
#19702=CARTESIAN_POINT('',(0.0337929399400242,0.0154689110867544,0.081));
#19703=CARTESIAN_POINT('',(0.0320429399400243,0.0185,0.081));
#19704=CARTESIAN_POINT('',(0.0302929399400243,0.0215310889132454,0.081));
#19705=CARTESIAN_POINT('',(0.0302929399400243,0.0215310889132454,0.073));
#19706=CARTESIAN_POINT('',(0.0320249907475932,0.0225310889132454,0.073));
#19707=CARTESIAN_POINT('',(0.0337749907475932,0.0195,0.083));
#19708=CARTESIAN_POINT('',(0.0355249907475932,0.0164689110867544,0.083));
#19709=CARTESIAN_POINT('',(0.0320249907475932,0.0225310889132454,0.083));
#19710=CARTESIAN_POINT('',(0.0320249907475932,0.0225310889132454,0.073));
#19711=CARTESIAN_POINT('',(0.0320249907475932,0.0225310889132454,0.081));
#19712=CARTESIAN_POINT('',(0.0337749907475932,0.0195,0.081));
#19713=CARTESIAN_POINT('',(0.0355249907475932,0.0164689110867544,0.081));
#19714=CARTESIAN_POINT('',(0.0355249907475932,0.0164689110867544,0.073));
#19715=CARTESIAN_POINT('',(0.0311589653438087,0.0220310889132454,0.073));
#19716=CARTESIAN_POINT('',(0.0311589653438087,0.0220310889132454,0.083));
#19717=CARTESIAN_POINT('',(0.0311589653438087,0.0220310889132454,0.081));
#19718=CARTESIAN_POINT('',(4.47686656242088E-16,-0.044397,0.0815014));
#19719=CARTESIAN_POINT('',(-1.32786462810487E-16,0.043,0.0815014));
#19720=CARTESIAN_POINT('',(-1.43180183778462E-16,0.04597688,0.0815014));
#19721=CARTESIAN_POINT('',(-1.32786462810487E-16,0.043,0.0815014));
#19722=CARTESIAN_POINT('',(-1.3766406224085E-16,0.044397,0.0815014));
#19723=CARTESIAN_POINT('',(4.47686656242088E-16,-0.044397,0.0815014));
#19724=CARTESIAN_POINT('',(-0.043,1.7347234759768E-17,0.0815014));
#19725=CARTESIAN_POINT('',(-0.04597688,1.7347234759768E-17,0.0815014));
#19726=CARTESIAN_POINT('',(-0.043,1.7347234759768E-17,0.0815014));
#19727=CARTESIAN_POINT('',(-0.044397,1.7347234759768E-17,0.0815014));
#19728=CARTESIAN_POINT('',(4.47686656242088E-16,-0.044397,0.0815014));
#19729=CARTESIAN_POINT('',(4.33053857950996E-16,-0.043,0.0815014));
#19730=CARTESIAN_POINT('',(4.64235020854922E-16,-0.04597688,0.0815014));
#19731=CARTESIAN_POINT('',(4.33053857950996E-16,-0.043,0.0815014));
#19732=CARTESIAN_POINT('',(4.47686656242088E-16,-0.044397,0.0815014));
#19733=CARTESIAN_POINT('',(4.47686656242088E-16,-0.044397,0.0815014));
#19734=CARTESIAN_POINT('',(0.043,-1.7347234759768E-17,0.0815014));
#19735=CARTESIAN_POINT('',(0.04597688,-1.7347234759768E-17,0.0815014));
#19736=CARTESIAN_POINT('',(0.043,-1.7347234759768E-17,0.0815014));
#19737=CARTESIAN_POINT('',(0.044397,-1.7347234759768E-17,0.0815014));
#19738=CARTESIAN_POINT('',(0.,0.,0.081));
#19739=CARTESIAN_POINT('',(-0.02598076211353,-0.0150000000000018,0.081));
#19740=CARTESIAN_POINT('',(-0.0219807621135261,-0.0150000000000018,0.081));
#19741=CARTESIAN_POINT('',(0.0259807621135363,-0.0149999999999982,0.081));
#19742=CARTESIAN_POINT('',(0.029980762113539,-0.0149999999999982,0.081));
#19743=CARTESIAN_POINT('',(0.,0.03,0.081));
#19744=CARTESIAN_POINT('',(0.004,0.03,0.081));
#19745=CARTESIAN_POINT('',(0.,0.,0.081));
#19746=CARTESIAN_POINT('',(0.00755,0.,0.081));
#19747=CARTESIAN_POINT('',(0.,0.,0.081));
#19748=CARTESIAN_POINT('',(0.05,0.,0.081));
#19749=CARTESIAN_POINT('',(0.043,-1.7347234759768E-17,0.081));
#19750=CARTESIAN_POINT('',(0.044397,-1.7347234759768E-17,0.081));
#19751=CARTESIAN_POINT('',(4.33053857950996E-16,-0.043,0.081));
#19752=CARTESIAN_POINT('',(4.47686656242088E-16,-0.044397,0.081));
#19753=CARTESIAN_POINT('',(-0.043,1.7347234759768E-17,0.081));
#19754=CARTESIAN_POINT('',(-0.044397,1.7347234759768E-17,0.081));
#19755=CARTESIAN_POINT('',(-1.32786462810487E-16,0.043,0.081));
#19756=CARTESIAN_POINT('',(-1.3766406224085E-16,0.044397,0.081));
#19757=CARTESIAN_POINT('',(0.0346589653438087,0.0159689110867544,0.081));
#19758=CARTESIAN_POINT('',(-0.00349999999999973,-0.038,0.081));
#19759=CARTESIAN_POINT('',(-0.0311589653438087,0.0220310889132454,0.081));
#19760=CARTESIAN_POINT('',(-0.0175,0.0303108891324553,0.081));
#19761=CARTESIAN_POINT('',(-0.0075,0.0303108891324553,0.081));
#19762=CARTESIAN_POINT('',(0.,0.,0.083));
#19763=CARTESIAN_POINT('',(-0.02598076211353,-0.0150000000000018,0.083));
#19764=CARTESIAN_POINT('',(-0.0219807621135261,-0.0150000000000018,0.083));
#19765=CARTESIAN_POINT('',(0.,0.03,0.083));
#19766=CARTESIAN_POINT('',(0.004,0.03,0.083));
#19767=CARTESIAN_POINT('',(0.,0.,0.083));
#19768=CARTESIAN_POINT('',(0.05,0.,0.083));
#19769=CARTESIAN_POINT('',(0.,0.,0.083));
#19770=CARTESIAN_POINT('',(0.00755,0.,0.083));
#19771=CARTESIAN_POINT('',(0.0259807621135363,-0.0149999999999982,0.083));
#19772=CARTESIAN_POINT('',(0.029980762113539,-0.0149999999999982,0.083));
#19773=CARTESIAN_POINT('',(0.043,-1.7347234759768E-17,0.083));
#19774=CARTESIAN_POINT('',(0.04597688,-1.7347234759768E-17,0.083));
#19775=CARTESIAN_POINT('',(4.33053857950996E-16,-0.043,0.083));
#19776=CARTESIAN_POINT('',(4.64235020854922E-16,-0.04597688,0.083));
#19777=CARTESIAN_POINT('',(-0.043,1.7347234759768E-17,0.083));
#19778=CARTESIAN_POINT('',(-0.04597688,1.7347234759768E-17,0.083));
#19779=CARTESIAN_POINT('',(-1.32786462810487E-16,0.043,0.083));
#19780=CARTESIAN_POINT('',(-1.43180183778462E-16,0.04597688,0.083));
#19781=CARTESIAN_POINT('',(0.0346589653438087,0.0159689110867544,0.083));
#19782=CARTESIAN_POINT('',(-0.00349999999999973,-0.038,0.083));
#19783=CARTESIAN_POINT('',(-0.0311589653438087,0.0220310889132454,0.083));
#19784=CARTESIAN_POINT('',(-0.0175,0.0303108891324553,0.083));
#19785=CARTESIAN_POINT('',(-0.0075,0.0303108891324553,0.083));
#19786=CARTESIAN_POINT('',(0.,0.,0.107));
#19787=CARTESIAN_POINT('',(0.,0.,0.107));
#19788=CARTESIAN_POINT('',(0.00755,0.,0.107));
#19789=CARTESIAN_POINT('',(0.,0.,0.107));
#19790=CARTESIAN_POINT('',(0.00505,0.,0.107));
#19791=CARTESIAN_POINT('',(0.,0.,0.073));
#19792=CARTESIAN_POINT('',(0.,0.,0.073));
#19793=CARTESIAN_POINT('',(0.00755,0.,0.073));
#19794=CARTESIAN_POINT('',(0.,0.,0.073));
#19795=CARTESIAN_POINT('',(0.00555,0.,0.073));
#19796=CARTESIAN_POINT('',(0.,0.,0.073));
#19797=CARTESIAN_POINT('',(0.,0.,0.074));
#19798=CARTESIAN_POINT('',(0.00455,0.,0.074));
#19799=CARTESIAN_POINT('',(0.,0.,0.073));
#19800=CARTESIAN_POINT('',(0.,0.,0.073));
#19801=CARTESIAN_POINT('',(0.,0.,0.073));
#19802=CARTESIAN_POINT('',(0.,0.,0.083));
#19803=CARTESIAN_POINT('',(0.,0.03,0.083));
#19804=CARTESIAN_POINT('',(0.0259807621135363,-0.0149999999999982,0.083));
#19805=CARTESIAN_POINT('',(-0.02598076211353,-0.0150000000000018,0.083));
#19806=CARTESIAN_POINT('',(0.043,-1.7347234759768E-17,0.083));
#19807=CARTESIAN_POINT('',(0.043,-1.7347234759768E-17,0.083));
#19808=CARTESIAN_POINT('',(4.33053857950996E-16,-0.043,0.083));
#19809=CARTESIAN_POINT('',(4.33053857950996E-16,-0.043,0.083));
#19810=CARTESIAN_POINT('',(-0.043,1.7347234759768E-17,0.083));
#19811=CARTESIAN_POINT('',(-0.043,1.7347234759768E-17,0.083));
#19812=CARTESIAN_POINT('',(-1.32786462810487E-16,0.043,0.083));
#19813=CARTESIAN_POINT('',(-1.32786462810487E-16,0.043,0.083));
#19814=CARTESIAN_POINT('',(0.0346589653438087,0.0159689110867544,0.073));
#19815=CARTESIAN_POINT('',(-0.00349999999999973,-0.038,0.073));
#19816=CARTESIAN_POINT('',(-0.0311589653438087,0.0220310889132454,0.073));
#19817=CARTESIAN_POINT('',(-0.0175,0.0303108891324553,0.107));
#19818=CARTESIAN_POINT('',(0.,0.,0.1029));
#19819=CARTESIAN_POINT('',(0.,0.,0.107));
#19820=CARTESIAN_POINT('',(0.,0.,0.09473856967));
#19821=CARTESIAN_POINT('',(0.,0.,0.074));
#19822=CARTESIAN_POINT('',(1.42442054663212E-18,0.00241485272203757,0.09473856967));
#19823=CARTESIAN_POINT('',(-0.00482970544407513,0.00241485272203757,0.09473856967));
#19824=CARTESIAN_POINT('',(-0.00482970544407514,-0.00241485272203756,0.09473856967));
#19825=CARTESIAN_POINT('',(-3.37185721263055E-18,-0.00241485272203757,0.09473856967));
#19826=CARTESIAN_POINT('',(2.61589656660303E-18,0.00241485272203757,0.0945272023210931));
#19827=CARTESIAN_POINT('',(-0.00482970544407514,0.00241485272203757,0.094527202321093));
#19828=CARTESIAN_POINT('',(-0.00482970544407514,-0.00241485272203757,0.094527202321093));
#19829=CARTESIAN_POINT('',(-1.66526855591768E-18,-0.00241485272203757,0.0945272023210931));
#19830=CARTESIAN_POINT('',(3.8165923765144E-18,0.00248323514802505,0.0943272023210931));
#19831=CARTESIAN_POINT('',(-0.00496647029605009,0.00248323514802505,0.0943272023210931));
#19832=CARTESIAN_POINT('',(-0.0049664702960501,-0.00248323514802504,0.0943272023210931));
#19833=CARTESIAN_POINT('',(-7.13964209548004E-20,-0.00248323514802505,0.0943272023210931));
#19834=CARTESIAN_POINT('',(5.02650797636622E-18,0.00262,0.09413856967));
#19835=CARTESIAN_POINT('',(-0.00524,0.00262000000000001,0.09413856967));
#19836=CARTESIAN_POINT('',(-0.00524000000000001,-0.00262,0.09413856967));
#19837=CARTESIAN_POINT('',(1.4097591922587E-18,-0.00262,0.09413856967));
#19838=CARTESIAN_POINT('',(0.,0.,0.));
#19839=CARTESIAN_POINT('',(0.00604745574900122,0.,0.06762567913));
#19840=CARTESIAN_POINT('',(8.28175714867204E-18,0.,0.06762567913));
#19841=CARTESIAN_POINT('',(0.00450000000000001,0.,0.06762567913));
#19842=CARTESIAN_POINT('',(6.5911382126792E-18,0.,0.06762567913));
#19843=CARTESIAN_POINT('',(0.00380000000000001,0.,0.06762567913));
#19844=CARTESIAN_POINT('',(0.00604745574900122,0.,0.06622567913));
#19845=CARTESIAN_POINT('',(8.11030659679141E-18,0.,0.06622567913));
#19846=CARTESIAN_POINT('',(-0.00449999999999999,0.,0.06622567913));
#19847=CARTESIAN_POINT('',(6.00804404586185E-18,0.,0.06622567913));
#19848=CARTESIAN_POINT('',(-0.00379999999999999,0.,0.06622567913));
#19849=CARTESIAN_POINT('',(-0.00748201094464286,0.,0.0501919291324776));
#19850=CARTESIAN_POINT('',(-0.00748201094464285,0.00243105272334464,0.0501012148467632));
#19851=CARTESIAN_POINT('',(-0.00605307400631542,0.00439781569075195,0.050010500561049));
#19852=CARTESIAN_POINT('',(-0.00462413706798799,0.00636457865815926,0.0499197862753347));
#19853=CARTESIAN_POINT('',(-0.00231206853399399,0.00711581526389425,0.0498290719896204));
#19854=CARTESIAN_POINT('',(5.60947406115009E-18,0.00786705186962924,0.0497383577039061));
#19855=CARTESIAN_POINT('',(0.00231206853399401,0.00711581526389425,0.0496476434181919));
#19856=CARTESIAN_POINT('',(0.004624137067988,0.00636457865815926,0.0495569291324775));
#19857=CARTESIAN_POINT('',(0.00605307400631544,0.00439781569075195,0.0494662148467633));
#19858=CARTESIAN_POINT('',(0.00748201094464287,0.00243105272334464,0.049375500561049));
#19859=CARTESIAN_POINT('',(0.00748201094464287,9.16282075454235E-19,0.0492847862753347));
#19860=CARTESIAN_POINT('',(0.00748201094464287,-0.00243105272334463,0.0491940719896204));
#19861=CARTESIAN_POINT('',(0.00605307400631544,-0.00439781569075195,0.0491033577039062));
#19862=CARTESIAN_POINT('',(0.004624137067988,-0.00636457865815926,0.0490126434181918));
#19863=CARTESIAN_POINT('',(0.00231206853399401,-0.00711581526389425,0.0489219291324776));
#19864=CARTESIAN_POINT('',(7.42525307968667E-18,-0.00786705186962924,0.0488312148467633));
#19865=CARTESIAN_POINT('',(-0.00231206853399399,-0.00711581526389425,0.048740500561049));
#19866=CARTESIAN_POINT('',(-0.00462413706798798,-0.00636457865815926,0.0486497862753347));
#19867=CARTESIAN_POINT('',(-0.00605307400631542,-0.00439781569075195,0.0485590719896204));
#19868=CARTESIAN_POINT('',(-0.00748201094464285,-0.00243105272334464,0.0484683577039061));
#19869=CARTESIAN_POINT('',(-0.00748201094464286,0.,0.0483776434181919));
#19870=CARTESIAN_POINT('',(-0.00748201094464285,0.00243105272334464,0.0482869291324776));
#19871=CARTESIAN_POINT('',(-0.00605307400631542,0.00439781569075195,0.0481962148467633));
#19872=CARTESIAN_POINT('',(-0.00462413706798799,0.00636457865815926,0.048105500561049));
#19873=CARTESIAN_POINT('',(-0.00231206853399399,0.00711581526389425,0.0480147862753347));
#19874=CARTESIAN_POINT('',(5.38728814187621E-18,0.00786705186962924,0.0479240719896205));
#19875=CARTESIAN_POINT('',(0.00231206853399401,0.00711581526389425,0.0478333577039062));
#19876=CARTESIAN_POINT('',(0.004624137067988,0.00636457865815926,0.0477426434181919));
#19877=CARTESIAN_POINT('',(0.00605307400631544,0.00439781569075195,0.0476519291324776));
#19878=CARTESIAN_POINT('',(0.00748201094464287,0.00243105272334464,0.0475612148467632));
#19879=CARTESIAN_POINT('',(0.00748201094464287,9.16282075454235E-19,0.047470500561049));
#19880=CARTESIAN_POINT('',(0.00748201094464287,-0.00243105272334463,0.0473797862753347));
#19881=CARTESIAN_POINT('',(0.00605307400631544,-0.00439781569075195,0.0472890719896204));
#19882=CARTESIAN_POINT('',(0.00530625606780677,-0.00542572239919884,0.0472416611809043));
#19883=CARTESIAN_POINT('',(0.00426197926959799,-0.00614947318729602,0.0471918228596965));
#19884=CARTESIAN_POINT('',(-0.0065,0.,0.0496249648492409));
#19885=CARTESIAN_POINT('',(-0.0065,0.00211197802551389,0.0495342505635266));
#19886=CARTESIAN_POINT('',(-0.00525861046343716,0.00382060413990108,0.0494435362778123));
#19887=CARTESIAN_POINT('',(-0.00401722092687431,0.00552923025428826,0.049352821992098));
#19888=CARTESIAN_POINT('',(-0.00200861046343716,0.0061818673559185,0.0492621077063837));
#19889=CARTESIAN_POINT('',(5.60326625583903E-18,0.00683450445754873,0.0491713934206694));
#19890=CARTESIAN_POINT('',(0.00200861046343717,0.0061818673559185,0.0490806791349552));
#19891=CARTESIAN_POINT('',(0.00401722092687432,0.00552923025428826,0.0489899648492409));
#19892=CARTESIAN_POINT('',(0.00525861046343717,0.00382060413990108,0.0488992505635266));
#19893=CARTESIAN_POINT('',(0.00650000000000001,0.00211197802551389,0.0488085362778123));
#19894=CARTESIAN_POINT('',(0.0065,7.9602041944578E-19,0.048717821992098));
#19895=CARTESIAN_POINT('',(0.00650000000000001,-0.00211197802551389,0.0486271077063837));
#19896=CARTESIAN_POINT('',(0.00525861046343717,-0.00382060413990108,0.0485363934206694));
#19897=CARTESIAN_POINT('',(0.00401722092687432,-0.00552923025428826,0.0484456791349552));
#19898=CARTESIAN_POINT('',(0.00200861046343717,-0.0061818673559185,0.0483549648492409));
#19899=CARTESIAN_POINT('',(7.16614409774116E-18,-0.00683450445754873,0.0482642505635266));
#19900=CARTESIAN_POINT('',(-0.00200861046343716,-0.0061818673559185,0.0481735362778123));
#19901=CARTESIAN_POINT('',(-0.00401722092687431,-0.00552923025428826,0.048082821992098));
#19902=CARTESIAN_POINT('',(-0.00525861046343716,-0.00382060413990108,0.0479921077063837));
#19903=CARTESIAN_POINT('',(-0.0065,-0.00211197802551389,0.0479013934206695));
#19904=CARTESIAN_POINT('',(-0.0065,0.,0.0478106791349552));
#19905=CARTESIAN_POINT('',(-0.0065,0.00211197802551389,0.0477199648492408));
#19906=CARTESIAN_POINT('',(-0.00525861046343716,0.00382060413990108,0.0476292505635266));
#19907=CARTESIAN_POINT('',(-0.00401722092687431,0.00552923025428826,0.0475385362778122));
#19908=CARTESIAN_POINT('',(-0.00200861046343716,0.0061818673559185,0.047447821992098));
#19909=CARTESIAN_POINT('',(5.38108033656515E-18,0.00683450445754873,0.0473571077063837));
#19910=CARTESIAN_POINT('',(0.00200861046343717,0.0061818673559185,0.0472663934206695));
#19911=CARTESIAN_POINT('',(0.00401722092687432,0.00552923025428826,0.0471756791349551));
#19912=CARTESIAN_POINT('',(0.00525861046343717,0.00382060413990108,0.0470849648492409));
#19913=CARTESIAN_POINT('',(0.00650000000000001,0.00211197802551389,0.0469942505635266));
#19914=CARTESIAN_POINT('',(0.0065,7.9602041944578E-19,0.0469035362778123));
#19915=CARTESIAN_POINT('',(0.00650000000000001,-0.00211197802551389,0.046812821992098));
#19916=CARTESIAN_POINT('',(0.00525861046343717,-0.00382060413990108,0.0467221077063837));
#19917=CARTESIAN_POINT('',(0.00460981208072669,-0.00471359850389472,0.0466746968976677));
#19918=CARTESIAN_POINT('',(0.00370259619470649,-0.00534235729046131,0.0466248585764598));
#19919=CARTESIAN_POINT('',(-0.00641348585396246,0.,0.0495750158837374));
#19920=CARTESIAN_POINT('',(-0.00641348585396245,0.00208386787546353,0.0494843015980231));
#19921=CARTESIAN_POINT('',(-0.00518861904903895,0.00376975240074554,0.0493935873123088));
#19922=CARTESIAN_POINT('',(-0.00396375224411544,0.00545563692602755,0.0493028730265945));
#19923=CARTESIAN_POINT('',(-0.00198187612205772,0.00609958751357779,0.0492121587408802));
#19924=CARTESIAN_POINT('',(5.6027193546276E-18,0.00674353810112803,0.0491214444551659));
#19925=CARTESIAN_POINT('',(0.00198187612205773,0.00609958751357779,0.0490307301694517));
#19926=CARTESIAN_POINT('',(0.00396375224411545,0.00545563692602755,0.0489400158837374));
#19927=CARTESIAN_POINT('',(0.00518861904903896,0.00376975240074554,0.0488493015980231));
#19928=CARTESIAN_POINT('',(0.00641348585396247,0.00208386787546353,0.0487585873123088));
#19929=CARTESIAN_POINT('',(0.00641348585396247,7.85425492243196E-19,0.0486678730265945));
#19930=CARTESIAN_POINT('',(0.00641348585396247,-0.00208386787546353,0.0485771587408802));
#19931=CARTESIAN_POINT('',(0.00518861904903896,-0.00376975240074554,0.048486444455166));
#19932=CARTESIAN_POINT('',(0.00396375224411545,-0.00545563692602755,0.0483957301694517));
#19933=CARTESIAN_POINT('',(0.00198187612205773,-0.00609958751357779,0.0483050158837374));
#19934=CARTESIAN_POINT('',(7.1433168650856E-18,-0.00674353810112803,0.0482143015980231));
#19935=CARTESIAN_POINT('',(-0.00198187612205772,-0.00609958751357779,0.0481235873123088));
#19936=CARTESIAN_POINT('',(-0.00396375224411544,-0.00545563692602755,0.0480328730265945));
#19937=CARTESIAN_POINT('',(-0.00518861904903895,-0.00376975240074554,0.0479421587408802));
#19938=CARTESIAN_POINT('',(-0.00641348585396245,-0.00208386787546353,0.047851444455166));
#19939=CARTESIAN_POINT('',(-0.00641348585396246,0.,0.0477607301694517));
#19940=CARTESIAN_POINT('',(-0.00641348585396245,0.00208386787546353,0.0476700158837374));
#19941=CARTESIAN_POINT('',(-0.00518861904903895,0.00376975240074554,0.0475793015980231));
#19942=CARTESIAN_POINT('',(-0.00396375224411544,0.00545563692602755,0.0474885873123088));
#19943=CARTESIAN_POINT('',(-0.00198187612205772,0.00609958751357779,0.0473978730265945));
#19944=CARTESIAN_POINT('',(5.38053343535374E-18,0.00674353810112803,0.0473071587408802));
#19945=CARTESIAN_POINT('',(0.00198187612205773,0.00609958751357779,0.047216444455166));
#19946=CARTESIAN_POINT('',(0.00396375224411545,0.00545563692602755,0.0471257301694517));
#19947=CARTESIAN_POINT('',(0.00518861904903896,0.00376975240074554,0.0470350158837374));
#19948=CARTESIAN_POINT('',(0.00641348585396247,0.00208386787546353,0.0469443015980231));
#19949=CARTESIAN_POINT('',(0.00641348585396247,7.85425492243196E-19,0.0468535873123088));
#19950=CARTESIAN_POINT('',(0.00641348585396247,-0.00208386787546353,0.0467628730265945));
#19951=CARTESIAN_POINT('',(0.00518861904903896,-0.00376975240074554,0.0466721587408802));
#19952=CARTESIAN_POINT('',(0.00454845608756398,-0.00465086112707498,0.0466247479321641));
#19953=CARTESIAN_POINT('',(0.00365331512579774,-0.00527125121679797,0.0465749096109563));
#19954=CARTESIAN_POINT('',(-0.00699100547232143,0.,0.0499084469908592));
#19955=CARTESIAN_POINT('',(-0.00748201094464286,0.,0.0501919291324776));
#19956=CARTESIAN_POINT('',(-0.0065,0.,0.0496249648492409));
#19957=CARTESIAN_POINT('',(-0.00748201094464286,0.,0.0501919291324776));
#19958=CARTESIAN_POINT('',(-0.00748201094464285,0.00243105272334464,0.0501012148467632));
#19959=CARTESIAN_POINT('',(-0.00605307400631542,0.00439781569075195,0.050010500561049));
#19960=CARTESIAN_POINT('',(-0.00462413706798799,0.00636457865815926,0.0499197862753347));
#19961=CARTESIAN_POINT('',(-0.00231206853399399,0.00711581526389425,0.0498290719896204));
#19962=CARTESIAN_POINT('',(5.60947406115009E-18,0.00786705186962924,0.0497383577039061));
#19963=CARTESIAN_POINT('',(0.00231206853399401,0.00711581526389425,0.0496476434181919));
#19964=CARTESIAN_POINT('',(0.004624137067988,0.00636457865815926,0.0495569291324775));
#19965=CARTESIAN_POINT('',(0.00605307400631544,0.00439781569075195,0.0494662148467633));
#19966=CARTESIAN_POINT('',(0.00748201094464287,0.00243105272334464,0.049375500561049));
#19967=CARTESIAN_POINT('',(0.00748201094464287,9.16282075454235E-19,0.0492847862753347));
#19968=CARTESIAN_POINT('',(0.00748201094464287,-0.00243105272334463,0.0491940719896204));
#19969=CARTESIAN_POINT('',(0.00605307400631544,-0.00439781569075195,0.0491033577039062));
#19970=CARTESIAN_POINT('',(0.004624137067988,-0.00636457865815926,0.0490126434181918));
#19971=CARTESIAN_POINT('',(0.00231206853399401,-0.00711581526389425,0.0489219291324776));
#19972=CARTESIAN_POINT('',(7.42525307968667E-18,-0.00786705186962924,0.0488312148467633));
#19973=CARTESIAN_POINT('',(-0.00231206853399399,-0.00711581526389425,0.048740500561049));
#19974=CARTESIAN_POINT('',(-0.00462413706798798,-0.00636457865815926,0.0486497862753347));
#19975=CARTESIAN_POINT('',(-0.00605307400631542,-0.00439781569075195,0.0485590719896204));
#19976=CARTESIAN_POINT('',(-0.00748201094464285,-0.00243105272334464,0.0484683577039061));
#19977=CARTESIAN_POINT('',(-0.00748201094464286,0.,0.0483776434181919));
#19978=CARTESIAN_POINT('',(-0.00748201094464285,0.00243105272334464,0.0482869291324776));
#19979=CARTESIAN_POINT('',(-0.00605307400631542,0.00439781569075195,0.0481962148467633));
#19980=CARTESIAN_POINT('',(-0.00462413706798799,0.00636457865815926,0.048105500561049));
#19981=CARTESIAN_POINT('',(-0.00231206853399399,0.00711581526389425,0.0480147862753347));
#19982=CARTESIAN_POINT('',(5.38728814187621E-18,0.00786705186962924,0.0479240719896205));
#19983=CARTESIAN_POINT('',(0.00231206853399401,0.00711581526389425,0.0478333577039062));
#19984=CARTESIAN_POINT('',(0.004624137067988,0.00636457865815926,0.0477426434181919));
#19985=CARTESIAN_POINT('',(0.00605307400631544,0.00439781569075195,0.0476519291324776));
#19986=CARTESIAN_POINT('',(0.00748201094464287,0.00243105272334464,0.0475612148467632));
#19987=CARTESIAN_POINT('',(0.00748201094464287,9.16282075454235E-19,0.047470500561049));
#19988=CARTESIAN_POINT('',(0.00748201094464287,-0.00243105272334463,0.0473797862753347));
#19989=CARTESIAN_POINT('',(0.00605307400631544,-0.00439781569075195,0.0472890719896204));
#19990=CARTESIAN_POINT('',(0.00530625606780689,-0.00542572239919866,0.0472416611809044));
#19991=CARTESIAN_POINT('',(0.00426197926959833,-0.00614947318729578,0.0471918228596965));
#19992=CARTESIAN_POINT('',(0.00426197926959833,-0.00614947318729578,0.0471918228596965));
#19993=CARTESIAN_POINT('',(0.00398228773215241,-0.00574591523887855,0.0469083407180782));
#19994=CARTESIAN_POINT('',(0.00370259619470649,-0.00534235729046131,0.0466248585764598));
#19995=CARTESIAN_POINT('',(0.00367795566025212,-0.00530680425362964,0.046599884093708));
#19996=CARTESIAN_POINT('',(0.00365331512579812,-0.00527125121679776,0.0465749096109563));
#19997=CARTESIAN_POINT('',(0.00365331512579852,-0.00527125121679756,0.0465749096109564));
#19998=CARTESIAN_POINT('',(0.00418300421785061,-0.00498093574494503,0.046638839317779));
#19999=CARTESIAN_POINT('',(0.00509595215042321,-0.00414814728430873,0.0466991834499751));
#20000=CARTESIAN_POINT('',(0.00573004291196533,-0.00312785079813037,0.0467584423785249));
#20001=CARTESIAN_POINT('',(0.00596966594774492,-0.00257159259454815,0.04678567913));
#20002=CARTESIAN_POINT('',(0.00596966594774489,-0.00257159259454823,0.04678567913));
#20003=CARTESIAN_POINT('',(-1.22293354860711E-5,3.97877174541167E-6,0.0468128222162991));
#20004=CARTESIAN_POINT('',(0.0065,7.9602041944578E-19,0.0469035362778123));
#20005=CARTESIAN_POINT('',(-0.0065,0.,0.0478106791349552));
#20006=CARTESIAN_POINT('',(-0.00650000000000001,0.00211197802551388,0.0477199648492409));
#20007=CARTESIAN_POINT('',(-0.00525861046343716,0.00382060413990108,0.0476292505635266));
#20008=CARTESIAN_POINT('',(-0.00401722092687431,0.00552923025428826,0.0475385362778122));
#20009=CARTESIAN_POINT('',(-0.00200861046343716,0.0061818673559185,0.047447821992098));
#20010=CARTESIAN_POINT('',(5.38108033656515E-18,0.00683450445754873,0.0473571077063837));
#20011=CARTESIAN_POINT('',(0.00200861046343717,0.0061818673559185,0.0472663934206695));
#20012=CARTESIAN_POINT('',(0.00401722092687432,0.00552923025428826,0.0471756791349551));
#20013=CARTESIAN_POINT('',(0.00525861046343717,0.00382060413990108,0.0470849648492409));
#20014=CARTESIAN_POINT('',(0.00649999999999998,0.00211197802551393,0.0469942505635266));
#20015=CARTESIAN_POINT('',(0.0065,7.96020419445779E-19,0.0469035362778123));
#20016=CARTESIAN_POINT('',(-0.0065,0.,0.0478106791349552));
#20017=CARTESIAN_POINT('',(0.0065,7.96020419445781E-19,0.0487178219920981));
#20018=CARTESIAN_POINT('',(0.00650000000000003,-0.00211197802551387,0.0486271077063837));
#20019=CARTESIAN_POINT('',(0.00525861046343717,-0.00382060413990108,0.0485363934206694));
#20020=CARTESIAN_POINT('',(0.00401722092687432,-0.00552923025428826,0.0484456791349552));
#20021=CARTESIAN_POINT('',(0.00200861046343717,-0.0061818673559185,0.0483549648492409));
#20022=CARTESIAN_POINT('',(7.16614409774116E-18,-0.00683450445754873,0.0482642505635266));
#20023=CARTESIAN_POINT('',(-0.00200861046343716,-0.0061818673559185,0.0481735362778123));
#20024=CARTESIAN_POINT('',(-0.00401722092687431,-0.00552923025428826,0.048082821992098));
#20025=CARTESIAN_POINT('',(-0.00525861046343716,-0.00382060413990108,0.0479921077063837));
#20026=CARTESIAN_POINT('',(-0.00649999999999999,-0.00211197802551391,0.0479013934206695));
#20027=CARTESIAN_POINT('',(-0.0065,0.,0.0478106791349552));
#20028=CARTESIAN_POINT('',(0.0065,7.9602041944578E-19,0.048717821992098));
#20029=CARTESIAN_POINT('',(-0.0065,0.,0.0496249648492409));
#20030=CARTESIAN_POINT('',(-0.0065,0.00211197802551389,0.0495342505635266));
#20031=CARTESIAN_POINT('',(-0.00525861046343716,0.00382060413990108,0.0494435362778123));
#20032=CARTESIAN_POINT('',(-0.00401722092687431,0.00552923025428826,0.049352821992098));
#20033=CARTESIAN_POINT('',(-0.00200861046343716,0.0061818673559185,0.0492621077063837));
#20034=CARTESIAN_POINT('',(5.60326625583903E-18,0.00683450445754873,0.0491713934206694));
#20035=CARTESIAN_POINT('',(0.00200861046343717,0.0061818673559185,0.0490806791349552));
#20036=CARTESIAN_POINT('',(0.00401722092687432,0.00552923025428826,0.0489899648492409));
#20037=CARTESIAN_POINT('',(0.00525861046343717,0.00382060413990108,0.0488992505635266));
#20038=CARTESIAN_POINT('',(0.0065,0.00211197802551392,0.0488085362778123));
#20039=CARTESIAN_POINT('',(0.0065,7.9602041944578E-19,0.048717821992098));
#20040=CARTESIAN_POINT('',(-0.0065,0.,0.05098567913));
#20041=CARTESIAN_POINT('',(-0.0065,0.00139216394854201,0.0509258825049104));
#20042=CARTESIAN_POINT('',(-0.00601209861219997,0.00283854168444359,0.0508578508580355));
#20043=CARTESIAN_POINT('',(-0.00473881207941318,0.00450353441535566,0.0507671294297172));
#20044=CARTESIAN_POINT('',(-0.00421228132056244,0.00500154670113435,0.0507346711453865));
#20045=CARTESIAN_POINT('',(-0.0030273902334642,0.00579600653049259,0.0506702885995784));
#20046=CARTESIAN_POINT('',(-0.00237885749509726,0.00608954574355769,0.0506395433453287));
#20047=CARTESIAN_POINT('',(-0.00102560939713424,0.00645675272171483,0.050578426998065));
#20048=CARTESIAN_POINT('',(-0.00030367301496546,0.0065319158651834,0.0505458223968087));
#20049=CARTESIAN_POINT('',(0.00111920072308763,0.00644247870864103,0.0504815615671662));
#20050=CARTESIAN_POINT('',(0.00180859004388786,0.00628280413851949,0.0504513811063915));
#20051=CARTESIAN_POINT('',(0.00311059239441925,0.00575055134275219,0.0503896801606666));
#20052=CARTESIAN_POINT('',(0.00373007126500205,0.00537063786359636,0.0503569608419805));
#20053=CARTESIAN_POINT('',(0.0048044795422359,0.00443555622578788,0.0502928821077617));
#20054=CARTESIAN_POINT('',(0.00525317896866053,0.00389249931724978,0.0502631287087374));
#20055=CARTESIAN_POINT('',(0.0059658150773882,0.00267516180332607,0.050200895697937));
#20056=CARTESIAN_POINT('',(0.00622663675302494,0.00199622202754049,0.0501680936432468));
#20057=CARTESIAN_POINT('',(0.00651099344925417,0.000602388530043543,0.05010425681266));
#20058=CARTESIAN_POINT('',(0.00653759021180571,-9.93993057869834E-5,0.0500747914560228));
#20059=CARTESIAN_POINT('',(0.00636330161511123,-0.00150278360205708,0.0500120805120238));
#20060=CARTESIAN_POINT('',(0.00615721630509946,-0.00220068351354411,0.0499792279792733));
#20061=CARTESIAN_POINT('',(0.00553676033670485,-0.00347830497921899,0.0499156921049825));
#20062=CARTESIAN_POINT('',(0.00513232728730257,-0.00405110020501809,0.0498863749004916));
#20063=CARTESIAN_POINT('',(0.0041387911019502,-0.00506187756366211,0.049823241605466));
#20064=CARTESIAN_POINT('',(0.00355057709646319,-0.00549052166700355,0.0497903710217429));
#20065=CARTESIAN_POINT('',(0.00228372268767734,-0.00612674763472041,0.0497271942213094));
#20066=CARTESIAN_POINT('',(0.00161460618063539,-0.00633617958351373,0.0496978848300432));
#20067=CARTESIAN_POINT('',(0.000208606071525814,-0.0065353353655344,0.0496343860591597));
#20068=CARTESIAN_POINT('',(-0.000518900078309723,-0.00651774283233561,0.0496015299121185));
#20069=CARTESIAN_POINT('',(-0.00190855809191155,-0.00625360975193776,0.0495387691945051));
#20070=CARTESIAN_POINT('',(-0.00256826845705628,-0.00601329722457722,0.0495093272538655));
#20071=CARTESIAN_POINT('',(-0.00380776289581589,-0.00531570203339748,0.0494455210097757));
#20072=CARTESIAN_POINT('',(-0.00437421795963069,-0.0048594189913196,0.049412711738628));
#20073=CARTESIAN_POINT('',(-0.00531494605788761,-0.0038077662865909,0.0493504228378307));
#20074=CARTESIAN_POINT('',(-0.00569422021225458,-0.00321448480076881,0.0493207083866951));
#20075=CARTESIAN_POINT('',(-0.00625510978961098,-0.00190542852921204,0.0492566536267806));
#20076=CARTESIAN_POINT('',(-0.00642702787888753,-0.00119927714474249,0.0492239235136309));
#20077=CARTESIAN_POINT('',(-0.0065347900081369,0.000203648165848476,0.0491621607304204));
#20078=CARTESIAN_POINT('',(-0.00647555925786837,0.00090839605602264,0.0491320346317823));
#20079=CARTESIAN_POINT('',(-0.00594944360627666,0.00298099398905514,0.049035669317932));
#20080=CARTESIAN_POINT('',(-0.00514941531216868,0.00421526192212428,0.0489754985627794));
#20081=CARTESIAN_POINT('',(-0.00291101632274778,0.00598422050880514,0.048846754562263));
#20082=CARTESIAN_POINT('',(-0.00152663083830425,0.00647732477884384,0.0487867687682968));
#20083=CARTESIAN_POINT('',(0.00132703907897548,0.00652114294353052,0.0486578893101228));
#20084=CARTESIAN_POINT('',(0.00272549909433502,0.00607109015430752,0.0485979737679985));
#20085=CARTESIAN_POINT('',(0.00501803035286572,0.0043710241766283,0.048469080736597));
#20086=CARTESIAN_POINT('',(0.00585487210850577,0.00316319651939615,0.0484091205156593));
#20087=CARTESIAN_POINT('',(0.00664142800919386,0.00042044455755067,0.0482803358382475));
#20088=CARTESIAN_POINT('',(0.00657143556203462,-0.00104840443285802,0.0482202161486085));
#20089=CARTESIAN_POINT('',(0.00578979634639851,-0.00303915902305769,0.0481238000953949));
#20090=CARTESIAN_POINT('',(0.00542633082347876,-0.00364681078028188,0.0480935635664421));
#20091=CARTESIAN_POINT('',(0.00474737139188325,-0.00445376679180473,0.0480473347232857));
#20092=CARTESIAN_POINT('',(0.00449681825450261,-0.00470696398512329,0.0480314587978482));
#20093=CARTESIAN_POINT('',(0.00395553899020957,-0.00517016398852178,0.0479993857674241));
#20094=CARTESIAN_POINT('',(0.00366004488627924,-0.00537184808729585,0.0479832352812528));
#20095=CARTESIAN_POINT('',(0.00336685009946227,-0.00557505095485768,0.0479671284889492));
#20096=CARTESIAN_POINT('',(-0.00682733698154762,0.,0.0507966910355878));
#20097=CARTESIAN_POINT('',(-0.00682733698154762,0.00146227267850127,0.0507368944104981));
#20098=CARTESIAN_POINT('',(-0.0063148651064283,0.00298148932551787,0.0506688627636233));
#20099=CARTESIAN_POINT('',(-0.00497745645513572,0.00473033031717387,0.0505781413353049));
#20100=CARTESIAN_POINT('',(-0.00442440985177819,0.00525342227039878,0.0505456830509742));
#20101=CARTESIAN_POINT('',(-0.00317984819977019,0.00608789072783439,0.0504813005051662));
#20102=CARTESIAN_POINT('',(-0.00249865565386296,0.00639621243935651,0.0504505552509165));
#20103=CARTESIAN_POINT('',(-0.00107725861010421,0.00678191179041106,0.0503894389036528));
#20104=CARTESIAN_POINT('',(-0.000318965846980269,0.00686086011488066,0.0503568343023965));
#20105=CARTESIAN_POINT('',(0.00117556315177092,0.0067669189446674,0.0502925734727539));
#20106=CARTESIAN_POINT('',(0.00189966979862991,0.00659920323734378,0.0502623930119793));
#20107=CARTESIAN_POINT('',(0.00326724038291374,0.00604014643794775,0.0502006920662544));
#20108=CARTESIAN_POINT('',(0.00391791592174717,0.00564110069240482,0.0501679727475682));
#20109=CARTESIAN_POINT('',(0.00504643090089172,0.00465892877754698,0.0501038940133495));
#20110=CARTESIAN_POINT('',(0.00551772662206526,0.00408852377527819,0.0500741406143251));
#20111=CARTESIAN_POINT('',(0.00626625075429644,0.00280988170945719,0.0500119076035247));
#20112=CARTESIAN_POINT('',(0.00654020728839858,0.00209675084184725,0.0499791055488345));
#20113=CARTESIAN_POINT('',(0.00683888405580113,0.000632724536680984,0.0499152687182477));
#20114=CARTESIAN_POINT('',(0.00686682021896383,-0.000104405008667636,0.0498858033616105));
#20115=CARTESIAN_POINT('',(0.00668375452947548,-0.0015784630863981,0.0498230924176116));
#20116=CARTESIAN_POINT('',(0.00646729085895286,-0.00231150891333874,0.049790239884861));
#20117=CARTESIAN_POINT('',(0.00581558901611555,-0.00365347080272662,0.0497267040105703));
#20118=CARTESIAN_POINT('',(0.00539078890615489,-0.00425511173010386,0.0496973868060793));
#20119=CARTESIAN_POINT('',(0.00434721869988382,-0.00531679136714716,0.0496342535110538));
#20120=CARTESIAN_POINT('',(0.00372938251023371,-0.00576702178848028,0.0496013829273307));
#20121=CARTESIAN_POINT('',(0.00239872990171982,-0.00643528780048248,0.0495382061268972));
#20122=CARTESIAN_POINT('',(0.00169591699810574,-0.00665526664496158,0.049508896735631));
#20123=CARTESIAN_POINT('',(0.000219111376415932,-0.00686445181968139,0.0494453979647474));
#20124=CARTESIAN_POINT('',(-0.000545031645287988,-0.00684597333468028,0.0494125418177063));
#20125=CARTESIAN_POINT('',(-0.00200467219112918,-0.006568538635011,0.0493497811000929));
#20126=CARTESIAN_POINT('',(-0.00269760526390808,-0.00631612408036826,0.0493203391594533));
#20127=CARTESIAN_POINT('',(-0.00399952006701057,-0.00558339831930807,0.0492565329153635));
#20128=CARTESIAN_POINT('',(-0.00459450154479021,-0.00510413707511864,0.0492237236442158));
#20129=CARTESIAN_POINT('',(-0.00558260427322259,-0.00399952362854343,0.0491614347434185));
#20130=CARTESIAN_POINT('',(-0.00598097849787717,-0.00337636476260179,0.0491317202922829));
#20131=CARTESIAN_POINT('',(-0.00657011421388486,-0.00200138502510542,0.0490676655323683));
#20132=CARTESIAN_POINT('',(-0.00675069001830252,-0.00125967218483466,0.0490349354192187));
#20133=CARTESIAN_POINT('',(-0.0068638789983386,0.000213903792911022,0.0489731726360082));
#20134=CARTESIAN_POINT('',(-0.00680166541499197,0.000954142459565442,0.04894304653737));
#20135=CARTESIAN_POINT('',(-0.00624905482350225,0.00313111546203805,0.0488466812235198));
#20136=CARTESIAN_POINT('',(-0.00540873747601797,0.00442754055505055,0.0487865104683671));
#20137=CARTESIAN_POINT('',(-0.00305761375295149,0.00628558307469247,0.0486577664678508));
#20138=CARTESIAN_POINT('',(-0.00160351125838856,0.00680351984678389,0.0485977806738846));
#20139=CARTESIAN_POINT('',(0.00139386815074587,0.00684954467389603,0.0484689012157106));
#20140=CARTESIAN_POINT('',(0.00286275396306585,0.00637682743520206,0.0484089856735863));
#20141=CARTESIAN_POINT('',(0.00527073603117671,0.00459114692435894,0.0482800926421847));
#20142=CARTESIAN_POINT('',(0.00614972074902048,0.00332249362719632,0.048220132421247));
#20143=CARTESIAN_POINT('',(0.00697588723960853,0.000441617950224018,0.0480913477438352));
#20144=CARTESIAN_POINT('',(0.00690237000531325,-0.00110120159324154,0.0480312280541963));
#20145=CARTESIAN_POINT('',(0.0060813678017532,-0.00319220966014245,0.0479348120009826));
#20146=CARTESIAN_POINT('',(0.00569959832388436,-0.00383046247768077,0.0479045754720299));
#20147=CARTESIAN_POINT('',(0.00498644681060703,-0.00467805641921186,0.0478583466288735));
#20148=CARTESIAN_POINT('',(0.00472327593357909,-0.00494400450560692,0.047842470703436));
#20149=CARTESIAN_POINT('',(0.00415473809689405,-0.005430531046077,0.0478103976730118));
#20150=CARTESIAN_POINT('',(0.00384436304711054,-0.00564237186240781,0.0477942471868405));
#20151=CARTESIAN_POINT('',(0.00353640310698247,-0.00585580793201727,0.047778140394537));
#20152=CARTESIAN_POINT('',(-0.00715467396309524,0.,0.0506077029411755));
#20153=CARTESIAN_POINT('',(-0.00715467396309523,0.00153238140846052,0.0505479063160859));
#20154=CARTESIAN_POINT('',(-0.00661763160065663,0.00312443696659216,0.0504798746692111));
#20155=CARTESIAN_POINT('',(-0.00521610083085826,0.00495712621899208,0.0503891532408927));
#20156=CARTESIAN_POINT('',(-0.00463653838299393,0.0055052978396632,0.050356694956562));
#20157=CARTESIAN_POINT('',(-0.00333230616607618,0.0063797749251762,0.0502923124107539));
#20158=CARTESIAN_POINT('',(-0.00261845381262866,0.00670287913515533,0.0502615671565042));
#20159=CARTESIAN_POINT('',(-0.00112890782307418,0.0071070708591073,0.0502004508092405));
#20160=CARTESIAN_POINT('',(-0.000334258678995079,0.00718980436457791,0.0501678462079842));
#20161=CARTESIAN_POINT('',(0.00123192558045422,0.00709135918069376,0.0501035853783417));
#20162=CARTESIAN_POINT('',(0.00199074955337196,0.00691560233616806,0.050073404917567));
#20163=CARTESIAN_POINT('',(0.00342388837140823,0.0063297415331433,0.0500117039718421));
#20164=CARTESIAN_POINT('',(0.00410576057849229,0.00591156352121328,0.049978984653156));
#20165=CARTESIAN_POINT('',(0.00528838225954753,0.00488230132930608,0.0499149059189373));
#20166=CARTESIAN_POINT('',(0.00578227427547,0.00428454823330661,0.0498851525199129));
#20167=CARTESIAN_POINT('',(0.00656668643120468,0.0029446016155883,0.0498229195091125));
#20168=CARTESIAN_POINT('',(0.00685377782377222,0.00219727965615402,0.0497901174544223));
#20169=CARTESIAN_POINT('',(0.00716677466234808,0.000663060543318424,0.0497262806238355));
#20170=CARTESIAN_POINT('',(0.00719605022612195,-0.000109410711548288,0.0496968152671983));
#20171=CARTESIAN_POINT('',(0.00700420744383973,-0.00165414257073912,0.0496341043231993));
#20172=CARTESIAN_POINT('',(0.00677736541280625,-0.00242233431313338,0.0496012517904488));
#20173=CARTESIAN_POINT('',(0.00609441769552624,-0.00382863662623425,0.049537715916158));
#20174=CARTESIAN_POINT('',(0.00564925052500722,-0.00445912325518964,0.0495083987116671));
#20175=CARTESIAN_POINT('',(0.00455564629781744,-0.0055717051706322,0.0494452654166416));
#20176=CARTESIAN_POINT('',(0.00390818792400423,-0.00604352190995701,0.0494123948329184));
#20177=CARTESIAN_POINT('',(0.0025137371157623,-0.00674382796624454,0.0493492180324849));
#20178=CARTESIAN_POINT('',(0.0017772278155761,-0.00697435370640943,0.0493199086412188));
#20179=CARTESIAN_POINT('',(0.00022961668130605,-0.00719356827382838,0.0492564098703352));
#20180=CARTESIAN_POINT('',(-0.000571163212266254,-0.00717420383702495,0.049223553723294));
#20181=CARTESIAN_POINT('',(-0.00210078629034681,-0.00688346751808424,0.0491607930056807));
#20182=CARTESIAN_POINT('',(-0.00282694207075989,-0.0066189509361593,0.049131351065041));
#20183=CARTESIAN_POINT('',(-0.00419127723820524,-0.00585109460521867,0.0490675448209512));
#20184=CARTESIAN_POINT('',(-0.00481478512994973,-0.00534885515891767,0.0490347355498035));
#20185=CARTESIAN_POINT('',(-0.00585026248855756,-0.00419128097049597,0.0489724466490063));
#20186=CARTESIAN_POINT('',(-0.00626773678349976,-0.00353824472443477,0.0489427321978707));
#20187=CARTESIAN_POINT('',(-0.00688511863815874,-0.00209734152099881,0.0488786774379561));
#20188=CARTESIAN_POINT('',(-0.00707435215771751,-0.00132006722492682,0.0488459473248065));
#20189=CARTESIAN_POINT('',(-0.00719296798854031,0.000224159419973568,0.048784184541596));
#20190=CARTESIAN_POINT('',(-0.00712777157211556,0.000999888863108244,0.0487540584429578));
#20191=CARTESIAN_POINT('',(-0.00654866604072785,0.00328123693502096,0.0486576931291076));
#20192=CARTESIAN_POINT('',(-0.00566805963986726,0.00463981918797682,0.0485975223739549));
#20193=CARTESIAN_POINT('',(-0.0032042111831552,0.0065869456405798,0.0484687783734385));
#20194=CARTESIAN_POINT('',(-0.00168039167847287,0.00712971491472395,0.0484087925794723));
#20195=CARTESIAN_POINT('',(0.00146069722251627,0.00717794640426154,0.0482799131212984));
#20196=CARTESIAN_POINT('',(0.00300000883179668,0.0066825647160966,0.0482199975791741));
#20197=CARTESIAN_POINT('',(0.00552344170948769,0.00481126967208959,0.0480911045477725));
#20198=CARTESIAN_POINT('',(0.0064445693895352,0.00348179073499648,0.0480311443268348));
#20199=CARTESIAN_POINT('',(0.0073103464700232,0.000462791342897367,0.047902359649423));
#20200=CARTESIAN_POINT('',(0.00723330444859188,-0.00115399875362506,0.0478422399597841));
#20201=CARTESIAN_POINT('',(0.0063729392571079,-0.0033452602972272,0.0477458239065704));
#20202=CARTESIAN_POINT('',(0.00597286582428995,-0.00401411417507966,0.0477155873776177));
#20203=CARTESIAN_POINT('',(0.00522552222933081,-0.004902346046619,0.0476693585344612));
#20204=CARTESIAN_POINT('',(0.00494973361265557,-0.00518104502609055,0.0476534826090237));
#20205=CARTESIAN_POINT('',(0.00435393720357852,-0.00569089810363222,0.0476214095785996));
#20206=CARTESIAN_POINT('',(0.00402868120794183,-0.00591289563751978,0.0476052590924282));
#20207=CARTESIAN_POINT('',(0.00370595611450266,-0.00613656490917685,0.0475891523001247));
#20208=CARTESIAN_POINT('',(-0.00748201094464286,0.,0.0504187148467633));
#20209=CARTESIAN_POINT('',(-0.00748201094464285,0.00160249013841978,0.0503589182216737));
#20210=CARTESIAN_POINT('',(-0.00692039809488496,0.00326738460766644,0.0502908865747988));
#20211=CARTESIAN_POINT('',(-0.00545474520658079,0.00518392212081029,0.0502001651464805));
#20212=CARTESIAN_POINT('',(-0.00484866691420967,0.00575717340892763,0.0501677068621498));
#20213=CARTESIAN_POINT('',(-0.00348476413238216,0.00667165912251801,0.0501033243163417));
#20214=CARTESIAN_POINT('',(-0.00273825197139437,0.00700954583095415,0.050072579062092));
#20215=CARTESIAN_POINT('',(-0.00118055703604415,0.00743222992780353,0.0500114627148283));
#20216=CARTESIAN_POINT('',(-0.000349551511009888,0.00751874861427516,0.049978858113572));
#20217=CARTESIAN_POINT('',(0.00128828800913751,0.00741579941672012,0.0499145972839295));
#20218=CARTESIAN_POINT('',(0.00208182930811401,0.00723200143499235,0.0498844168231548));
#20219=CARTESIAN_POINT('',(0.00358053635990272,0.00661933662833886,0.0498227158774299));
#20220=CARTESIAN_POINT('',(0.00429360523523741,0.00618202635002174,0.0497899965587437));
#20221=CARTESIAN_POINT('',(0.00553033361820334,0.00510567388106518,0.049725917824525));
#20222=CARTESIAN_POINT('',(0.00604682192887473,0.00448057269133503,0.0496961644255007));
#20223=CARTESIAN_POINT('',(0.00686712210811291,0.00307932152171942,0.0496339314147002));
#20224=CARTESIAN_POINT('',(0.00716734835914586,0.00229780847046079,0.04960112936001));
#20225=CARTESIAN_POINT('',(0.00749466526889503,0.000693396549955864,0.0495372925294232));
#20226=CARTESIAN_POINT('',(0.00752528023328007,-0.00011441641442894,0.049507827172786));
#20227=CARTESIAN_POINT('',(0.00732466035820398,-0.00172982205508014,0.0494451162287871));
#20228=CARTESIAN_POINT('',(0.00708743996665964,-0.00253315971292801,0.0494122636960365));
#20229=CARTESIAN_POINT('',(0.00637324637493694,-0.00400380244974188,0.0493487278217458));
#20230=CARTESIAN_POINT('',(0.00590771214385954,-0.00466313478027542,0.0493194106172549));
#20231=CARTESIAN_POINT('',(0.00476407389575106,-0.00582661897411724,0.0492562773222293));
#20232=CARTESIAN_POINT('',(0.00408699333777475,-0.00632002203143374,0.0492234067385062));
#20233=CARTESIAN_POINT('',(0.00262874432980478,-0.0070523681320066,0.0491602299380727));
#20234=CARTESIAN_POINT('',(0.00185853863304645,-0.00729344076785728,0.0491309205468065));
#20235=CARTESIAN_POINT('',(0.000240121986196168,-0.00752268472797537,0.049067421775923));
#20236=CARTESIAN_POINT('',(-0.000597294779244519,-0.00750243433936963,0.0490345656288818));
#20237=CARTESIAN_POINT('',(-0.00219690038956444,-0.00719839640115748,0.0489718049112684));
#20238=CARTESIAN_POINT('',(-0.0029562788776117,-0.00692177779195035,0.0489423629706288));
#20239=CARTESIAN_POINT('',(-0.00438303440939992,-0.00611879089112926,0.048878556726539));
#20240=CARTESIAN_POINT('',(-0.00503506871510925,-0.00559357324271671,0.0488457474553913));
#20241=CARTESIAN_POINT('',(-0.00611792070389254,-0.0043830383124485,0.048783458554594));
#20242=CARTESIAN_POINT('',(-0.00655449506912235,-0.00370012468626775,0.0487537441034584));
#20243=CARTESIAN_POINT('',(-0.00720012306243262,-0.00219329801689219,0.0486896893435438));
#20244=CARTESIAN_POINT('',(-0.0073980142971325,-0.00138046226501898,0.0486569592303942));
#20245=CARTESIAN_POINT('',(-0.00752205697874201,0.000234415047036114,0.0485951964471837));
#20246=CARTESIAN_POINT('',(-0.00745387772923916,0.00104563526665105,0.0485650703485456));
#20247=CARTESIAN_POINT('',(-0.00684827725795344,0.00343135840800387,0.0484687050346953));
#20248=CARTESIAN_POINT('',(-0.00592738180371655,0.0048520978209031,0.0484085342795426));
#20249=CARTESIAN_POINT('',(-0.00335080861335891,0.00688830820646713,0.0482797902790263));
#20250=CARTESIAN_POINT('',(-0.00175727209855718,0.007455909982664,0.0482198044850601));
#20251=CARTESIAN_POINT('',(0.00152752629428666,0.00750634813462706,0.0480909250268861));
#20252=CARTESIAN_POINT('',(0.00313726370052751,0.00698830199699114,0.0480310094847618));
#20253=CARTESIAN_POINT('',(0.00577614738779868,0.00503139241982023,0.0479021164533603));
#20254=CARTESIAN_POINT('',(0.00673941803004991,0.00364108784279665,0.0478421562324226));
#20255=CARTESIAN_POINT('',(0.00764480570043787,0.000483964735570715,0.0477133715550107));
#20256=CARTESIAN_POINT('',(0.00756423889187051,-0.00120679591400858,0.0476532518653718));
#20257=CARTESIAN_POINT('',(0.0066645107124626,-0.00349831093431196,0.0475568358121581));
#20258=CARTESIAN_POINT('',(0.00624613332469554,-0.00419776587247855,0.0475265992832054));
#20259=CARTESIAN_POINT('',(0.00546459764805459,-0.00512663567402613,0.047480370440049));
#20260=CARTESIAN_POINT('',(0.00517619129173205,-0.00541808554657418,0.0474644945146114));
#20261=CARTESIAN_POINT('',(0.004553136310263,-0.00595126516118744,0.0474324214841873));
#20262=CARTESIAN_POINT('',(0.00421299936877313,-0.00618341941263174,0.047416270998016));
#20263=CARTESIAN_POINT('',(0.00387550912202286,-0.00641732188633643,0.0474001642057124));
#20264=CARTESIAN_POINT('',(-0.00699100547232143,0.,0.0507021969883817));
#20265=CARTESIAN_POINT('',(-0.0065,0.,0.05098567913));
#20266=CARTESIAN_POINT('',(-0.00748201094464286,0.,0.0504187148467633));
#20267=CARTESIAN_POINT('',(-0.0065,0.,0.05098567913));
#20268=CARTESIAN_POINT('',(-0.0065,0.00211197802551389,0.0508949648442857));
#20269=CARTESIAN_POINT('',(-0.00525861046343716,0.00382060413990108,0.0508042505585714));
#20270=CARTESIAN_POINT('',(-0.00401722092687431,0.00552923025428826,0.0507135362728571));
#20271=CARTESIAN_POINT('',(-0.00200861046343716,0.0061818673559185,0.0506228219871429));
#20272=CARTESIAN_POINT('',(5.7699056946876E-18,0.00683450445754873,0.0505321077014286));
#20273=CARTESIAN_POINT('',(0.00200861046343717,0.0061818673559185,0.0504413934157143));
#20274=CARTESIAN_POINT('',(0.00401722092687432,0.00552923025428826,0.05035067913));
#20275=CARTESIAN_POINT('',(0.00525861046343717,0.00382060413990108,0.0502599648442857));
#20276=CARTESIAN_POINT('',(0.0065,0.00211197802551392,0.0501692505585715));
#20277=CARTESIAN_POINT('',(0.0065,7.9602041944578E-19,0.0500785362728571));
#20278=CARTESIAN_POINT('',(0.0065,7.9602041944578E-19,0.0500785362728572));
#20279=CARTESIAN_POINT('',(0.0065,7.96020419445781E-19,0.0500785362728572));
#20280=CARTESIAN_POINT('',(0.00650000000000003,-0.00211197802551387,0.0499878219871428));
#20281=CARTESIAN_POINT('',(0.00525861046343717,-0.00382060413990108,0.0498971077014286));
#20282=CARTESIAN_POINT('',(0.00401722092687432,-0.00552923025428826,0.0498063934157143));
#20283=CARTESIAN_POINT('',(0.00200861046343717,-0.0061818673559185,0.04971567913));
#20284=CARTESIAN_POINT('',(7.33278353658974E-18,-0.00683450445754873,0.0496249648442857));
#20285=CARTESIAN_POINT('',(-0.00200861046343716,-0.0061818673559185,0.0495342505585714));
#20286=CARTESIAN_POINT('',(-0.00401722092687431,-0.00552923025428826,0.0494435362728571));
#20287=CARTESIAN_POINT('',(-0.00525861046343716,-0.00382060413990108,0.0493528219871429));
#20288=CARTESIAN_POINT('',(-0.00649999999999999,-0.00211197802551391,0.0492621077014285));
#20289=CARTESIAN_POINT('',(-0.0065,0.,0.0491713934157143));
#20290=CARTESIAN_POINT('',(-0.0065,0.,0.0491713934157143));
#20291=CARTESIAN_POINT('',(-0.0065,0.,0.0491713934157143));
#20292=CARTESIAN_POINT('',(-0.00650000000000001,0.00211197802551388,0.04908067913));
#20293=CARTESIAN_POINT('',(-0.00525861046343716,0.00382060413990108,0.0489899648442857));
#20294=CARTESIAN_POINT('',(-0.00401722092687431,0.00552923025428826,0.0488992505585714));
#20295=CARTESIAN_POINT('',(-0.00200861046343716,0.0061818673559185,0.0488085362728572));
#20296=CARTESIAN_POINT('',(5.54771977541372E-18,0.00683450445754873,0.0487178219871428));
#20297=CARTESIAN_POINT('',(0.00200861046343717,0.0061818673559185,0.0486271077014286));
#20298=CARTESIAN_POINT('',(0.00401722092687432,0.00552923025428826,0.0485363934157143));
#20299=CARTESIAN_POINT('',(0.00525861046343717,0.00382060413990108,0.04844567913));
#20300=CARTESIAN_POINT('',(0.00649999999999998,0.00211197802551393,0.0483549648442856));
#20301=CARTESIAN_POINT('',(0.0065,7.96020419445779E-19,0.0482642505585714));
#20302=CARTESIAN_POINT('',(0.0065,7.9602041944578E-19,0.0482642505585714));
#20303=CARTESIAN_POINT('',(0.0065,7.96020419445781E-19,0.0482642505585715));
#20304=CARTESIAN_POINT('',(0.00650000000000004,-0.00211197802551386,0.0481735362728571));
#20305=CARTESIAN_POINT('',(0.00525861046343717,-0.00382060413990108,0.0480828219871429));
#20306=CARTESIAN_POINT('',(0.00460981098571225,-0.0047136000110528,0.0480354110984088));
#20307=CARTESIAN_POINT('',(0.00370259321821895,-0.00534235935335683,0.0479855726937042));
#20308=CARTESIAN_POINT('',(0.00370259421038123,-0.00534235866572474,0.0479855727658843));
#20309=CARTESIAN_POINT('',(0.00398228679950131,-0.00574591588526488,0.047702090660359));
#20310=CARTESIAN_POINT('',(0.00426198038078367,-0.00614947241717293,0.0474186086270138));
#20311=CARTESIAN_POINT('',(-0.00748201094464286,0.,0.0504187148467633));
#20312=CARTESIAN_POINT('',(-0.00748201094464285,0.00243105272334464,0.050328000561049));
#20313=CARTESIAN_POINT('',(-0.00605307400631542,0.00439781569075195,0.0502372862753347));
#20314=CARTESIAN_POINT('',(-0.00462413706798799,0.00636457865815926,0.0501465719896204));
#20315=CARTESIAN_POINT('',(-0.00231206853399399,0.00711581526389425,0.0500558577039062));
#20316=CARTESIAN_POINT('',(5.63724730105931E-18,0.00786705186962924,0.0499651434181919));
#20317=CARTESIAN_POINT('',(0.00231206853399401,0.00711581526389425,0.0498744291324776));
#20318=CARTESIAN_POINT('',(0.004624137067988,0.00636457865815926,0.0497837148467633));
#20319=CARTESIAN_POINT('',(0.00605307400631544,0.00439781569075195,0.049693000561049));
#20320=CARTESIAN_POINT('',(0.00748201094464287,0.00243105272334464,0.0496022862753347));
#20321=CARTESIAN_POINT('',(0.00748201094464287,9.16282075454235E-19,0.0495115719896204));
#20322=CARTESIAN_POINT('',(0.00748201094464287,-0.00243105272334463,0.0494208577039061));
#20323=CARTESIAN_POINT('',(0.00605307400631544,-0.00439781569075195,0.0493301434181919));
#20324=CARTESIAN_POINT('',(0.004624137067988,-0.00636457865815926,0.0492394291324775));
#20325=CARTESIAN_POINT('',(0.00231206853399401,-0.00711581526389425,0.0491487148467633));
#20326=CARTESIAN_POINT('',(7.45302631959591E-18,-0.00786705186962924,0.049058000561049));
#20327=CARTESIAN_POINT('',(-0.00231206853399399,-0.00711581526389425,0.0489672862753347));
#20328=CARTESIAN_POINT('',(-0.00462413706798798,-0.00636457865815926,0.0488765719896204));
#20329=CARTESIAN_POINT('',(-0.00605307400631542,-0.00439781569075195,0.0487858577039062));
#20330=CARTESIAN_POINT('',(-0.00748201094464285,-0.00243105272334464,0.0486951434181918));
#20331=CARTESIAN_POINT('',(-0.00748201094464286,0.,0.0486044291324776));
#20332=CARTESIAN_POINT('',(-0.00748201094464285,0.00243105272334464,0.0485137148467633));
#20333=CARTESIAN_POINT('',(-0.00605307400631542,0.00439781569075195,0.048423000561049));
#20334=CARTESIAN_POINT('',(-0.00462413706798799,0.00636457865815926,0.0483322862753347));
#20335=CARTESIAN_POINT('',(-0.00231206853399399,0.00711581526389425,0.0482415719896204));
#20336=CARTESIAN_POINT('',(5.41506138178544E-18,0.00786705186962924,0.0481508577039061));
#20337=CARTESIAN_POINT('',(0.00231206853399401,0.00711581526389425,0.0480601434181919));
#20338=CARTESIAN_POINT('',(0.004624137067988,0.00636457865815926,0.0479694291324776));
#20339=CARTESIAN_POINT('',(0.00605307400631544,0.00439781569075195,0.0478787148467633));
#20340=CARTESIAN_POINT('',(0.00748201094464287,0.00243105272334464,0.047788000561049));
#20341=CARTESIAN_POINT('',(0.00748201094464287,9.16282075454235E-19,0.0476972862753347));
#20342=CARTESIAN_POINT('',(0.00748201094464287,-0.00243105272334463,0.0476065719896204));
#20343=CARTESIAN_POINT('',(0.00605307400631544,-0.00439781569075195,0.0475158577039062));
#20344=CARTESIAN_POINT('',(0.00530625647659887,-0.00542572183654477,0.0474684469211417));
#20345=CARTESIAN_POINT('',(0.00426198038078368,-0.00614947241717293,0.0474186086270138));
#20346=CARTESIAN_POINT('',(1.0842021724855E-17,1.47451495458029E-17,0.0497741129358333));
#20347=CARTESIAN_POINT('',(-0.00748201094464286,0.,0.0503053219896204));
#20348=CARTESIAN_POINT('',(0.004261979825191,-0.00614947280223435,0.0473052157433551));
#20349=CARTESIAN_POINT('',(0.00426197926959833,-0.00614947318729578,0.0472485192882679));
#20350=CARTESIAN_POINT('',(0.00370259619470581,-0.00534235729046056,0.0472485192882679));
#20351=CARTESIAN_POINT('',(0.00370259619470735,-0.00534235729045949,0.04678567913));
#20352=CARTESIAN_POINT('',(0.00353170713956903,-0.00509578695397652,0.04678567913));
#20353=CARTESIAN_POINT('',(-0.00748201094464286,0.,0.0503053219896204));
#20354=CARTESIAN_POINT('',(-0.0065,0.,0.0503053219896204));
#20355=CARTESIAN_POINT('',(0.0083,0.,0.00847567913));
#20356=CARTESIAN_POINT('',(1.03797133171545E-18,0.,0.00847567913));
#20357=CARTESIAN_POINT('',(-0.0084,0.,0.00847567913));
#20358=CARTESIAN_POINT('',(1.03797133171545E-18,0.,0.00847567913));
#20359=CARTESIAN_POINT('',(-0.0096,0.,0.00847567913));
#20360=CARTESIAN_POINT('',(0.0099,0.,0.01077567913));
#20361=CARTESIAN_POINT('',(1.31964009551934E-18,0.,0.01077567913));
#20362=CARTESIAN_POINT('',(0.0084,0.,0.01077567913));
#20363=CARTESIAN_POINT('',(1.31964009551934E-18,0.,0.01077567913));
#20364=CARTESIAN_POINT('',(0.0096,0.,0.01077567913));
#20365=CARTESIAN_POINT('',(0.0099,0.,0.01962567913));
#20366=CARTESIAN_POINT('',(2.40345251276475E-18,0.,0.01962567913));
#20367=CARTESIAN_POINT('',(-0.0075,0.,0.01962567913));
#20368=CARTESIAN_POINT('',(2.40345251276475E-18,0.,0.01962567913));
#20369=CARTESIAN_POINT('',(-0.0099,0.,0.01962567913));
#20370=CARTESIAN_POINT('',(0.0065,0.,0.04648567913));
#20371=CARTESIAN_POINT('',(5.69285381527454E-18,0.,0.04648567913));
#20372=CARTESIAN_POINT('',(0.00550000000000001,0.,0.04648567913));
#20373=CARTESIAN_POINT('',(5.69285381527454E-18,0.,0.04648567913));
#20374=CARTESIAN_POINT('',(0.00620000000000001,0.,0.04648567913));
#20375=CARTESIAN_POINT('',(0.0045,0.,0.05148567913));
#20376=CARTESIAN_POINT('',(6.30517721484821E-18,0.,0.05148567913));
#20377=CARTESIAN_POINT('',(-0.00549999999999999,0.,0.05148567913));
#20378=CARTESIAN_POINT('',(6.30517721484821E-18,0.,0.05148567913));
#20379=CARTESIAN_POINT('',(-0.00619999999999999,0.,0.05148567913));
#20380=CARTESIAN_POINT('',(0.00261523063261998,0.,0.06962567913));
#20381=CARTESIAN_POINT('',(8.52668650850151E-18,0.,0.06962567913));
#20382=CARTESIAN_POINT('',(-0.00261523063261996,0.,0.06962567913));
#20383=CARTESIAN_POINT('',(8.52668650850151E-18,0.,0.06962567913));
#20384=CARTESIAN_POINT('',(-0.00449999999999999,0.,0.06962567913));
#20385=CARTESIAN_POINT('',(0.00075,0.,0.06462567913));
#20386=CARTESIAN_POINT('',(7.91436310892783E-18,0.,0.06462567913));
#20387=CARTESIAN_POINT('',(0.000950000000000008,0.,0.06462567913));
#20388=CARTESIAN_POINT('',(7.91436310892783E-18,0.,0.06462567913));
#20389=CARTESIAN_POINT('',(0.00280000000000001,0.,0.06462567913));
#20390=CARTESIAN_POINT('',(0.0065,0.,0.01762567913));
#20391=CARTESIAN_POINT('',(2.15852315293528E-18,0.,0.01762567913));
#20392=CARTESIAN_POINT('',(-0.0075,0.,0.01762567913));
#20393=CARTESIAN_POINT('',(2.15852315293528E-18,0.,0.01762567913));
#20394=CARTESIAN_POINT('',(-0.004,0.,0.01762567913));
#20395=CARTESIAN_POINT('',(0.0075,0.,-0.00037432087));
#20396=CARTESIAN_POINT('',(-4.58410855299551E-20,0.,-0.000374320869999999));
#20397=CARTESIAN_POINT('',(-0.0099,0.,-0.000374320869999998));
#20398=CARTESIAN_POINT('',(-4.58410855299551E-20,0.,-0.000374320869999999));
#20399=CARTESIAN_POINT('',(0.008,0.,-0.00037432087));
#20400=CARTESIAN_POINT('',(0.,0.,0.));
#20401=CARTESIAN_POINT('',(6.42764189476295E-18,0.,0.05248567913));
#20402=CARTESIAN_POINT('',(-0.00449999999999999,0.,0.05248567913));
#20403=CARTESIAN_POINT('',(0.,0.,0.));
#20404=CARTESIAN_POINT('',(5.72959321924896E-18,0.,0.04678567913));
#20405=CARTESIAN_POINT('',(6.26843781087379E-18,0.,0.05118567913));
#20406=CARTESIAN_POINT('',(-0.00649999999999999,0.,0.05118567913));
#20407=CARTESIAN_POINT('',(0.,0.,0.));
#20408=CARTESIAN_POINT('',(1.53912544274125E-20,0.,0.000125679130000001));
#20409=CARTESIAN_POINT('',(0.0075,0.,0.00012567913));
#20410=CARTESIAN_POINT('',(2.60208521396521E-18,0.,0.01862567913));
#20411=CARTESIAN_POINT('',(2.28098783285001E-18,0.,0.01862567913));
#20412=CARTESIAN_POINT('',(-0.003,0.,0.01862567913));
#20413=CARTESIAN_POINT('',(0.,0.,0.));
#20414=CARTESIAN_POINT('',(7.88987017294488E-18,0.,0.06442567913));
#20415=CARTESIAN_POINT('',(0.00300000000000001,0.,0.06442567913));
#20416=CARTESIAN_POINT('',(0.,0.,0.));
#20417=CARTESIAN_POINT('',(7.93885604491078E-18,0.,0.06482567913));
#20418=CARTESIAN_POINT('',(0.000750000000000008,0.,0.06482567913));
#20419=CARTESIAN_POINT('',(8.03682778884257E-18,0.,0.06562567913));
#20420=CARTESIAN_POINT('',(-0.000749999999999992,0.,0.06562567913));
#20421=CARTESIAN_POINT('',(8.03682778884257E-18,0.,0.06562567913));
#20422=CARTESIAN_POINT('',(0.,0.,0.));
#20423=CARTESIAN_POINT('',(0.,0.,0.));
#20424=CARTESIAN_POINT('',(2.77084655250895E-18,0.,0.02262567913));
#20425=CARTESIAN_POINT('',(-0.0045,0.,0.02262567913));
#20426=CARTESIAN_POINT('',(5.5703891353598E-18,0.,0.04548567913));
#20427=CARTESIAN_POINT('',(0.0045,0.,0.04548567913));
#20428=CARTESIAN_POINT('',(2.60208521396521E-18,0.,0.02262567913));
#20429=CARTESIAN_POINT('',(0.,0.,0.));
#20430=CARTESIAN_POINT('',(1.35637949949376E-18,0.,0.01107567913));
#20431=CARTESIAN_POINT('',(0.0099,0.,0.01107567913));
#20432=CARTESIAN_POINT('',(0.,0.,0.));
#20433=CARTESIAN_POINT('',(1.05021779970692E-18,0.,0.00857567913));
#20434=CARTESIAN_POINT('',(-0.0083,0.,0.00857567913));
#20435=CARTESIAN_POINT('',(1.30739362752787E-18,0.,0.01067567913));
#20436=CARTESIAN_POINT('',(0.0083,0.,0.01067567913));
#20437=CARTESIAN_POINT('',(0.,0.,0.));
#20438=CARTESIAN_POINT('',(1.00123192774103E-18,0.,0.00817567913));
#20439=CARTESIAN_POINT('',(-0.0099,0.,0.00817567913));
#20440=CARTESIAN_POINT('',(1.30739362752787E-18,0.,0.01067567913));
#20441=CARTESIAN_POINT('',(1.05021779970692E-18,0.,0.00857567913));
#20442=CARTESIAN_POINT('',(7.88987017294488E-18,0.,0.06442567913));
#20443=CARTESIAN_POINT('',(7.93885604491078E-18,0.,0.06482567913));
#20444=CARTESIAN_POINT('',(5.5703891353598E-18,0.,0.04548567913));
#20445=CARTESIAN_POINT('',(6.42764189476295E-18,0.,0.05248567913));
#20446=CARTESIAN_POINT('',(5.72959321924896E-18,0.,0.04678567913));
#20447=CARTESIAN_POINT('',(6.26843781087379E-18,0.,0.05118567913));
#20448=CARTESIAN_POINT('',(1.00123192774103E-18,0.,0.00817567913));
#20449=CARTESIAN_POINT('',(1.35637949949376E-18,0.,0.01107567913));
#20450=CARTESIAN_POINT('',(1.53912544274125E-20,0.,0.000125679130000001));
#20451=CARTESIAN_POINT('',(8.67361737988404E-18,0.,0.07262567913));
#20452=CARTESIAN_POINT('',(6.46618946264691E-18,0.,0.06732567913));
#20453=CARTESIAN_POINT('',(0.00350000000000001,0.,0.06732567913));
#20454=CARTESIAN_POINT('',(6.13299279589414E-18,0.,0.06652567913));
#20455=CARTESIAN_POINT('',(-0.00349999999999999,0.,0.06652567913));
#20456=CARTESIAN_POINT('',(6.13299279589414E-18,0.,0.06652567913));
#20457=CARTESIAN_POINT('',(6.46618946264691E-18,0.,0.06732567913));
#20458=CARTESIAN_POINT('',(5.92325318657326E-19,0.,0.0262148045536099));
#20459=CARTESIAN_POINT('',(0.0081026,-0.0149987,0.00954659375251877));
#20460=CARTESIAN_POINT('',(-0.00697862337013143,-0.0149987,-0.00276303245508544));
#20461=CARTESIAN_POINT('',(-0.00697838813503015,-0.0149986999999202,-0.00276293171953564));
#20462=CARTESIAN_POINT('',(-0.00586855331089345,-0.0149987000001014,-0.00232351824269545));
#20463=CARTESIAN_POINT('',(-0.00586855331089344,-0.0149987,-0.00232351824269545));
#20464=CARTESIAN_POINT('',(-0.00599779136539911,-0.0149987,-0.00199635660720541));
#20465=CARTESIAN_POINT('',(-0.0061497149337953,-0.0149987,-0.0014944673254811));
#20466=CARTESIAN_POINT('',(-0.00626830430592329,-0.0149987,-0.000821050784658449));
#20467=CARTESIAN_POINT('',(-0.00631547536017041,-0.0149987,-0.000277747312869822));
#20468=CARTESIAN_POINT('',(-0.00632000856749698,-0.0149987,0.00015929462411768));
#20469=CARTESIAN_POINT('',(-0.00629375135427824,-0.0149987,0.000623355245044501));
#20470=CARTESIAN_POINT('',(-0.00623620899930142,-0.0149987,0.00106910556953163));
#20471=CARTESIAN_POINT('',(-0.0061375129610423,-0.0149987,0.0015445813003547));
#20472=CARTESIAN_POINT('',(-0.00603763212681053,-0.0149987,0.00190296860679013));
#20473=CARTESIAN_POINT('',(-0.00590739644574497,-0.0149987,0.00228438984678247));
#20474=CARTESIAN_POINT('',(-0.00575937756486985,-0.0149987,0.00264292380533166));
#20475=CARTESIAN_POINT('',(-0.00557245894694935,-0.0149987,0.00302213298449338));
#20476=CARTESIAN_POINT('',(-0.00541853509390254,-0.0149987,0.00329368859104497));
#20477=CARTESIAN_POINT('',(-0.00517827337774273,-0.0149987,0.00367602487863288));
#20478=CARTESIAN_POINT('',(-0.00484358822980369,-0.0149987,0.00412251448769674));
#20479=CARTESIAN_POINT('',(-0.0044755270516579,-0.0149987,0.00452080082599289));
#20480=CARTESIAN_POINT('',(-0.00420113020130818,-0.0149987,0.00477711976686186));
#20481=CARTESIAN_POINT('',(-0.00402782270729364,-0.0149987,0.00492583884298841));
#20482=CARTESIAN_POINT('',(-0.00392453518784697,-0.0149987,0.00501167331557126));
#20483=CARTESIAN_POINT('',(-0.00370431548115027,-0.0149987,0.00518228504503203));
#20484=CARTESIAN_POINT('',(-0.00344389650213363,-0.0149987,0.00536626942805986));
#20485=CARTESIAN_POINT('',(-0.00309226575023302,-0.0149987,0.00558713368776282));
#20486=CARTESIAN_POINT('',(-0.00266255231181167,-0.0149987,0.00581308653683576));
#20487=CARTESIAN_POINT('',(-0.00203864766659636,-0.0149987,0.00607898500594078));
#20488=CARTESIAN_POINT('',(-0.00138277756767913,-0.0149987,0.0062807287260464));
#20489=CARTESIAN_POINT('',(-0.000456382127562958,-0.0149987,0.00643337330921512));
#20490=CARTESIAN_POINT('',(0.00015957483550569,-0.0149987,0.00645053065378608));
#20491=CARTESIAN_POINT('',(0.000677466861402992,-0.0149987,0.00642588067210073));
#20492=CARTESIAN_POINT('',(0.00109099272268039,-0.0149987,0.00637815025448105));
#20493=CARTESIAN_POINT('',(0.00139610309946203,-0.0149987,0.00632631389880589));
#20494=CARTESIAN_POINT('',(0.00183217795033315,-0.0149987,0.00623264988861146));
#20495=CARTESIAN_POINT('',(0.00235498770084253,-0.0149987,0.00607643471891711));
#20496=CARTESIAN_POINT('',(0.00295679228876969,-0.0149987,0.00583342874643564));
#20497=CARTESIAN_POINT('',(0.00357833557139731,-0.0149987,0.00550160366559475));
#20498=CARTESIAN_POINT('',(0.00402830733094401,-0.0149987,0.00520697635216527));
#20499=CARTESIAN_POINT('',(0.00449118687829753,-0.0149987,0.00485208586696231));
#20500=CARTESIAN_POINT('',(0.00484330182310477,-0.0149987,0.00453145167497373));
#20501=CARTESIAN_POINT('',(0.00508460958244847,-0.0149987,0.00428339144142465));
#20502=CARTESIAN_POINT('',(0.00521139975095086,-0.0149987,0.00414577193244223));
#20503=CARTESIAN_POINT('',(0.00532624379513806,-0.0149987,0.00401500546471082));
#20504=CARTESIAN_POINT('',(0.00535761453384072,-0.0149987,0.0039777739014523));
#20505=CARTESIAN_POINT('',(0.0054292549141877,-0.0149987,0.00389240085461715));
#20506=CARTESIAN_POINT('',(0.00554251733739671,-0.0149987,0.00375191503025411));
#20507=CARTESIAN_POINT('',(0.00571509837306046,-0.0149987,0.00352545361202452));
#20508=CARTESIAN_POINT('',(0.00589268626100846,-0.0149987,0.0032739742857001));
#20509=CARTESIAN_POINT('',(0.00603416113007693,-0.0149987,0.00306456557847418));
#20510=CARTESIAN_POINT('',(0.00619405534581928,-0.0149987,0.00281919005005542));
#20511=CARTESIAN_POINT('',(0.00628157614623252,-0.0149987,0.00268140069076854));
#20512=CARTESIAN_POINT('',(0.00636121993813283,-0.0149987,0.00257374771308024));
#20513=CARTESIAN_POINT('',(0.00646897408654251,-0.0149987,0.00258392973544523));
#20514=CARTESIAN_POINT('',(0.00643407102408375,-0.0149987,0.00267920952455317));
#20515=CARTESIAN_POINT('',(0.00638190829137443,-0.0149987,0.00293027097027729));
#20516=CARTESIAN_POINT('',(0.00630182432532361,-0.0149987,0.00316181661572083));
#20517=CARTESIAN_POINT('',(0.00621693397809521,-0.0149987,0.00337277795713077));
#20518=CARTESIAN_POINT('',(0.00613118669110985,-0.0149987,0.00355775221177337));
#20519=CARTESIAN_POINT('',(0.00607475008345043,-0.0149987,0.00367431078349054));
#20520=CARTESIAN_POINT('',(0.00595805328651394,-0.0149987,0.00389628684644505));
#20521=CARTESIAN_POINT('',(0.0058111379186003,-0.0149987,0.00414899740727856));
#20522=CARTESIAN_POINT('',(0.00560145356298951,-0.0149987,0.00446977563568582));
#20523=CARTESIAN_POINT('',(0.00537349142968617,-0.0149987,0.00476906799067895));
#20524=CARTESIAN_POINT('',(0.00516655017896163,-0.0149987,0.00501135781470711));
#20525=CARTESIAN_POINT('',(0.00502907279444013,-0.0149987,0.00516380028597474));
#20526=CARTESIAN_POINT('',(0.00478833180431244,-0.0149987,0.00540951530710551));
#20527=CARTESIAN_POINT('',(0.00448836823269244,-0.0149987,0.00568579113106821));
#20528=CARTESIAN_POINT('',(0.00407816864313292,-0.0149987,0.00601650811311655));
#20529=CARTESIAN_POINT('',(0.00364694800976718,-0.0149987,0.00630338858721496));
#20530=CARTESIAN_POINT('',(0.00327204128829861,-0.0149987,0.00651658046002988));
#20531=CARTESIAN_POINT('',(0.00301183190285494,-0.0149987,0.00665179701590169));
#20532=CARTESIAN_POINT('',(0.00262841659219902,-0.0149987,0.00682726803802908));
#20533=CARTESIAN_POINT('',(0.00214075254818061,-0.0149987,0.00701365129164976));
#20534=CARTESIAN_POINT('',(0.00153382137217885,-0.0149987,0.00719644222076747));
#20535=CARTESIAN_POINT('',(0.000758156059766897,-0.0149987,0.00733307054664956));
#20536=CARTESIAN_POINT('',(0.000157893043096049,-0.0149987,0.0073756635849659));
#20537=CARTESIAN_POINT('',(-0.000275947861242832,-0.0149987,0.00738212320653857));
#20538=CARTESIAN_POINT('',(-0.00080139976413858,-0.0149987,0.00735500387711496));
#20539=CARTESIAN_POINT('',(-0.00129897974408687,-0.0149987,0.00729168926470373));
#20540=CARTESIAN_POINT('',(-0.00179001180637925,-0.0149987,0.00719656643873165));
#20541=CARTESIAN_POINT('',(-0.0023086828513538,-0.0149987,0.00705470345348289));
#20542=CARTESIAN_POINT('',(-0.00269692127236669,-0.0149987,0.00692144102239403));
#20543=CARTESIAN_POINT('',(-0.00310967412185889,-0.0149987,0.00675366172174066));
#20544=CARTESIAN_POINT('',(-0.00349213106262486,-0.0149987,0.00657138531749029));
#20545=CARTESIAN_POINT('',(-0.00390858639104579,-0.0149987,0.00633765016949732));
#20546=CARTESIAN_POINT('',(-0.00415667325880236,-0.0149987,0.00618028307237662));
#20547=CARTESIAN_POINT('',(-0.00452971198711676,-0.0149987,0.00592538388379414));
#20548=CARTESIAN_POINT('',(-0.00495344066841688,-0.0149987,0.00558849047514652));
#20549=CARTESIAN_POINT('',(-0.00534805887266166,-0.0149987,0.00521559800980357));
#20550=CARTESIAN_POINT('',(-0.00565041908749544,-0.0149987,0.00488595952081331));
#20551=CARTESIAN_POINT('',(-0.00584671712296322,-0.0149987,0.00465505029489529));
#20552=CARTESIAN_POINT('',(-0.00611294319695769,-0.0149987,0.00430835586847634));
#20553=CARTESIAN_POINT('',(-0.00641390417825563,-0.0149987,0.00386020440961774));
#20554=CARTESIAN_POINT('',(-0.00673923705289183,-0.0149987,0.00329476077199415));
#20555=CARTESIAN_POINT('',(-0.00711749330497587,-0.0149987,0.00239359665867433));
#20556=CARTESIAN_POINT('',(-0.00735443530757019,-0.0149987,0.00155101673976854));
#20557=CARTESIAN_POINT('',(-0.00750924922811216,-0.0149987,0.000468096518621184));
#20558=CARTESIAN_POINT('',(-0.00751006361744199,-0.0149987,-0.000340745305600475));
#20559=CARTESIAN_POINT('',(-0.00742858049611148,-0.0149987,-0.00111766353747729));
#20560=CARTESIAN_POINT('',(-0.00728899156535579,-0.0149987,-0.00185729201443673));
#20561=CARTESIAN_POINT('',(-0.00711987284693758,-0.0149987,-0.00240489603628845));
#20562=CARTESIAN_POINT('',(-0.00697838813503015,-0.0149987,-0.00276293171953563));
#20563=CARTESIAN_POINT('',(-0.00642363978570473,-0.0149987,-0.00254329890958795));
#20564=CARTESIAN_POINT('',(-0.00697825083808498,-0.0149987000000119,-0.00276288495921407));
#20565=CARTESIAN_POINT('',(-0.00697825074522568,-0.0148409789485013,-0.00276288492244847));
#20566=CARTESIAN_POINT('',(-0.00685793302287164,-0.0145317701099072,-0.00271524776621376));
#20567=CARTESIAN_POINT('',(-0.00642401637047605,-0.0143370055991416,-0.0025434480100466));
#20568=CARTESIAN_POINT('',(-0.00598894144989318,-0.014531011342266,-0.00237118966306239));
#20569=CARTESIAN_POINT('',(-0.00586834301421938,-0.0148410151008114,-0.00232344136456195));
#20570=CARTESIAN_POINT('',(-0.00586834292136777,-0.0149986999999595,-0.0023234413277994));
#20571=CARTESIAN_POINT('',(-0.00642363978570473,0.0149987,0.00254329890958795));
#20572=CARTESIAN_POINT('',(-0.00697862337013143,0.0149987,0.00276303245508544));
#20573=CARTESIAN_POINT('',(-0.00697841856488692,0.0149986999999225,0.00276294376766862));
#20574=CARTESIAN_POINT('',(-0.00586852288100303,0.0149987000001005,0.00232350619462049));
#20575=CARTESIAN_POINT('',(-0.00697825083808499,0.0149987000000326,0.00276288495921407));
#20576=CARTESIAN_POINT('',(-0.0069782507471835,0.0148410138784296,0.00276288492322363));
#20577=CARTESIAN_POINT('',(-0.00685797052311819,0.0145320629891672,0.0027152626136117));
#20578=CARTESIAN_POINT('',(-0.00642393748064774,0.014337247250212,0.00254341677535397));
#20579=CARTESIAN_POINT('',(-0.005988930516056,0.014531353268975,0.00237118533405001));
#20580=CARTESIAN_POINT('',(-0.00586834301229698,0.0148409881450687,0.00232344136380081));
#20581=CARTESIAN_POINT('',(-0.00586834292136777,0.014998699999982,0.00232344132779939));
#20582=CARTESIAN_POINT('',(-0.00595197175455224,-0.0137865115759879,-0.00210067757078177));
#20583=CARTESIAN_POINT('',(-0.00572722807386818,-0.0138068062974582,-0.00273633214012084));
#20584=CARTESIAN_POINT('',(-0.00540062700556022,-0.0138271010189286,-0.00333605257006371));
#20585=CARTESIAN_POINT('',(-0.00446089457736053,-0.0138732614070653,-0.0045475063388789));
#20586=CARTESIAN_POINT('',(-0.00379371989130117,-0.0138991270737317,-0.00511734744676406));
#20587=CARTESIAN_POINT('',(-0.00228794941508494,-0.0139508584070646,-0.005945167953823));
#20588=CARTESIAN_POINT('',(-0.00144935362492807,-0.0139767240737311,-0.00620314735299679));
#20589=CARTESIAN_POINT('',(0.000261328143578779,-0.0140284554070643,-0.00636484946416264));
#20590=CARTESIAN_POINT('',(0.00113341412192876,-0.014054321073731,-0.00626857217615473));
#20591=CARTESIAN_POINT('',(0.00276762342257579,-0.0141060524070644,-0.00573758685231191));
#20592=CARTESIAN_POINT('',(0.00352974674487283,-0.0141319180737312,-0.00530287881647702));
#20593=CARTESIAN_POINT('',(0.00481866923934421,-0.0141836494070648,-0.00416654033650878));
#20594=CARTESIAN_POINT('',(0.00534546841151856,-0.0142095150737316,-0.00346490989237544));
#20595=CARTESIAN_POINT('',(0.0060770888172741,-0.0142612464070653,-0.00191013753954751));
#20596=CARTESIAN_POINT('',(0.00628191005085531,-0.0142871120737322,-0.00105699563085293));
#20597=CARTESIAN_POINT('',(0.00633588343265905,-0.014338843407066,0.000660465495998774));
#20598=CARTESIAN_POINT('',(0.00618503558088158,-0.0143647090737329,0.0015247847141559));
#20599=CARTESIAN_POINT('',(0.00555248386117227,-0.0144164404070667,0.00312242798679427));
#20600=CARTESIAN_POINT('',(0.00507077999324043,-0.0144423060737336,0.00385575204127552));
#20601=CARTESIAN_POINT('',(0.00385575204725291,-0.0144940374070673,0.00507077999924899));
#20602=CARTESIAN_POINT('',(0.00312242796919722,-0.0145199030737342,0.00555248390274121));
#20603=CARTESIAN_POINT('',(0.0015247847317121,-0.0145716344070679,0.00618503553932881));
#20604=CARTESIAN_POINT('',(0.000660465572282654,-0.0145975000737348,0.00633588327242417));
#20605=CARTESIAN_POINT('',(-0.00105699570718024,-0.0146492314070684,0.00628191021108882));
#20606=CARTESIAN_POINT('',(-0.00191013782721369,-0.0146750970737351,0.00607708941665809));
#20607=CARTESIAN_POINT('',(-0.00346490960474784,-0.0147268284070685,0.00534546781211641));
#20608=CARTESIAN_POINT('',(-0.00416653926224855,-0.0147526940737352,0.00481866700200547));
#20609=CARTESIAN_POINT('',(-0.0053028798907647,-0.0148044254070684,0.00352974898218043));
#20610=CARTESIAN_POINT('',(-0.00573759086178014,-0.0148302910737349,0.00276763177246633));
#20611=CARTESIAN_POINT('',(-0.00626856816669886,-0.0148820224070679,0.00113340577200012));
#20612=CARTESIAN_POINT('',(-0.00636483450060213,-0.0149078880737343,0.000261296981248004));
#20613=CARTESIAN_POINT('',(-0.00622057297407274,-0.0149540484021785,-0.00126510394998184));
#20614=CARTESIAN_POINT('',(-0.00604811884979192,-0.0149743430639563,-0.00192585323169751));
#20615=CARTESIAN_POINT('',(-0.00577681582588097,-0.014994637725734,-0.00254307154746529));
#20616=CARTESIAN_POINT('',(-0.00595190184505217,-0.0137902529083118,-0.00210065289705602));
#20617=CARTESIAN_POINT('',(-0.00572716080411827,-0.0138105476297821,-0.00273630000024857));
#20618=CARTESIAN_POINT('',(-0.00540056357193694,-0.0138308423512525,-0.00333601338611308));
#20619=CARTESIAN_POINT('',(-0.00446084218146172,-0.0138770027393892,-0.00454745292567268));
#20620=CARTESIAN_POINT('',(-0.00379367533177166,-0.0139028684060556,-0.00511728734043015));
#20621=CARTESIAN_POINT('',(-0.00228792254173836,-0.0139545997393885,-0.00594509812423768));
#20622=CARTESIAN_POINT('',(-0.00144933660139511,-0.013980465406055,-0.00620307449328773));
#20623=CARTESIAN_POINT('',(0.00026132507412203,-0.0140321967393882,-0.00636477470516471));
#20624=CARTESIAN_POINT('',(0.00113340080929592,-0.0140580624060549,-0.00626849854799165));
#20625=CARTESIAN_POINT('',(0.00276759091516852,-0.0141097937393883,-0.00573751946089189));
#20626=CARTESIAN_POINT('',(0.00352970528586722,-0.0141356594060551,-0.00530281653096521));
#20627=CARTESIAN_POINT('',(0.00481861264116609,-0.0141873907393887,-0.00416649139797816));
#20628=CARTESIAN_POINT('',(0.00534540562576625,-0.0142132564060555,-0.00346486919491779));
#20629=CARTESIAN_POINT('',(0.00607701743819862,-0.0142649877393892,-0.0019101151038294));
#20630=CARTESIAN_POINT('',(0.00628183626603084,-0.0142908534060561,-0.00105698321580138));
#20631=CARTESIAN_POINT('',(0.00633580901388464,-0.0143425847393899,0.000660457738432955));
#20632=CARTESIAN_POINT('',(0.00618496293390622,-0.0143684504060568,0.00152476680463927));
#20633=CARTESIAN_POINT('',(0.00555241864389858,-0.0144201817393906,0.00312239131199329));
#20634=CARTESIAN_POINT('',(0.00507072043386936,-0.0144460474060575,0.00385570675314098));
#20635=CARTESIAN_POINT('',(0.0038557067591183,-0.0144977787393912,0.00507072043987786));
#20636=CARTESIAN_POINT('',(0.00312239129439644,-0.0145236444060581,0.00555241868546704));
#20637=CARTESIAN_POINT('',(0.00152476682219527,-0.0145753757393918,0.00618496289235394));
#20638=CARTESIAN_POINT('',(0.000660457814715938,-0.0146012414060587,0.00633580885365165));
#20639=CARTESIAN_POINT('',(-0.0010569832921278,-0.0146529727393923,0.00628183642626247));
#20640=CARTESIAN_POINT('',(-0.0019101153914922,-0.014678838406059,0.00607701803757557));
#20641=CARTESIAN_POINT('',(-0.00346486890729358,-0.0147305697393924,0.00534540502637115));
#20642=CARTESIAN_POINT('',(-0.00416649032373055,-0.0147564354060591,0.00481861040385363));
#20643=CARTESIAN_POINT('',(-0.00530281760524028,-0.0148081667393923,0.00352970752314855));
#20644=CARTESIAN_POINT('',(-0.00573752347031303,-0.0148340324060588,0.00276759926496099));
#20645=CARTESIAN_POINT('',(-0.00626849453858287,-0.0148857637393918,0.00113339245946536));
#20646=CARTESIAN_POINT('',(-0.00636475974177996,-0.0149116294060582,0.000261293912157276));
#20647=CARTESIAN_POINT('',(-0.00622049990968925,-0.0149577897345023,-0.0012650890905725));
#20648=CARTESIAN_POINT('',(-0.00604804781098619,-0.0149780843962802,-0.00192583061138912));
#20649=CARTESIAN_POINT('',(-0.00577674797369298,-0.0149983790580579,-0.00254304167755531));
#20650=CARTESIAN_POINT('',(-0.00595186676701066,-0.01379399487195,-0.00210064051667888));
#20651=CARTESIAN_POINT('',(-0.00572712705060727,-0.0138142895934203,-0.00273628387363098));
#20652=CARTESIAN_POINT('',(-0.0054005317432546,-0.0138345843148906,-0.00333599372503347));
#20653=CARTESIAN_POINT('',(-0.0044608158911076,-0.0138807447030274,-0.00454742612487075));
#20654=CARTESIAN_POINT('',(-0.00379365297342232,-0.0139066103696938,-0.00511725718126046));
#20655=CARTESIAN_POINT('',(-0.00228790905767159,-0.0139583417030267,-0.00594506308629448));
#20656=CARTESIAN_POINT('',(-0.00144932805960615,-0.0139842073696932,-0.00620303793493879));
#20657=CARTESIAN_POINT('',(0.000261323533980402,-0.0140359387030264,-0.00636473719382177));
#20658=CARTESIAN_POINT('',(0.00113339412950152,-0.0140618043696931,-0.00626846160406045));
#20659=CARTESIAN_POINT('',(0.00276757460413525,-0.0141135357030265,-0.00573748564633126));
#20660=CARTESIAN_POINT('',(0.00352968448324787,-0.0141394013696933,-0.0053027852783634));
#20661=CARTESIAN_POINT('',(0.00481858424226123,-0.0141911327030269,-0.00416646684240551));
#20662=CARTESIAN_POINT('',(0.00534537412216198,-0.0142169983696937,-0.00346484877441547));
#20663=CARTESIAN_POINT('',(0.00607698162277769,-0.0142687297030274,-0.00191010384640302));
#20664=CARTESIAN_POINT('',(0.00628179924349267,-0.0142945953696943,-0.00105697698638059));
#20665=CARTESIAN_POINT('',(0.00633577167325347,-0.0143463267030281,0.000660453845968905));
#20666=CARTESIAN_POINT('',(0.0061849264822993,-0.014372192369695,0.00152475781829597));
#20667=CARTESIAN_POINT('',(0.00555238592024542,-0.0144239237030288,0.0031223729099136));
#20668=CARTESIAN_POINT('',(0.00507069054914571,-0.0144497893696957,0.00385568402920415));
#20669=CARTESIAN_POINT('',(0.00385568403518144,-0.0145015207030294,0.00507069055515417));
#20670=CARTESIAN_POINT('',(0.00312237289231686,-0.0145273863696963,0.00555238596181363));
#20671=CARTESIAN_POINT('',(0.00152475783585187,-0.01457911770303,0.00618492644074726));
#20672=CARTESIAN_POINT('',(0.000660453922251439,-0.0146049833696969,0.00633577151302142));
#20673=CARTESIAN_POINT('',(-0.00105697706270655,-0.0146567147030304,0.00628179940372335));
#20674=CARTESIAN_POINT('',(-0.00191010413406412,-0.0146825803696972,0.00607698222215111));
#20675=CARTESIAN_POINT('',(-0.00346484848679295,-0.0147343117030306,0.00534537352277041));
#20676=CARTESIAN_POINT('',(-0.00416646576816423,-0.0147601773696973,0.00481858200496196));
#20677=CARTESIAN_POINT('',(-0.00530278635263214,-0.0148119087030305,0.00352968672051601));
#20678=CARTESIAN_POINT('',(-0.00573748965572877,-0.014837774369697,0.00276758295387851));
#20679=CARTESIAN_POINT('',(-0.00626845759467531,-0.01488950570303,0.00113338577972016));
#20680=CARTESIAN_POINT('',(-0.0063647222305252,-0.0149153713696963,0.000261292372199303));
#20681=CARTESIAN_POINT('',(-0.00622046324864212,-0.0149615316981405,-0.00126508163466197));
#20682=CARTESIAN_POINT('',(-0.00604801216630023,-0.0149818263599183,-0.00192581926134205));
#20683=CARTESIAN_POINT('',(-0.00577671392793577,-0.0150021210216961,-0.00254302668992214));
#20684=CARTESIAN_POINT('',(-0.00595186676701067,-0.013953649428554,-0.00210064051667888));
#20685=CARTESIAN_POINT('',(-0.00572712705060728,-0.0139739441500243,-0.00273628387363098));
#20686=CARTESIAN_POINT('',(-0.00540053174325461,-0.0139942388714947,-0.00333599372503347));
#20687=CARTESIAN_POINT('',(-0.00446081589110761,-0.0140403992596314,-0.00454742612487077));
#20688=CARTESIAN_POINT('',(-0.00379365297342232,-0.0140662649262978,-0.00511725718126046));
#20689=CARTESIAN_POINT('',(-0.00228790905767159,-0.0141179962596307,-0.0059450630862945));
#20690=CARTESIAN_POINT('',(-0.00144932805960615,-0.0141438619262972,-0.0062030379349388));
#20691=CARTESIAN_POINT('',(0.000261323533980404,-0.0141955932596304,-0.00636473719382177));
#20692=CARTESIAN_POINT('',(0.00113339412950152,-0.0142214589262971,-0.00626846160406046));
#20693=CARTESIAN_POINT('',(0.00276757460413525,-0.0142731902596306,-0.00573748564633127));
#20694=CARTESIAN_POINT('',(0.00352968448324787,-0.0142990559262973,-0.00530278527836341));
#20695=CARTESIAN_POINT('',(0.00481858424226123,-0.0143507872596309,-0.00416646684240551));
#20696=CARTESIAN_POINT('',(0.00534537412216198,-0.0143766529262977,-0.00346484877441547));
#20697=CARTESIAN_POINT('',(0.00607698162277769,-0.0144283842596314,-0.00191010384640302));
#20698=CARTESIAN_POINT('',(0.00628179924349267,-0.0144542499262983,-0.00105697698638059));
#20699=CARTESIAN_POINT('',(0.00633577167325347,-0.0145059812596321,0.000660453845968901));
#20700=CARTESIAN_POINT('',(0.0061849264822993,-0.014531846926299,0.00152475781829598));
#20701=CARTESIAN_POINT('',(0.00555238592024542,-0.0145835782596327,0.0031223729099136));
#20702=CARTESIAN_POINT('',(0.00507069054914571,-0.0146094439262997,0.00385568402920416));
#20703=CARTESIAN_POINT('',(0.00385568403518144,-0.0146611752596335,0.00507069055515417));
#20704=CARTESIAN_POINT('',(0.00312237289231686,-0.0146870409263003,0.00555238596181364));
#20705=CARTESIAN_POINT('',(0.00152475783585187,-0.014738772259634,0.00618492644074727));
#20706=CARTESIAN_POINT('',(0.000660453922251436,-0.0147646379263009,0.00633577151302144));
#20707=CARTESIAN_POINT('',(-0.00105697706270656,-0.0148163692596345,0.00628179940372336));
#20708=CARTESIAN_POINT('',(-0.00191010413406411,-0.0148422349263012,0.00607698222215111));
#20709=CARTESIAN_POINT('',(-0.00346484848679295,-0.0148939662596346,0.00534537352277041));
#20710=CARTESIAN_POINT('',(-0.00416646576816423,-0.0149198319263013,0.00481858200496196));
#20711=CARTESIAN_POINT('',(-0.00530278635263215,-0.0149715632596345,0.003529686720516));
#20712=CARTESIAN_POINT('',(-0.00573748965572878,-0.014997428926301,0.00276758295387852));
#20713=CARTESIAN_POINT('',(-0.00626845759467531,-0.015049160259634,0.00113338577972016));
#20714=CARTESIAN_POINT('',(-0.00636472223052521,-0.0150750259263004,0.000261292372199302));
#20715=CARTESIAN_POINT('',(-0.00622046324864213,-0.0151211862547446,-0.00126508163466197));
#20716=CARTESIAN_POINT('',(-0.00604801216630023,-0.0151414809165224,-0.00192581926134205));
#20717=CARTESIAN_POINT('',(-0.00577671392793576,-0.0151617755783002,-0.00254302668992214));
#20718=CARTESIAN_POINT('',(-0.006012764145877,-0.0141095620215199,-0.00212213352154841));
#20719=CARTESIAN_POINT('',(-0.00578572497281708,-0.0141298567429902,-0.00276428055471631));
#20720=CARTESIAN_POINT('',(-0.00545578805871373,-0.0141501514644605,-0.00337012642351642));
#20721=CARTESIAN_POINT('',(-0.00450645736898466,-0.0141963118525973,-0.00459395376778236));
#20722=CARTESIAN_POINT('',(-0.00383246827817517,-0.0142221775192636,-0.00516961513239118));
#20723=CARTESIAN_POINT('',(-0.00231131812748966,-0.0142739088525966,-0.0060058908523253));
#20724=CARTESIAN_POINT('',(-0.00146415706761363,-0.0142997745192631,-0.0062665052076506));
#20725=CARTESIAN_POINT('',(0.000263997303215911,-0.0143515058525963,-0.00642985891570324));
#20726=CARTESIAN_POINT('',(0.00114499061416944,-0.014377371519263,-0.00633259826843059));
#20727=CARTESIAN_POINT('',(0.00279589144081968,-0.0144291028525964,-0.00579618955399959));
#20728=CARTESIAN_POINT('',(0.00356579895651638,-0.0144549685192632,-0.00535704148684126));
#20729=CARTESIAN_POINT('',(0.00486788627835968,-0.0145066998525967,-0.00420909664575432));
#20730=CARTESIAN_POINT('',(0.00540006608450627,-0.0145325655192636,-0.00350029987182573));
#20731=CARTESIAN_POINT('',(0.00613915913224367,-0.0145842968525973,-0.00192964734799031));
#20732=CARTESIAN_POINT('',(0.00634607237383449,-0.0146101625192642,-0.00106779159808349));
#20733=CARTESIAN_POINT('',(0.00640059703025495,-0.0146618938525979,0.000667211374263152));
#20734=CARTESIAN_POINT('',(0.0062482084450846,-0.0146877595192648,0.00154035859670298));
#20735=CARTESIAN_POINT('',(0.00560919595350615,-0.0147394908525986,0.00315431991637398));
#20736=CARTESIAN_POINT('',(0.00512257204709806,-0.0147653565192655,0.00389513401360513));
#20737=CARTESIAN_POINT('',(0.00389513401964358,-0.0148170878525993,0.00512257205316799));
#20738=CARTESIAN_POINT('',(0.0031543198985972,-0.0148429535192662,0.00560919599549967));
#20739=CARTESIAN_POINT('',(0.0015403586144385,-0.0148946848525999,0.00624820840310741));
#20740=CARTESIAN_POINT('',(0.000667211451326186,-0.0149205505192667,0.00640059686838347));
#20741=CARTESIAN_POINT('',(-0.0010677916751904,-0.0149722818526003,0.00634607253570459));
#20742=CARTESIAN_POINT('',(-0.00192964763859466,-0.0149981475192671,0.00613915973774966));
#20743=CARTESIAN_POINT('',(-0.00350029958126036,-0.0150498788526005,0.00540006547898194));
#20744=CARTESIAN_POINT('',(-0.00420909556052178,-0.0150757445192672,0.00486788401816916));
#20745=CARTESIAN_POINT('',(-0.00535704257210152,-0.0151274758526004,0.00356580121667545));
#20746=CARTESIAN_POINT('',(-0.00579619360441983,-0.0151533415192669,0.00279589987599453));
#20747=CARTESIAN_POINT('',(-0.00633259421802285,-0.0152050728525998,0.00114498217895609));
#20748=CARTESIAN_POINT('',(-0.00642984379930755,-0.0152309385192662,0.000263965822598579));
#20749=CARTESIAN_POINT('',(-0.00628410881095147,-0.0152770988477104,-0.00127802549893492));
#20750=CARTESIAN_POINT('',(-0.0061098932706154,-0.0152973935094883,-0.00194552355745231));
#20751=CARTESIAN_POINT('',(-0.00583581920539624,-0.015317688171266,-0.00256904603240167));
#20752=CARTESIAN_POINT('',(-0.00622068080271541,-0.014330055725037,-0.00219551523027012));
#20753=CARTESIAN_POINT('',(-0.0059857907935527,-0.0143503504465073,-0.00285986720297926));
#20754=CARTESIAN_POINT('',(-0.00564444492036105,-0.0143706451679776,-0.0034866627455973));
#20755=CARTESIAN_POINT('',(-0.00466228712175928,-0.0144168055561143,-0.0047528090772364));
#20756=CARTESIAN_POINT('',(-0.00396499201809,-0.0144426712227807,-0.00534837635923974));
#20757=CARTESIAN_POINT('',(-0.00239124169114502,-0.0144944025561137,-0.00621356983607658));
#20758=CARTESIAN_POINT('',(-0.00151478646786931,-0.0145202682227802,-0.00648319603091008));
#20759=CARTESIAN_POINT('',(0.000273126122402447,-0.0145719995561134,-0.00665219838175603));
#20760=CARTESIAN_POINT('',(0.00118458348939849,-0.01459786522278,-0.00655157453776847));
#20761=CARTESIAN_POINT('',(0.00289257116867112,-0.0146495965561135,-0.0059966172317251));
#20762=CARTESIAN_POINT('',(0.0036891014809477,-0.0146754622227802,-0.00554228376966927));
#20763=CARTESIAN_POINT('',(0.00503621395865962,-0.0147271935561138,-0.00435464389850914));
#20764=CARTESIAN_POINT('',(0.00558679612409495,-0.0147530592227806,-0.00362133748940482));
#20765=CARTESIAN_POINT('',(0.00635144642833699,-0.0148047905561144,-0.00199637303616592));
#20766=CARTESIAN_POINT('',(0.0065655145671437,-0.0148306562227812,-0.00110471499203134));
#20767=CARTESIAN_POINT('',(0.00662192464331508,-0.014882387556115,0.000690283019013507));
#20768=CARTESIAN_POINT('',(0.00646426658067974,-0.0149082532227819,0.00159362298592376));
#20769=CARTESIAN_POINT('',(0.00580315753954379,-0.0149599845561157,0.00326339381910821));
#20770=CARTESIAN_POINT('',(0.00529970656104317,-0.0149858502227826,0.00402982468538238));
#20771=CARTESIAN_POINT('',(0.00402982469162964,-0.0150375815561164,0.00529970656732299));
#20772=CARTESIAN_POINT('',(0.00326339380071673,-0.0150634472227833,0.00580315758298941));
#20773=CARTESIAN_POINT('',(0.00159362300427257,-0.015115178556117,0.00646426653725101));
#20774=CARTESIAN_POINT('',(0.000690283098741327,-0.0151410442227838,0.0066219244758462));
#20775=CARTESIAN_POINT('',(-0.00110471507180453,-0.0151927755561174,0.00656551473461114));
#20776=CARTESIAN_POINT('',(-0.00199637333681914,-0.0152186412227842,0.0063514470547809));
#20777=CARTESIAN_POINT('',(-0.00362133718879192,-0.0152703725561176,0.00558679549763207));
#20778=CARTESIAN_POINT('',(-0.0043546427757501,-0.0152962382227842,0.00503621162031348));
#20779=CARTESIAN_POINT('',(-0.00554228489245698,-0.0153479695561175,0.0036891038192613));
#20780=CARTESIAN_POINT('',(-0.00599662142220568,-0.015373835222784,0.0028925798955277));
#20781=CARTESIAN_POINT('',(-0.00655157034730082,-0.0154255665561169,0.00118457476250211));
#20782=CARTESIAN_POINT('',(-0.00665218274264726,-0.0154514322227833,0.000273093553210122));
#20783=CARTESIAN_POINT('',(-0.00650140835297288,-0.0154975925512275,-0.00132221861588513));
#20784=CARTESIAN_POINT('',(-0.00632116857622288,-0.0155178872130053,-0.002012798232469));
#20785=CARTESIAN_POINT('',(-0.0060376172453096,-0.0155381818747831,-0.00265788162437932));
#20786=CARTESIAN_POINT('',(-0.00636770008068748,-0.0143946368355882,-0.00224740393412229));
#20787=CARTESIAN_POINT('',(-0.00612725869207852,-0.0144149315570585,-0.00292745717015689));
#20788=CARTESIAN_POINT('',(-0.00577784546654924,-0.0144352262785288,-0.00356906636919523));
#20789=CARTESIAN_POINT('',(-0.00477247539665684,-0.0144813866666655,-0.00486513674377885));
#20790=CARTESIAN_POINT('',(-0.00405870045325198,-0.0145072523333319,-0.00547477963495758));
#20791=CARTESIAN_POINT('',(-0.00244775618498231,-0.0145589836666649,-0.00636042105379704));
#20792=CARTESIAN_POINT('',(-0.0015505868601175,-0.0145848493333314,-0.00663641958145776));
#20793=CARTESIAN_POINT('',(0.000279581172353473,-0.0146365806666646,-0.00680941612592736));
#20794=CARTESIAN_POINT('',(0.00121257987995963,-0.0146624463333313,-0.00670641414273623));
#20795=CARTESIAN_POINT('',(0.00296093405983815,-0.0147141776666647,-0.00613834100178227));
#20796=CARTESIAN_POINT('',(0.0037762895321105,-0.0147400433333314,-0.00567326984401944));
#20797=CARTESIAN_POINT('',(0.00515523960286111,-0.014791774666665,-0.00445756134791513));
#20798=CARTESIAN_POINT('',(0.00571883420133934,-0.0148176403333318,-0.00370692400957366));
#20799=CARTESIAN_POINT('',(0.00650155621496434,-0.0148693716666656,-0.00204355522275424));
#20800=CARTESIAN_POINT('',(0.0067206836301111,-0.0148952373333324,-0.00113082377427628));
#20801=CARTESIAN_POINT('',(0.00677842689937372,-0.0149469686666662,0.000706597135469611));
#20802=CARTESIAN_POINT('',(0.00661704275348959,-0.0149728343333331,0.00163128659673755));
#20803=CARTESIAN_POINT('',(0.0059403090923207,-0.0150245656666669,0.00334052071538206));
#20804=CARTESIAN_POINT('',(0.00542495957703594,-0.0150504313333339,0.00412506537275865));
#20805=CARTESIAN_POINT('',(0.00412506537915355,-0.0151021626666676,0.00542495958346417));
#20806=CARTESIAN_POINT('',(0.00334052069655592,-0.0151280283333345,0.00594030913679311));
#20807=CARTESIAN_POINT('',(0.00163128661552,-0.0151797596666682,0.00661704270903447));
#20808=CARTESIAN_POINT('',(0.000706597217081717,-0.015205625333335,0.0067784267279469));
#20809=CARTESIAN_POINT('',(-0.00113082385593482,-0.0152573566666687,0.00672068380153646));
#20810=CARTESIAN_POINT('',(-0.00204355553051307,-0.0152832223333354,0.00650155685621359));
#20811=CARTESIAN_POINT('',(-0.00370692370185609,-0.0153349536666688,0.00571883356007067));
#20812=CARTESIAN_POINT('',(-0.00445756019862087,-0.0153608193333355,0.00515523720925061));
#20813=CARTESIAN_POINT('',(-0.00567327099334306,-0.0154125506666686,0.0037762919256877));
#20814=CARTESIAN_POINT('',(-0.00613834529130048,-0.0154384163333352,0.00296094299294485));
#20815=CARTESIAN_POINT('',(-0.00670640985323126,-0.0154901476666682,0.00121257094681219));
#20816=CARTESIAN_POINT('',(-0.00680940011720463,-0.0155160133333345,0.000279547833422385));
#20817=CARTESIAN_POINT('',(-0.00665506233268495,-0.0155621736617787,-0.0013534678685624));
#20818=CARTESIAN_POINT('',(-0.00647056277751519,-0.0155824683235565,-0.00206036861137542));
#20819=CARTESIAN_POINT('',(-0.00618031000776251,-0.0156027629853343,-0.00272069787387743));
#20820=CARTESIAN_POINT('',(-0.00666173863663163,-0.0143946368355882,-0.00235118134182664));
#20821=CARTESIAN_POINT('',(-0.00641019448913015,-0.0144149315570585,-0.00306263710451214));
#20822=CARTESIAN_POINT('',(-0.00604464655892563,-0.0144352262785288,-0.0037338736163911));
#20823=CARTESIAN_POINT('',(-0.00499285194645195,-0.0144813866666655,-0.00508979207686375));
#20824=CARTESIAN_POINT('',(-0.00424611732357595,-0.0145072523333319,-0.00572758618639328));
#20825=CARTESIAN_POINT('',(-0.00256078517265692,-0.0145589836666649,-0.00665412348923796));
#20826=CARTESIAN_POINT('',(-0.00162218764461389,-0.0145848493333314,-0.00694286668255311));
#20827=CARTESIAN_POINT('',(0.000292491272255523,-0.0146365806666646,-0.00712385161427001));
#20828=CARTESIAN_POINT('',(0.00126857266108191,-0.0146624463333313,-0.00701609335267175));
#20829=CARTESIAN_POINT('',(0.00309765984217221,-0.0147141776666647,-0.00642178854189663));
#20830=CARTESIAN_POINT('',(0.00395066563443612,-0.0147400433333314,-0.00593524199271977));
#20831=CARTESIAN_POINT('',(0.00539329089126408,-0.014791774666665,-0.00466339624672713));
#20832=CARTESIAN_POINT('',(0.00598291035582812,-0.0148176403333318,-0.00387809704991134));
#20833=CARTESIAN_POINT('',(0.00680177578821902,-0.0148693716666656,-0.00213791959593085));
#20834=CARTESIAN_POINT('',(0.00703102175604589,-0.0148952373333324,-0.00118304133876616));
#20835=CARTESIAN_POINT('',(0.00709143141149102,-0.0149469686666662,0.000739225368381816));
#20836=CARTESIAN_POINT('',(0.00692259509910929,-0.0149728343333331,0.0017066138183651));
#20837=CARTESIAN_POINT('',(0.00621461219787452,-0.0150245656666669,0.00349477450792978));
#20838=CARTESIAN_POINT('',(0.00567546560902149,-0.0150504313333339,0.00431554674751118));
#20839=CARTESIAN_POINT('',(0.00431554675420138,-0.0151021626666676,0.00567546561574655));
#20840=CARTESIAN_POINT('',(0.00349477448823432,-0.0151280283333345,0.00621461224440051));
#20841=CARTESIAN_POINT('',(0.00170661383801487,-0.0151797596666682,0.00692259505260138));
#20842=CARTESIAN_POINT('',(0.000739225453762495,-0.015205625333335,0.00709143123214829));
#20843=CARTESIAN_POINT('',(-0.00118304142419541,-0.0152573566666687,0.00703102193538709));
#20844=CARTESIAN_POINT('',(-0.00213791991790094,-0.0152832223333354,0.00680177645907897));
#20845=CARTESIAN_POINT('',(-0.00387809672798443,-0.0153349536666688,0.00598290968494786));
#20846=CARTESIAN_POINT('',(-0.00466339504436239,-0.0153608193333355,0.00539328838712486));
#20847=CARTESIAN_POINT('',(-0.00593524319511522,-0.0154125506666686,0.00395066813854051));
#20848=CARTESIAN_POINT('',(-0.00642179302949008,-0.0154384163333352,0.00309766918777915));
#20849=CARTESIAN_POINT('',(-0.00701608886509214,-0.0154901476666682,0.00126856331543235));
#20850=CARTESIAN_POINT('',(-0.00712383486631935,-0.0155160133333345,0.000292456393846915));
#20851=CARTESIAN_POINT('',(-0.00696237029210909,-0.0155621736617787,-0.00141596637391693));
#20852=CARTESIAN_POINT('',(-0.00676935118009981,-0.0155824683235565,-0.00215550936918826));
#20853=CARTESIAN_POINT('',(-0.0064656955326683,-0.0156027629853343,-0.00284633037287366));
#20854=CARTESIAN_POINT('',(-0.0068087579146037,-0.014330055725037,-0.00240307004567882));
#20855=CARTESIAN_POINT('',(-0.00655166238765596,-0.0143503504465073,-0.00313022707168977));
#20856=CARTESIAN_POINT('',(-0.00617804710511382,-0.0143706451679776,-0.00381627723998903));
#20857=CARTESIAN_POINT('',(-0.00510304022134951,-0.0144168055561143,-0.00520211974340619));
#20858=CARTESIAN_POINT('',(-0.00433982575873793,-0.0144426712227807,-0.00585398946211112));
#20859=CARTESIAN_POINT('',(-0.00261729966649421,-0.0144944025561137,-0.00680097470695842));
#20860=CARTESIAN_POINT('',(-0.00165798803686209,-0.0145202682227802,-0.00709609023310079));
#20861=CARTESIAN_POINT('',(0.000298946322206545,-0.0145719995561134,-0.00728106935844133));
#20862=CARTESIAN_POINT('',(0.00129656905164305,-0.01459786522278,-0.00717093295763951));
#20863=CARTESIAN_POINT('',(0.00316602273333924,-0.0146495965561135,-0.00656351231195381));
#20864=CARTESIAN_POINT('',(0.00403785368559892,-0.0146754622227802,-0.00606622806706994));
#20865=CARTESIAN_POINT('',(0.00551231653546556,-0.0147271935561138,-0.00476631369613313));
#20866=CARTESIAN_POINT('',(0.00611494843307251,-0.0147530592227806,-0.00396368357008018));
#20867=CARTESIAN_POINT('',(0.00695188557484637,-0.0148047905561143,-0.00218510178251917));
#20868=CARTESIAN_POINT('',(0.00718619081901328,-0.0148306562227812,-0.0012091501210111));
#20869=CARTESIAN_POINT('',(0.00724793366754967,-0.014882387556115,0.000755539484837918));
#20870=CARTESIAN_POINT('',(0.00707537127191914,-0.0149082532227819,0.00174427742917887));
#20871=CARTESIAN_POINT('',(0.00635176375065143,-0.0149599845561157,0.00357190140420364));
#20872=CARTESIAN_POINT('',(0.00580071862501426,-0.0149858502227826,0.00441078743488745));
#20873=CARTESIAN_POINT('',(0.0044107874417253,-0.0150375815561164,0.00580071863188774));
#20874=CARTESIAN_POINT('',(0.00357190138407352,-0.0150634472227833,0.00635176379820421));
#20875=CARTESIAN_POINT('',(0.00174427744926231,-0.015115178556117,0.00707537122438484));
#20876=CARTESIAN_POINT('',(0.000755539572102883,-0.0151410442227838,0.00724793348424899));
#20877=CARTESIAN_POINT('',(-0.00120915020832571,-0.0151927755561174,0.0071861910023124));
#20878=CARTESIAN_POINT('',(-0.00218510211159487,-0.0152186412227842,0.00695188626051166));
#20879=CARTESIAN_POINT('',(-0.0039636832410486,-0.0152703725561176,0.00611494774738645));
#20880=CARTESIAN_POINT('',(-0.00476631246723315,-0.0152962382227842,0.00551231397606199));
#20881=CARTESIAN_POINT('',(-0.00606622929600129,-0.0153479695561175,0.00403785624496691));
#20882=CARTESIAN_POINT('',(-0.00656351689858488,-0.015373835222784,0.00316603228519629));
#20883=CARTESIAN_POINT('',(-0.00717092837102258,-0.0154255665561169,0.00129655949974243));
#20884=CARTESIAN_POINT('',(-0.00728105224087671,-0.0154514322227833,0.000298910674059181));
#20885=CARTESIAN_POINT('',(-0.00711602427182116,-0.0154975925512275,-0.00144721562659419));
#20886=CARTESIAN_POINT('',(-0.00691874538139212,-0.0155178872130053,-0.00220307974809468));
#20887=CARTESIAN_POINT('',(-0.0066083882951212,-0.0155381818747831,-0.00290914662237177));
#20888=CARTESIAN_POINT('',(-0.00701667457144212,-0.0141095620215199,-0.00247645175440052));
#20889=CARTESIAN_POINT('',(-0.00675172820839158,-0.0141298567429902,-0.00322581371995272));
#20890=CARTESIAN_POINT('',(-0.00636670396676113,-0.0141501514644605,-0.00393281356206992));
#20891=CARTESIAN_POINT('',(-0.00525886997412413,-0.0141963118525972,-0.00536097505286025));
#20892=CARTESIAN_POINT('',(-0.00447234949865277,-0.0142221775192636,-0.00603275068895968));
#20893=CARTESIAN_POINT('',(-0.00269722323014958,-0.0142739088525966,-0.0070086536907097));
#20894=CARTESIAN_POINT('',(-0.00170861743711776,-0.0142997745192631,-0.00731278105636027));
#20895=CARTESIAN_POINT('',(0.000308075141393081,-0.0143515058525963,-0.00750340882449413));
#20896=CARTESIAN_POINT('',(0.0013361619268721,-0.014377371519263,-0.0073899092269774));
#20897=CARTESIAN_POINT('',(0.00326270246119069,-0.0144291028525964,-0.00676393998967931));
#20898=CARTESIAN_POINT('',(0.00416115621003024,-0.0144549685192631,-0.00625147034989796));
#20899=CARTESIAN_POINT('',(0.0056806442157655,-0.0145066998525967,-0.00491186094888794));
#20900=CARTESIAN_POINT('',(0.00630167847266119,-0.0145325655192636,-0.00408472118765927));
#20901=CARTESIAN_POINT('',(0.00716417287093968,-0.0145842968525973,-0.00225182747069477));
#20902=CARTESIAN_POINT('',(0.00740563301232249,-0.0146101625192642,-0.00124607351495895));
#20903=CARTESIAN_POINT('',(0.00746926128060979,-0.0146618938525979,0.000778611129588272));
#20904=CARTESIAN_POINT('',(0.00729142940751428,-0.0146877595192648,0.00179754181839966));
#20905=CARTESIAN_POINT('',(0.00654572533668907,-0.0147394908525986,0.00368097530693788));
#20906=CARTESIAN_POINT('',(0.00597785313895937,-0.0147653565192655,0.00454547810666471));
#20907=CARTESIAN_POINT('',(0.00454547811371136,-0.0148170878525993,0.00597785314604275));
#20908=CARTESIAN_POINT('',(0.00368097528619306,-0.0148429535192662,0.00654572538569395));
#20909=CARTESIAN_POINT('',(0.00179754183909638,-0.0148946848525999,0.00729142935852844));
#20910=CARTESIAN_POINT('',(0.000778611219518018,-0.0149205505192667,0.00746926109171173));
#20911=CARTESIAN_POINT('',(-0.00124607360493985,-0.0149722818526003,0.00740563320121896));
#20912=CARTESIAN_POINT('',(-0.00225182780981934,-0.0149981475192671,0.0071641735775429));
#20913=CARTESIAN_POINT('',(-0.00408472084858016,-0.0150498788526005,0.00630167776603658));
#20914=CARTESIAN_POINT('',(-0.00491185968246147,-0.0150757445192672,0.00568064157820631));
#20915=CARTESIAN_POINT('',(-0.00625147161635675,-0.0151274758526004,0.00416115884755274));
#20916=CARTESIAN_POINT('',(-0.00676394471637073,-0.0151533415192669,0.00326271230472946));
#20917=CARTESIAN_POINT('',(-0.00738990450030057,-0.0152050728525998,0.00133615208328845));
#20918=CARTESIAN_POINT('',(-0.00750339118421643,-0.0152309385192662,0.00030803840467072));
#20919=CARTESIAN_POINT('',(-0.00733332381384257,-0.0152770988477104,-0.0014914087435444));
#20920=CARTESIAN_POINT('',(-0.00713002068699959,-0.0152973935094882,-0.00227035442311136));
#20921=CARTESIAN_POINT('',(-0.00681018633503457,-0.015317688171266,-0.00299798221434941));
#20922=CARTESIAN_POINT('',(-0.00707757195030846,-0.013953649428554,-0.00249794475927006));
#20923=CARTESIAN_POINT('',(-0.0068103261306014,-0.0139739441500243,-0.00325381040103805));
#20924=CARTESIAN_POINT('',(-0.00642196028222026,-0.0139942388714947,-0.00396694626055288));
#20925=CARTESIAN_POINT('',(-0.0053045114520012,-0.0140403992596314,-0.00540750269577186));
#20926=CARTESIAN_POINT('',(-0.00451116480340562,-0.0140662649262978,-0.0060851086400904));
#20927=CARTESIAN_POINT('',(-0.00272063229996765,-0.0141179962596307,-0.00706948145674051));
#20928=CARTESIAN_POINT('',(-0.00172344644512524,-0.0141438619262972,-0.00737624832907208));
#20929=CARTESIAN_POINT('',(0.000310748910628592,-0.0141955932596305,-0.00756853054637559));
#20930=CARTESIAN_POINT('',(0.00134775841154002,-0.0142214589262971,-0.00745404589134754));
#20931=CARTESIAN_POINT('',(0.00329101929787511,-0.0142731902596305,-0.00682264389734764));
#20932=CARTESIAN_POINT('',(0.00419727068329876,-0.0142990559262973,-0.00630572655837581));
#20933=CARTESIAN_POINT('',(0.00572994625186395,-0.0143507872596309,-0.00495449075223675));
#20934=CARTESIAN_POINT('',(0.00635637043500548,-0.0143766529262977,-0.00412017228506952));
#20935=CARTESIAN_POINT('',(0.00722635038040566,-0.0144283842596314,-0.00227137097228207));
#20936=CARTESIAN_POINT('',(0.00746990614266431,-0.0144542499262983,-0.00125688812666184));
#20937=CARTESIAN_POINT('',(0.00753408663761127,-0.0145059812596321,0.000785368657882526));
#20938=CARTESIAN_POINT('',(0.00735471137029958,-0.014531846926299,0.00181314259680667));
#20939=CARTESIAN_POINT('',(0.00660253536994981,-0.0145835782596328,0.00371292231339825));
#20940=CARTESIAN_POINT('',(0.00602973463691172,-0.0146094439262997,0.00458492809106569));
#20941=CARTESIAN_POINT('',(0.00458492809817351,-0.0146611752596334,0.00602973464405657));
#20942=CARTESIAN_POINT('',(0.00371292229247339,-0.0146870409263003,0.00660253541937999));
#20943=CARTESIAN_POINT('',(0.00181314261768301,-0.014738772259634,0.0073547113208886));
#20944=CARTESIAN_POINT('',(0.000785368748592763,-0.0147646379263009,0.00753408644707377));
#20945=CARTESIAN_POINT('',(-0.00125688821742369,-0.0148163692596345,0.0074699063332002));
#20946=CARTESIAN_POINT('',(-0.00227137131434988,-0.0148422349263012,0.00722635109314146));
#20947=CARTESIAN_POINT('',(-0.00412017194304756,-0.0148939662596347,0.0063563697222481));
#20948=CARTESIAN_POINT('',(-0.00495448947481903,-0.0149198319263013,0.0057299435914135));
#20949=CARTESIAN_POINT('',(-0.00630572783582614,-0.0149715632596345,0.00419727334371219));
#20950=CARTESIAN_POINT('',(-0.00682264866506179,-0.014997428926301,0.00329102922684548));
#20951=CARTESIAN_POINT('',(-0.00745404112364812,-0.015049160259634,0.00134774848252438));
#20952=CARTESIAN_POINT('',(-0.0075685127529988,-0.0150750259263004,0.000310711855069994));
#20953=CARTESIAN_POINT('',(-0.00739696937615192,-0.0151211862547445,-0.00150435260781735));
#20954=CARTESIAN_POINT('',(-0.00719190179131477,-0.0151414809165224,-0.00229005871922163));
#20955=CARTESIAN_POINT('',(-0.00686929161249504,-0.0151617755783001,-0.00302400155682894));
#20956=CARTESIAN_POINT('',(-0.00707757195030845,-0.0137939948724753,-0.00249794475927006));
#20957=CARTESIAN_POINT('',(-0.0068103261306014,-0.0138142895939456,-0.00325381040103805));
#20958=CARTESIAN_POINT('',(-0.00642196028222026,-0.0138345843154159,-0.00396694626055287));
#20959=CARTESIAN_POINT('',(-0.0053045114520012,-0.0138807447035526,-0.00540750269577185));
#20960=CARTESIAN_POINT('',(-0.00451116480340562,-0.013906610370219,-0.0060851086400904));
#20961=CARTESIAN_POINT('',(-0.00272063229996764,-0.013958341703552,-0.00706948145674052));
#20962=CARTESIAN_POINT('',(-0.00172344644512524,-0.0139842073702185,-0.00737624832907208));
#20963=CARTESIAN_POINT('',(0.000310748910628593,-0.0140359387035517,-0.00756853054637559));
#20964=CARTESIAN_POINT('',(0.00134775841154002,-0.0140618043702184,-0.00745404589134754));
#20965=CARTESIAN_POINT('',(0.00329101929787511,-0.0141135357035518,-0.00682264389734764));
#20966=CARTESIAN_POINT('',(0.00419727068329876,-0.0141394013702185,-0.00630572655837581));
#20967=CARTESIAN_POINT('',(0.00572994625186394,-0.0141911327035521,-0.00495449075223675));
#20968=CARTESIAN_POINT('',(0.00635637043500548,-0.014216998370219,-0.00412017228506952));
#20969=CARTESIAN_POINT('',(0.00722635038040566,-0.0142687297035527,-0.00227137097228208));
#20970=CARTESIAN_POINT('',(0.00746990614266432,-0.0142945953702195,-0.00125688812666185));
#20971=CARTESIAN_POINT('',(0.00753408663761127,-0.0143463267035533,0.000785368657882525));
#20972=CARTESIAN_POINT('',(0.00735471137029958,-0.0143721923702202,0.00181314259680667));
#20973=CARTESIAN_POINT('',(0.0066025353699498,-0.014423923703554,0.00371292231339825));
#20974=CARTESIAN_POINT('',(0.00602973463691171,-0.0144497893702209,0.00458492809106569));
#20975=CARTESIAN_POINT('',(0.00458492809817351,-0.0145015207035547,0.00602973464405656));
#20976=CARTESIAN_POINT('',(0.00371292229247339,-0.0145273863702216,0.00660253541937999));
#20977=CARTESIAN_POINT('',(0.00181314261768301,-0.0145791177035553,0.00735471132088859));
#20978=CARTESIAN_POINT('',(0.000785368748592767,-0.0146049833702221,0.00753408644707377));
#20979=CARTESIAN_POINT('',(-0.00125688821742368,-0.0146567147035557,0.0074699063332002));
#20980=CARTESIAN_POINT('',(-0.00227137131434989,-0.0146825803702225,0.00722635109314146));
#20981=CARTESIAN_POINT('',(-0.00412017194304756,-0.0147343117035559,0.00635636972224811));
#20982=CARTESIAN_POINT('',(-0.00495448947481903,-0.0147601773702226,0.00572994359141351));
#20983=CARTESIAN_POINT('',(-0.00630572783582614,-0.0148119087035558,0.00419727334371219));
#20984=CARTESIAN_POINT('',(-0.00682264866506179,-0.0148377743702223,0.00329102922684548));
#20985=CARTESIAN_POINT('',(-0.0074540411236481,-0.0148895057035552,0.00134774848252438));
#20986=CARTESIAN_POINT('',(-0.00756851275299878,-0.0149153713702216,0.000310711855069997));
#20987=CARTESIAN_POINT('',(-0.00739696937615191,-0.0149615316986658,-0.00150435260781735));
#20988=CARTESIAN_POINT('',(-0.00719190179131477,-0.0149818263604436,-0.00229005871922163));
#20989=CARTESIAN_POINT('',(-0.00686929161249505,-0.0150021210222214,-0.00302400155682894));
#20990=CARTESIAN_POINT('',(-0.0070775368722768,-0.0137902529093624,-0.0024979323788964));
#20991=CARTESIAN_POINT('',(-0.00681029237709987,-0.0138105476308327,-0.00325379427442499));
#20992=CARTESIAN_POINT('',(-0.00642192845354686,-0.013830842352303,-0.00396692659947878));
#20993=CARTESIAN_POINT('',(-0.00530448516165446,-0.0138770027404397,-0.00540747589497744));
#20994=CARTESIAN_POINT('',(-0.00451114244506255,-0.0139028684071061,-0.00608507848092918));
#20995=CARTESIAN_POINT('',(-0.00272061881590466,-0.0139545997404391,-0.00706944641880716));
#20996=CARTESIAN_POINT('',(-0.00172343790333868,-0.0139804654071056,-0.0073762117707334));
#20997=CARTESIAN_POINT('',(0.000310747370487398,-0.0140321967404388,-0.00756849303504318));
#20998=CARTESIAN_POINT('',(0.00134775173174749,-0.0140580624071055,-0.00745400894742672));
#20999=CARTESIAN_POINT('',(0.00329100298684642,-0.0141097937404389,-0.00682261008279651));
#21000=CARTESIAN_POINT('',(0.00419724988068525,-0.0141356594071056,-0.00630569530578278));
#21001=CARTESIAN_POINT('',(0.00572991785296706,-0.0141873907404392,-0.00495446619667099));
#21002=CARTESIAN_POINT('',(0.00635633893141005,-0.0142132564071061,-0.00412015186457294));
#21003=CARTESIAN_POINT('',(0.00722631456499478,-0.0142649877404398,-0.00227135971485885));
#21004=CARTESIAN_POINT('',(0.00746986912013654,-0.0142908534071066,-0.0012568818972428));
#21005=CARTESIAN_POINT('',(0.00753404929699058,-0.0143425847404404,0.000785364765419568));
#21006=CARTESIAN_POINT('',(0.00735467491870289,-0.0143684504071073,0.00181313361046589));
#21007=CARTESIAN_POINT('',(0.00660250264630582,-0.0144201817404411,0.00371290391132373));
#21008=CARTESIAN_POINT('',(0.00602970475219645,-0.014446047407108,0.00458490536713524));
#21009=CARTESIAN_POINT('',(0.00458490537424303,-0.0144977787404418,0.00602970475934126));
#21010=CARTESIAN_POINT('',(0.00371290389039897,-0.0145236444071087,0.00660250269573577));
#21011=CARTESIAN_POINT('',(0.00181313363134214,-0.0145753757404424,0.00735467486929215));
#21012=CARTESIAN_POINT('',(0.00078536485612936,-0.0146012414071092,0.00753404910645403));
#21013=CARTESIAN_POINT('',(-0.00125688198800419,-0.0146529727404428,0.00746986931067148));
#21014=CARTESIAN_POINT('',(-0.00227136005692497,-0.0146788384071096,0.00722631527772705));
#21015=CARTESIAN_POINT('',(-0.00412015152255267,-0.014730569740443,0.00635633821865621));
#21016=CARTESIAN_POINT('',(-0.0049544649192596,-0.0147564354071097,0.00572991519252981));
#21017=CARTESIAN_POINT('',(-0.00630569658322677,-0.0148081667404429,0.00419725254108549));
#21018=CARTESIAN_POINT('',(-0.00682261485048703,-0.0148340324071094,0.00329101291576758));
#21019=CARTESIAN_POINT('',(-0.00745400417975091,-0.0148857637404423,0.00134774180278106));
#21020=CARTESIAN_POINT('',(-0.00756847524175456,-0.0149116294071087,0.000310710315112458));
#21021=CARTESIAN_POINT('',(-0.00739693271511507,-0.0149577897355529,-0.00150434515190892));
#21022=CARTESIAN_POINT('',(-0.00719186614663881,-0.0149780843973307,-0.00229004736917774));
#21023=CARTESIAN_POINT('',(-0.00686925756674739,-0.0149983790591085,-0.00302398656919998));
#21024=CARTESIAN_POINT('',(-0.00707746696279632,-0.0137865115775635,-0.00249790770517756));
#21025=CARTESIAN_POINT('',(-0.00681022510736881,-0.0138068062990338,-0.00325376213456173));
#21026=CARTESIAN_POINT('',(-0.00642186501994136,-0.0138271010205041,-0.00396688741553913));
#21027=CARTESIAN_POINT('',(-0.00530443276577034,-0.0138732614086409,-0.00540742248178619));
#21028=CARTESIAN_POINT('',(-0.00451109788554553,-0.0138991270753072,-0.00608501837461211));
#21029=CARTESIAN_POINT('',(-0.00272059194256561,-0.0139508584086402,-0.00706937658924141));
#21030=CARTESIAN_POINT('',(-0.00172342087981049,-0.0139767240753067,-0.00737613891104477));
#21031=CARTESIAN_POINT('',(0.000310744301031509,-0.0140284554086399,-0.0075684182760662));
#21032=CARTESIAN_POINT('',(0.00134773841911838,-0.0140543210753066,-0.00745393531928427));
#21033=CARTESIAN_POINT('',(0.00329097047944826,-0.01410605240864,-0.00682254269139537));
#21034=CARTESIAN_POINT('',(0.00419720842169126,-0.0141319180753068,-0.00630563302028842));
#21035=CARTESIAN_POINT('',(0.0057298612548048,-0.0141836494086403,-0.00495441725815409));
#21036=CARTESIAN_POINT('',(0.00635627614567535,-0.0142095150753072,-0.0041201111671267));
#21037=CARTESIAN_POINT('',(0.00722624318593931,-0.0142612464086409,-0.00227133727914703));
#21038=CARTESIAN_POINT('',(0.00746979533533275,-0.0142871120753078,-0.00125686948219474));
#21039=CARTESIAN_POINT('',(0.00753397487823703,-0.0143388434086415,0.000785357007855923));
#21040=CARTESIAN_POINT('',(0.00735460227174789,-0.0143647090753085,0.00181311570095429));
#21041=CARTESIAN_POINT('',(0.00660243742905041,-0.0144164404086423,0.00371286723653302));
#21042=CARTESIAN_POINT('',(0.00602964519284208,-0.0144423060753091,0.0045848600790134));
#21043=CARTESIAN_POINT('',(0.00458486008612111,-0.0144940374086429,0.00602964519998682));
#21044=CARTESIAN_POINT('',(0.00371286721560847,-0.0145199030753098,0.00660243747847987));
#21045=CARTESIAN_POINT('',(0.00181311572183033,-0.0145716344086435,0.00735460222233764));
#21046=CARTESIAN_POINT('',(0.000785357098564819,-0.0145975000753104,0.00753397468770236));
#21047=CARTESIAN_POINT('',(-0.00125686957295523,-0.0146492314086439,0.0074697955258658));
#21048=CARTESIAN_POINT('',(-0.00227133762120977,-0.0146750970753107,0.00722624389866454));
#21049=CARTESIAN_POINT('',(-0.00412011082510981,-0.0147268284086441,0.00635627543292855));
#21050=CARTESIAN_POINT('',(-0.00495441598075532,-0.0147526940753108,0.00572985859439383));
#21051=CARTESIAN_POINT('',(-0.0063056342977198,-0.014804425408644,0.00419721108206523));
#21052=CARTESIAN_POINT('',(-0.0068225474590388,-0.0148302910753105,0.00329098040827135));
#21053=CARTESIAN_POINT('',(-0.00745393055165556,-0.0148820224086434,0.00134772849025003));
#21054=CARTESIAN_POINT('',(-0.00756840048295334,-0.0149078880753098,0.000310707246022589));
#21055=CARTESIAN_POINT('',(-0.00739685965075207,-0.014954048403754,-0.00150433029250374));
#21056=CARTESIAN_POINT('',(-0.007191795107853,-0.0149743430655318,-0.00229002474887569));
#21057=CARTESIAN_POINT('',(-0.00686918971457842,-0.0149946377273096,-0.00302395669929837));
#21058=CARTESIAN_POINT('',(-0.00586834150890119,-0.0138049000806154,-0.00232344489035294));
#21059=CARTESIAN_POINT('',(-0.00586834159177923,-0.0139608126196482,-0.00232344492316673));
#21060=CARTESIAN_POINT('',(-0.00598842721148222,-0.0142726376300705,-0.00237099026780637));
#21061=CARTESIAN_POINT('',(-0.00642329533287495,-0.0144663808213605,-0.0025431670426404));
#21062=CARTESIAN_POINT('',(-0.00685816345475783,-0.0142726376313009,-0.00271534381766851));
#21063=CARTESIAN_POINT('',(-0.00697824907519072,-0.0139608126212183,-0.00276288916259713));
#21064=CARTESIAN_POINT('',(-0.00697824915847185,-0.0138049000821855,-0.00276288919557052));
#21065=CARTESIAN_POINT('',(-0.00697843089362731,-0.013804899963342,-0.00276295619394444));
#21066=CARTESIAN_POINT('',(-0.00586849430092666,-0.013804899964658,-0.00232350132797368));
#21067=CARTESIAN_POINT('',(-0.00697825089046431,-0.0138048997861662,-0.00276288482710193));
#21068=CARTESIAN_POINT('',(-0.00625400807864927,-0.0138546414753982,-0.00458958735145836));
#21069=CARTESIAN_POINT('',(-0.00330460840350429,-0.0139541248538628,-0.00763147687281364));
#21070=CARTESIAN_POINT('',(0.0030621357297459,-0.0141033499215613,-0.00773406117409333));
#21071=CARTESIAN_POINT('',(0.00763353556729034,-0.0142525749892608,-0.00330332218243761));
#21072=CARTESIAN_POINT('',(0.00773371924336336,-0.0144018000569608,0.00306199180738646));
#21073=CARTESIAN_POINT('',(0.00330333556286005,-0.0145510251246608,0.00763352977367144));
#21074=CARTESIAN_POINT('',(-0.00306212095780749,-0.0147002501923603,0.00773406701808752));
#21075=CARTESIAN_POINT('',(-0.00763305811154286,-0.0148494752600588,0.00330095436087306));
#21076=CARTESIAN_POINT('',(-0.0077007653178123,-0.0149489586385234,-0.00093549061401399));
#21077=CARTESIAN_POINT('',(-0.00697825341078448,-0.0149987003277554,-0.00276287845231342));
#21078=CARTESIAN_POINT('',(-0.00586834506485856,-0.0149987002524587,-0.0023234359064578));
#21079=CARTESIAN_POINT('',(-0.00647593969287228,-0.0149489585632873,-0.000786698594375238));
#21080=CARTESIAN_POINT('',(-0.00641900151649344,-0.0148494751849436,0.00277592940882954));
#21081=CARTESIAN_POINT('',(-0.00257508317452219,-0.0147002501174267,0.00650394465486067));
#21082=CARTESIAN_POINT('',(0.00277793186253437,-0.0145510250499086,0.00641939816488278));
#21083=CARTESIAN_POINT('',(0.00650365218961118,-0.0144017999823902,0.00257497457819126));
#21084=CARTESIAN_POINT('',(0.00641940304225482,-0.0142525749148716,-0.00277792059801396));
#21085=CARTESIAN_POINT('',(0.00257509562175463,-0.0141033498473536,-0.00650393973044446));
#21086=CARTESIAN_POINT('',(-0.00277900223015413,-0.0139541247798366,-0.00641767179346711));
#21087=CARTESIAN_POINT('',(-0.00525929268773173,-0.013854641401493,-0.00385960230652013));
#21088=CARTESIAN_POINT('',(-0.00586834292757561,-0.0138048997123215,-0.00232344131214153));
#21089=CARTESIAN_POINT('',(-0.0069782482560913,-0.0138058164296786,-0.00276288945313269));
#21090=CARTESIAN_POINT('',(-0.00671751942259483,-0.0138237235055873,-0.00342050460393881));
#21091=CARTESIAN_POINT('',(-0.00636415962312206,-0.0138416305814961,-0.00404145862550986));
#21092=CARTESIAN_POINT('',(-0.00530451092621718,-0.0138854033240712,-0.00540750215977932));
#21093=CARTESIAN_POINT('',(-0.00451116435625826,-0.0139112689907376,-0.00608510803693347));
#21094=CARTESIAN_POINT('',(-0.00272063203029814,-0.0139630003240705,-0.00706948075601239));
#21095=CARTESIAN_POINT('',(-0.00172344627429696,-0.0139888659907371,-0.00737624759793717));
#21096=CARTESIAN_POINT('',(0.000310748879827101,-0.0140405973240703,-0.00756852979618164));
#21097=CARTESIAN_POINT('',(0.00134775827794998,-0.0140664629907369,-0.00745404515250133));
#21098=CARTESIAN_POINT('',(0.00329101897166874,-0.0141181943240703,-0.0068226432210861));
#21099=CARTESIAN_POINT('',(0.00419727026726461,-0.0141440599907371,-0.00630572593335119));
#21100=CARTESIAN_POINT('',(0.00572994568391076,-0.0141957913240707,-0.00495449026114685));
#21101=CARTESIAN_POINT('',(0.00635636980496102,-0.0142216569907375,-0.00412017187667741));
#21102=CARTESIAN_POINT('',(0.00722634966412866,-0.0142733883240712,-0.00227137074714344));
#21103=CARTESIAN_POINT('',(0.00746990540224603,-0.0142992539907381,-0.00125688800207892));
#21104=CARTESIAN_POINT('',(0.00753408589083141,-0.0143509853240719,0.000785368580036637));
#21105=CARTESIAN_POINT('',(0.00735471064129942,-0.0143768509907388,0.00181314241708767));
#21106=CARTESIAN_POINT('',(0.00660253471550546,-0.0144285823240726,0.00371292194537279));
#21107=CARTESIAN_POINT('',(0.00602973403924347,-0.0144544479907395,0.00458492763660688));
#21108=CARTESIAN_POINT('',(0.00458492764371473,-0.0145061793240733,0.00602973404638829));
#21109=CARTESIAN_POINT('',(0.00371292192444796,-0.0145320449907402,0.00660253476493562));
#21110=CARTESIAN_POINT('',(0.00181314243796406,-0.0145837763240739,0.00735471059188843));
#21111=CARTESIAN_POINT('',(0.000785368670746929,-0.0146096419907407,0.00753408570029392));
#21112=CARTESIAN_POINT('',(-0.00125688809284068,-0.0146613733240743,0.00746990559278191));
#21113=CARTESIAN_POINT('',(-0.00227137108921116,-0.014687238990741,0.0072263503768644));
#21114=CARTESIAN_POINT('',(-0.00412017153465543,-0.0147389703240745,0.00635636909220375));
#21115=CARTESIAN_POINT('',(-0.00495448898372923,-0.0147648359907411,0.00572994302346061));
#21116=CARTESIAN_POINT('',(-0.00630572721080138,-0.0148165673240743,0.00419727292767782));
#21117=CARTESIAN_POINT('',(-0.00682264798879975,-0.0148424329907408,0.00329102890063817));
#21118=CARTESIAN_POINT('',(-0.00745404038480235,-0.0148941643240738,0.00134774834893538));
#21119=CARTESIAN_POINT('',(-0.00756851200280659,-0.0149200299907402,0.000310711824272237));
#21120=CARTESIAN_POINT('',(-0.00740584135015542,-0.0149638027765913,-0.001410472206315));
#21121=CARTESIAN_POINT('',(-0.0072383566310885,-0.0149817098957761,-0.00210502129056344));
#21122=CARTESIAN_POINT('',(-0.00697825014639974,-0.0149996170149608,-0.00276288468535656));
#21123=CARTESIAN_POINT('',(-0.0069782487171706,-0.0138055108774392,-0.00276288963568727));
#21124=CARTESIAN_POINT('',(-0.00671751986644679,-0.0138234179533479,-0.00342050482994451));
#21125=CARTESIAN_POINT('',(-0.00636416004362621,-0.0138413250292567,-0.00404145889254434));
#21126=CARTESIAN_POINT('',(-0.00530451127670632,-0.0138850977718318,-0.00540750251707348));
#21127=CARTESIAN_POINT('',(-0.00451116465432798,-0.0139109634384982,-0.00608510843899961));
#21128=CARTESIAN_POINT('',(-0.00272063221006061,-0.0139626947718311,-0.00706948122311977));
#21129=CARTESIAN_POINT('',(-0.00172344638817159,-0.0139885604384977,-0.0073762480853138));
#21130=CARTESIAN_POINT('',(0.000310748900359457,-0.0140402917718309,-0.00756853029626308));
#21131=CARTESIAN_POINT('',(0.00134775836700148,-0.0140661574384975,-0.00745404564501834));
#21132=CARTESIAN_POINT('',(0.00329101918911883,-0.0141178887718309,-0.006822643671884));
#21133=CARTESIAN_POINT('',(0.00419727054459417,-0.0141437544384977,-0.0063057263499944));
#21134=CARTESIAN_POINT('',(0.00572994606250998,-0.0141954857718313,-0.0049544905885088));
#21135=CARTESIAN_POINT('',(0.00635637022495046,-0.0142213514384981,-0.00412017214891278));
#21136=CARTESIAN_POINT('',(0.00722635014160097,-0.0142730827718318,-0.00227137089722152));
#21137=CARTESIAN_POINT('',(0.00746990589581098,-0.0142989484384987,-0.00125688808512627));
#21138=CARTESIAN_POINT('',(0.00753408638863701,-0.0143506797718325,0.000785368631928915));
#21139=CARTESIAN_POINT('',(0.00735471112725302,-0.0143765454384994,0.00181314253688886));
#21140=CARTESIAN_POINT('',(0.00660253515175994,-0.0144282767718332,0.00371292219069961));
#21141=CARTESIAN_POINT('',(0.00602973443765085,-0.0144541424385001,0.00458492793955042));
#21142=CARTESIAN_POINT('',(0.00458492794665827,-0.0145058737718339,0.00602973444479567));
#21143=CARTESIAN_POINT('',(0.00371292216977478,-0.0145317394385007,0.00660253520119011));
#21144=CARTESIAN_POINT('',(0.00181314255776525,-0.0145834707718344,0.00735471107784203));
#21145=CARTESIAN_POINT('',(0.000785368722639213,-0.0146093364385013,0.00753408619809951));
#21146=CARTESIAN_POINT('',(-0.00125688817588804,-0.0146610677718349,0.00746990608634688));
#21147=CARTESIAN_POINT('',(-0.00227137123928926,-0.0146869334385016,0.00722635085433675));
#21148=CARTESIAN_POINT('',(-0.00412017180689078,-0.0147386647718351,0.00635636951219315));
#21149=CARTESIAN_POINT('',(-0.00495448931109109,-0.0147645304385017,0.00572994340205966));
#21150=CARTESIAN_POINT('',(-0.00630572762744468,-0.0148162617718349,0.00419727320500755));
#21151=CARTESIAN_POINT('',(-0.00682264843959796,-0.0148421274385014,0.00329102911808892));
#21152=CARTESIAN_POINT('',(-0.00745404087731905,-0.0148938587718344,0.00134774843798622));
#21153=CARTESIAN_POINT('',(-0.00756851250288686,-0.0149197244385008,0.000310711844802144));
#21154=CARTESIAN_POINT('',(-0.00740584183948742,-0.0149634972243519,-0.00141047229951024));
#21155=CARTESIAN_POINT('',(-0.00723835710935415,-0.0149814043435367,-0.00210502142965017));
#21156=CARTESIAN_POINT('',(-0.00697825060747917,-0.0149993114627214,-0.00276288486791082));
#21157=CARTESIAN_POINT('',(-0.00697824894777644,-0.0138052053248561,-0.00276288972699076));
#21158=CARTESIAN_POINT('',(-0.00671752008843649,-0.0138231124007648,-0.0034205049429798));
#21159=CARTESIAN_POINT('',(-0.00636416025393864,-0.0138410194766736,-0.00404145902609992));
#21160=CARTESIAN_POINT('',(-0.0053045114520012,-0.0138847922192487,-0.00540750269577185));
#21161=CARTESIAN_POINT('',(-0.00451116480340563,-0.0139106578859151,-0.0060851086400904));
#21162=CARTESIAN_POINT('',(-0.00272063229996765,-0.013962389219248,-0.00706948145674051));
#21163=CARTESIAN_POINT('',(-0.00172344644512525,-0.0139882548859145,-0.00737624832907208));
#21164=CARTESIAN_POINT('',(0.000310748910628583,-0.0140399862192477,-0.00756853054637559));
#21165=CARTESIAN_POINT('',(0.00134775841154001,-0.0140658518859144,-0.00745404589134754));
#21166=CARTESIAN_POINT('',(0.00329101929787509,-0.0141175832192478,-0.00682264389734765));
#21167=CARTESIAN_POINT('',(0.00419727068329875,-0.0141434488859146,-0.00630572655837581));
#21168=CARTESIAN_POINT('',(0.00572994625186394,-0.0141951802192481,-0.00495449075223676));
#21169=CARTESIAN_POINT('',(0.00635637043500547,-0.014221045885915,-0.00412017228506954));
#21170=CARTESIAN_POINT('',(0.00722635038040566,-0.0142727772192487,-0.0022713709722821));
#21171=CARTESIAN_POINT('',(0.00746990614266431,-0.0142986428859156,-0.00125688812666187));
#21172=CARTESIAN_POINT('',(0.00753408663761127,-0.0143503742192494,0.000785368657882503));
#21173=CARTESIAN_POINT('',(0.00735471137029958,-0.0143762398859162,0.00181314259680665));
#21174=CARTESIAN_POINT('',(0.00660253536994981,-0.0144279712192501,0.00371292231339824));
#21175=CARTESIAN_POINT('',(0.00602973463691173,-0.014453836885917,0.00458492809106568));
#21176=CARTESIAN_POINT('',(0.00458492809817353,-0.0145055682192507,0.00602973464405655));
#21177=CARTESIAN_POINT('',(0.00371292229247341,-0.0145314338859176,0.00660253541937998));
#21178=CARTESIAN_POINT('',(0.00181314261768305,-0.0145831652192513,0.00735471132088858));
#21179=CARTESIAN_POINT('',(0.000785368748592804,-0.0146090308859182,0.00753408644707376));
#21180=CARTESIAN_POINT('',(-0.00125688821742364,-0.0146607622192517,0.00746990633320021));
#21181=CARTESIAN_POINT('',(-0.00227137131434985,-0.0146866278859185,0.00722635109314147));
#21182=CARTESIAN_POINT('',(-0.00412017194304753,-0.0147383592192519,0.00635636972224813));
#21183=CARTESIAN_POINT('',(-0.00495448947481901,-0.0147642248859186,0.00572994359141353));
#21184=CARTESIAN_POINT('',(-0.00630572783582613,-0.0148159562192518,0.00419727334371222));
#21185=CARTESIAN_POINT('',(-0.00682264866506177,-0.0148418218859183,0.00329102922684551));
#21186=CARTESIAN_POINT('',(-0.00745404112364809,-0.0148935532192512,0.00134774848252442));
#21187=CARTESIAN_POINT('',(-0.00756851275299878,-0.0149194188859176,0.000310711855070045));
#21188=CARTESIAN_POINT('',(-0.00740584208422366,-0.0149631916717688,-0.00141047234612124));
#21189=CARTESIAN_POINT('',(-0.00723835734855563,-0.0149810987909535,-0.00210502149921351));
#21190=CARTESIAN_POINT('',(-0.00697825083808507,-0.0149990059101382,-0.00276288495921415));
#21191=CARTESIAN_POINT('',(-0.00697824894777643,-0.0136489871793071,-0.00276288972699076));
#21192=CARTESIAN_POINT('',(-0.00671752008843648,-0.0136668942552158,-0.00342050494297979));
#21193=CARTESIAN_POINT('',(-0.00636416025393864,-0.0136848013311246,-0.00404145902609991));
#21194=CARTESIAN_POINT('',(-0.00530451145200118,-0.0137285740736997,-0.00540750269577185));
#21195=CARTESIAN_POINT('',(-0.00451116480340563,-0.0137544397403661,-0.0060851086400904));
#21196=CARTESIAN_POINT('',(-0.00272063229996765,-0.013806171073699,-0.00706948145674051));
#21197=CARTESIAN_POINT('',(-0.00172344644512525,-0.0138320367403656,-0.00737624832907206));
#21198=CARTESIAN_POINT('',(0.000310748910628584,-0.0138837680736988,-0.00756853054637558));
#21199=CARTESIAN_POINT('',(0.00134775841154,-0.0139096337403654,-0.00745404589134751));
#21200=CARTESIAN_POINT('',(0.00329101929787509,-0.0139613650736988,-0.00682264389734765));
#21201=CARTESIAN_POINT('',(0.00419727068329874,-0.0139872307403656,-0.00630572655837582));
#21202=CARTESIAN_POINT('',(0.00572994625186393,-0.0140389620736992,-0.00495449075223676));
#21203=CARTESIAN_POINT('',(0.00635637043500546,-0.014064827740366,-0.00412017228506954));
#21204=CARTESIAN_POINT('',(0.00722635038040564,-0.0141165590736997,-0.0022713709722821));
#21205=CARTESIAN_POINT('',(0.0074699061426643,-0.0141424247403666,-0.00125688812666187));
#21206=CARTESIAN_POINT('',(0.00753408663761126,-0.0141941560737003,0.000785368657882502));
#21207=CARTESIAN_POINT('',(0.00735471137029958,-0.0142200217403673,0.00181314259680665));
#21208=CARTESIAN_POINT('',(0.00660253536994981,-0.0142717530737011,0.00371292231339823));
#21209=CARTESIAN_POINT('',(0.00602973463691171,-0.014297618740368,0.00458492809106568));
#21210=CARTESIAN_POINT('',(0.00458492809817351,-0.0143493500737018,0.00602973464405654));
#21211=CARTESIAN_POINT('',(0.0037129222924734,-0.0143752157403687,0.00660253541937998));
#21212=CARTESIAN_POINT('',(0.00181314261768305,-0.0144269470737023,0.00735471132088859));
#21213=CARTESIAN_POINT('',(0.000785368748592803,-0.0144528127403691,0.00753408644707377));
#21214=CARTESIAN_POINT('',(-0.00125688821742364,-0.0145045440737028,0.00746990633320021));
#21215=CARTESIAN_POINT('',(-0.00227137131434984,-0.0145304097403695,0.00722635109314145));
#21216=CARTESIAN_POINT('',(-0.00412017194304752,-0.0145821410737029,0.00635636972224812));
#21217=CARTESIAN_POINT('',(-0.00495448947481899,-0.0146080067403696,0.00572994359141353));
#21218=CARTESIAN_POINT('',(-0.00630572783582612,-0.0146597380737028,0.00419727334371222));
#21219=CARTESIAN_POINT('',(-0.00682264866506177,-0.0146856037403693,0.00329102922684551));
#21220=CARTESIAN_POINT('',(-0.0074540411236481,-0.0147373350737023,0.00134774848252442));
#21221=CARTESIAN_POINT('',(-0.00756851275299876,-0.0147632007403686,0.000310711855070046));
#21222=CARTESIAN_POINT('',(-0.00740584208422365,-0.0148069735262198,-0.00141047234612124));
#21223=CARTESIAN_POINT('',(-0.00723835734855561,-0.0148248806454045,-0.0021050214992135));
#21224=CARTESIAN_POINT('',(-0.00697825083808506,-0.0148427877645893,-0.00276288495921415));
#21225=CARTESIAN_POINT('',(-0.00691820617138646,-0.0134930745863413,-0.00273911706262906));
#21226=CARTESIAN_POINT('',(-0.00665972069498067,-0.01351098166225,-0.00339107397613279));
#21227=CARTESIAN_POINT('',(-0.00630940126584622,-0.0135288887381587,-0.00400668519925462));
#21228=CARTESIAN_POINT('',(-0.00525886997412414,-0.0135726614807338,-0.00536097505286025));
#21229=CARTESIAN_POINT('',(-0.00447234949865277,-0.0135985271474002,-0.00603275068895968));
#21230=CARTESIAN_POINT('',(-0.00269722323014959,-0.0136502584807331,-0.00700865369070969));
#21231=CARTESIAN_POINT('',(-0.00170861743711776,-0.0136761241473997,-0.00731278105636027));
#21232=CARTESIAN_POINT('',(0.000308075141393075,-0.0137278554807329,-0.00750340882449412));
#21233=CARTESIAN_POINT('',(0.00133616192687209,-0.0137537211473996,-0.0073899092269774));
#21234=CARTESIAN_POINT('',(0.00326270246119067,-0.013805452480733,-0.00676393998967932));
#21235=CARTESIAN_POINT('',(0.00416115621003024,-0.0138313181473997,-0.00625147034989796));
#21236=CARTESIAN_POINT('',(0.00568064421576549,-0.0138830494807333,-0.00491186094888795));
#21237=CARTESIAN_POINT('',(0.00630167847266118,-0.0139089151474001,-0.00408472118765929));
#21238=CARTESIAN_POINT('',(0.00716417287093968,-0.0139606464807338,-0.0022518274706948));
#21239=CARTESIAN_POINT('',(0.00740563301232249,-0.0139865121474007,-0.00124607351495897));
#21240=CARTESIAN_POINT('',(0.00746926128060979,-0.0140382434807345,0.000778611129588249));
#21241=CARTESIAN_POINT('',(0.00729142940751429,-0.0140641091474014,0.00179754181839964));
#21242=CARTESIAN_POINT('',(0.00654572533668908,-0.0141158404807352,0.00368097530693786));
#21243=CARTESIAN_POINT('',(0.00597785313895938,-0.0141417061474021,0.00454547810666469));
#21244=CARTESIAN_POINT('',(0.00454547811371137,-0.0141934374807359,0.00597785314604273));
#21245=CARTESIAN_POINT('',(0.00368097528619307,-0.0142193031474028,0.00654572538569394));
#21246=CARTESIAN_POINT('',(0.00179754183909641,-0.0142710344807365,0.00729142935852844));
#21247=CARTESIAN_POINT('',(0.000778611219518056,-0.0142969001474033,0.00746926109171172));
#21248=CARTESIAN_POINT('',(-0.0012460736049398,-0.0143486314807369,0.00740563320121896));
#21249=CARTESIAN_POINT('',(-0.00225182780981931,-0.0143744971474037,0.00716417357754291));
#21250=CARTESIAN_POINT('',(-0.00408472084858013,-0.0144262284807371,0.0063016777660366));
#21251=CARTESIAN_POINT('',(-0.00491185968246145,-0.0144520941474037,0.00568064157820633));
#21252=CARTESIAN_POINT('',(-0.00625147161635674,-0.0145038254807369,0.00416115884755278));
#21253=CARTESIAN_POINT('',(-0.00676394471637072,-0.0145296911474035,0.00326271230472949));
#21254=CARTESIAN_POINT('',(-0.00738990450030056,-0.0145814224807364,0.00133615208328849));
#21255=CARTESIAN_POINT('',(-0.00750339118421642,-0.0146072881474028,0.000308038404670769));
#21256=CARTESIAN_POINT('',(-0.00734212017868972,-0.0146510609332539,-0.00139833625348307));
#21257=CARTESIAN_POINT('',(-0.00717607652782788,-0.0146689680524387,-0.00208690931432024));
#21258=CARTESIAN_POINT('',(-0.00691820804543036,-0.0146868751716234,-0.00273911233587572));
#21259=CARTESIAN_POINT('',(-0.00671320730991327,-0.0132725808828242,-0.00265795210955161));
#21260=CARTESIAN_POINT('',(-0.00646238122194688,-0.0132904879587329,-0.00329059036997));
#21261=CARTESIAN_POINT('',(-0.00612244238603927,-0.0133083950346416,-0.00388795992802378));
#21262=CARTESIAN_POINT('',(-0.00510304022134952,-0.0133521677772168,-0.00520211974340619));
#21263=CARTESIAN_POINT('',(-0.00433982575873794,-0.0133780334438831,-0.00585398946211112));
#21264=CARTESIAN_POINT('',(-0.00261729966649422,-0.0134297647772161,-0.00680097470695842));
#21265=CARTESIAN_POINT('',(-0.00165798803686209,-0.0134556304438826,-0.00709609023310079));
#21266=CARTESIAN_POINT('',(0.000298946322206539,-0.0135073617772158,-0.00728106935844134));
#21267=CARTESIAN_POINT('',(0.00129656905164304,-0.0135332274438825,-0.00717093295763951));
#21268=CARTESIAN_POINT('',(0.00316602273333922,-0.0135849587772159,-0.00656351231195381));
#21269=CARTESIAN_POINT('',(0.00403785368559892,-0.0136108244438827,-0.00606622806706994));
#21270=CARTESIAN_POINT('',(0.00551231653546556,-0.0136625557772162,-0.00476631369613314));
#21271=CARTESIAN_POINT('',(0.0061149484330725,-0.0136884214438831,-0.0039636835700802));
#21272=CARTESIAN_POINT('',(0.00695188557484636,-0.0137401527772168,-0.00218510178251919));
#21273=CARTESIAN_POINT('',(0.00718619081901328,-0.0137660184438837,-0.00120915012101113));
#21274=CARTESIAN_POINT('',(0.00724793366754968,-0.0138177497772174,0.000755539484837897));
#21275=CARTESIAN_POINT('',(0.00707537127191915,-0.0138436154438843,0.00174427742917886));
#21276=CARTESIAN_POINT('',(0.00635176375065145,-0.0138953467772181,0.00357190140420363));
#21277=CARTESIAN_POINT('',(0.00580071862501427,-0.013921212443885,0.00441078743488744));
#21278=CARTESIAN_POINT('',(0.00441078744172532,-0.0139729437772188,0.00580071863188773));
#21279=CARTESIAN_POINT('',(0.00357190138407354,-0.0139988094438857,0.00635176379820421));
#21280=CARTESIAN_POINT('',(0.00174427744926234,-0.0140505407772194,0.00707537122438483));
#21281=CARTESIAN_POINT('',(0.000755539572102914,-0.0140764064438862,0.00724793348424898));
#21282=CARTESIAN_POINT('',(-0.00120915020832567,-0.0141281377772198,0.00718619100231241));
#21283=CARTESIAN_POINT('',(-0.00218510211159483,-0.0141540034438866,0.00695188626051167));
#21284=CARTESIAN_POINT('',(-0.00396368324104856,-0.01420573477722,0.00611494774738647));
#21285=CARTESIAN_POINT('',(-0.00476631246723314,-0.0142316004438867,0.005512313976062));
#21286=CARTESIAN_POINT('',(-0.00606622929600128,-0.0142833317772199,0.00403785624496693));
#21287=CARTESIAN_POINT('',(-0.00656351689858486,-0.0143091974438864,0.00316603228519632));
#21288=CARTESIAN_POINT('',(-0.00717092837102258,-0.0143609287772193,0.00129655949974247));
#21289=CARTESIAN_POINT('',(-0.00728105224087672,-0.0143867944438857,0.000298910674059226));
#21290=CARTESIAN_POINT('',(-0.00712455998459551,-0.0144305672297369,-0.00135690104140363));
#21291=CARTESIAN_POINT('',(-0.00696343650502349,-0.0144484743489216,-0.00202507044701344));
#21292=CARTESIAN_POINT('',(-0.0067132091284259,-0.0144663814681063,-0.00265794752286045));
#21293=CARTESIAN_POINT('',(-0.00656825122483005,-0.013207999772273,-0.00260055982083585));
#21294=CARTESIAN_POINT('',(-0.00632284114236892,-0.0132259068481817,-0.00321953773065421));
#21295=CARTESIAN_POINT('',(-0.00599024249432473,-0.0132438139240904,-0.00380400848363825));
#21296=CARTESIAN_POINT('',(-0.00499285194645196,-0.0132875866666655,-0.00508979207686375));
#21297=CARTESIAN_POINT('',(-0.00424611732357595,-0.0133134523333319,-0.00572758618639327));
#21298=CARTESIAN_POINT('',(-0.00256078517265693,-0.0133651836666649,-0.00665412348923796));
#21299=CARTESIAN_POINT('',(-0.0016221876446139,-0.0133910493333314,-0.00694286668255311));
#21300=CARTESIAN_POINT('',(0.000292491272255514,-0.0134427806666646,-0.00712385161427001));
#21301=CARTESIAN_POINT('',(0.0012685726610819,-0.0134686463333313,-0.00701609335267175));
#21302=CARTESIAN_POINT('',(0.0030976598421722,-0.0135203776666647,-0.00642178854189664));
#21303=CARTESIAN_POINT('',(0.00395066563443611,-0.0135462433333314,-0.00593524199271978));
#21304=CARTESIAN_POINT('',(0.00539329089126407,-0.013597974666665,-0.00466339624672714));
#21305=CARTESIAN_POINT('',(0.00598291035582811,-0.0136238403333319,-0.00387809704991136));
#21306=CARTESIAN_POINT('',(0.00680177578821901,-0.0136755716666656,-0.00213791959593088));
#21307=CARTESIAN_POINT('',(0.00703102175604588,-0.0137014373333324,-0.00118304133876618));
#21308=CARTESIAN_POINT('',(0.00709143141149102,-0.0137531686666662,0.000739225368381796));
#21309=CARTESIAN_POINT('',(0.00692259509910929,-0.0137790343333331,0.00170661381836508));
#21310=CARTESIAN_POINT('',(0.00621461219787453,-0.0138307656666669,0.00349477450792977));
#21311=CARTESIAN_POINT('',(0.0056754656090215,-0.0138566313333338,0.00431554674751117));
#21312=CARTESIAN_POINT('',(0.0043155467542014,-0.0139083626666676,0.00567546561574654));
#21313=CARTESIAN_POINT('',(0.00349477448823434,-0.0139342283333345,0.0062146122444005));
#21314=CARTESIAN_POINT('',(0.0017066138380149,-0.0139859596666682,0.00692259505260138));
#21315=CARTESIAN_POINT('',(0.00073922545376252,-0.014011825333335,0.00709143123214829));
#21316=CARTESIAN_POINT('',(-0.00118304142419538,-0.0140635566666686,0.00703102193538709));
#21317=CARTESIAN_POINT('',(-0.0021379199179009,-0.0140894223333354,0.00680177645907898));
#21318=CARTESIAN_POINT('',(-0.0038780967279844,-0.0141411536666688,0.00598290968494787));
#21319=CARTESIAN_POINT('',(-0.00466339504436237,-0.0141670193333355,0.00539328838712488));
#21320=CARTESIAN_POINT('',(-0.0059352431951152,-0.0142187506666686,0.00395066813854053));
#21321=CARTESIAN_POINT('',(-0.00642179302949006,-0.0142446163333352,0.00309766918777917));
#21322=CARTESIAN_POINT('',(-0.00701608886509214,-0.0142963476666681,0.00126856331543239));
#21323=CARTESIAN_POINT('',(-0.00712383486631935,-0.0143222133333345,0.000292456393846961));
#21324=CARTESIAN_POINT('',(-0.00697072169603521,-0.0143659861191856,-0.00132760192196235));
#21325=CARTESIAN_POINT('',(-0.00681307730294682,-0.0143838932383704,-0.00198134376459991));
#21326=CARTESIAN_POINT('',(-0.00656825300407612,-0.0144018003575551,-0.00260055533318361));
#21327=CARTESIAN_POINT('',(-0.00627833905466362,-0.013207999772273,-0.00248577524340433));
#21328=CARTESIAN_POINT('',(-0.00604376098321297,-0.0132259068481817,-0.00307743245202264));
#21329=CARTESIAN_POINT('',(-0.00572584271089564,-0.0132438139240904,-0.00363610559486718));
#21330=CARTESIAN_POINT('',(-0.00477247539665684,-0.0132875866666655,-0.00486513674377885));
#21331=CARTESIAN_POINT('',(-0.00405870045325199,-0.0133134523333319,-0.00547477963495758));
#21332=CARTESIAN_POINT('',(-0.00244775618498232,-0.0133651836666649,-0.00636042105379704));
#21333=CARTESIAN_POINT('',(-0.00155058686011751,-0.0133910493333314,-0.00663641958145776));
#21334=CARTESIAN_POINT('',(0.000279581172353464,-0.0134427806666646,-0.00680941612592736));
#21335=CARTESIAN_POINT('',(0.00121257987995962,-0.0134686463333313,-0.00670641414273624));
#21336=CARTESIAN_POINT('',(0.00296093405983814,-0.0135203776666647,-0.00613834100178228));
#21337=CARTESIAN_POINT('',(0.0037762895321105,-0.0135462433333314,-0.00567326984401944));
#21338=CARTESIAN_POINT('',(0.0051552396028611,-0.013597974666665,-0.00445756134791514));
#21339=CARTESIAN_POINT('',(0.00571883420133933,-0.0136238403333319,-0.00370692400957368));
#21340=CARTESIAN_POINT('',(0.00650155621496433,-0.0136755716666656,-0.00204355522275425));
#21341=CARTESIAN_POINT('',(0.00672068363011109,-0.0137014373333324,-0.0011308237742763));
#21342=CARTESIAN_POINT('',(0.00677842689937372,-0.0137531686666662,0.000706597135469592));
#21343=CARTESIAN_POINT('',(0.00661704275348959,-0.0137790343333331,0.00163128659673753));
#21344=CARTESIAN_POINT('',(0.00594030909232071,-0.0138307656666669,0.00334052071538205));
#21345=CARTESIAN_POINT('',(0.00542495957703595,-0.0138566313333338,0.00412506537275864));
#21346=CARTESIAN_POINT('',(0.00412506537915357,-0.0139083626666676,0.00542495958346416));
#21347=CARTESIAN_POINT('',(0.00334052069655595,-0.0139342283333345,0.0059403091367931));
#21348=CARTESIAN_POINT('',(0.00163128661552003,-0.0139859596666682,0.00661704270903446));
#21349=CARTESIAN_POINT('',(0.000706597217081738,-0.014011825333335,0.00677842672794689));
#21350=CARTESIAN_POINT('',(-0.0011308238559348,-0.0140635566666686,0.00672068380153647));
#21351=CARTESIAN_POINT('',(-0.00204355553051304,-0.0140894223333354,0.0065015568562136));
#21352=CARTESIAN_POINT('',(-0.00370692370185607,-0.0141411536666688,0.00571883356007068));
#21353=CARTESIAN_POINT('',(-0.00445756019862085,-0.0141670193333355,0.00515523720925063));
#21354=CARTESIAN_POINT('',(-0.00567327099334305,-0.0142187506666686,0.00377629192568772));
#21355=CARTESIAN_POINT('',(-0.00613834529130047,-0.0142446163333352,0.00296094299294487));
#21356=CARTESIAN_POINT('',(-0.00670640985323126,-0.0142963476666681,0.00121257094681222));
#21357=CARTESIAN_POINT('',(-0.00680940011720462,-0.0143222133333345,0.000279547833422429));
#21358=CARTESIAN_POINT('',(-0.00666304511891462,-0.0143659861191856,-0.0012690036830798));
#21359=CARTESIAN_POINT('',(-0.0065123588987935,-0.0143838932383704,-0.00189389039977284));
#21360=CARTESIAN_POINT('',(-0.0062783407553766,-0.0144018003575551,-0.00248577095382993));
#21361=CARTESIAN_POINT('',(-0.00613338296958041,-0.0132725808828242,-0.00242838295468858));
#21362=CARTESIAN_POINT('',(-0.005904220903635,-0.0132904879587329,-0.00300637981270685));
#21363=CARTESIAN_POINT('',(-0.0055936428191811,-0.0133083950346417,-0.00355215415048165));
#21364=CARTESIAN_POINT('',(-0.00466228712175929,-0.0133521677772168,-0.00475280907723641));
#21365=CARTESIAN_POINT('',(-0.00396499201809001,-0.0133780334438831,-0.00534837635923974));
#21366=CARTESIAN_POINT('',(-0.00239124169114502,-0.0134297647772161,-0.00621356983607658));
#21367=CARTESIAN_POINT('',(-0.00151478646786932,-0.0134556304438826,-0.00648319603091008));
#21368=CARTESIAN_POINT('',(0.000273126122402439,-0.0135073617772158,-0.00665219838175603));
#21369=CARTESIAN_POINT('',(0.00118458348939848,-0.0135332274438825,-0.00655157453776848));
#21370=CARTESIAN_POINT('',(0.00289257116867111,-0.0135849587772159,-0.0059966172317251));
#21371=CARTESIAN_POINT('',(0.0036891014809477,-0.0136108244438827,-0.00554228376966928));
#21372=CARTESIAN_POINT('',(0.00503621395865961,-0.0136625557772162,-0.00435464389850914));
#21373=CARTESIAN_POINT('',(0.00558679612409495,-0.0136884214438831,-0.00362133748940483));
#21374=CARTESIAN_POINT('',(0.00635144642833699,-0.0137401527772168,-0.00199637303616594));
#21375=CARTESIAN_POINT('',(0.0065655145671437,-0.0137660184438837,-0.00110471499203136));
#21376=CARTESIAN_POINT('',(0.00662192464331508,-0.0138177497772174,0.00069028301901349));
#21377=CARTESIAN_POINT('',(0.00646426658067975,-0.0138436154438843,0.00159362298592375));
#21378=CARTESIAN_POINT('',(0.0058031575395438,-0.0138953467772181,0.0032633938191082));
#21379=CARTESIAN_POINT('',(0.00529970656104318,-0.0139212124438851,0.00402982468538238));
#21380=CARTESIAN_POINT('',(0.00402982469162966,-0.0139729437772188,0.00529970656732298));
#21381=CARTESIAN_POINT('',(0.00326339380071675,-0.0139988094438857,0.0058031575829894));
#21382=CARTESIAN_POINT('',(0.0015936230042726,-0.0140505407772194,0.00646426653725101));
#21383=CARTESIAN_POINT('',(0.00069028309874135,-0.0140764064438862,0.0066219244758462));
#21384=CARTESIAN_POINT('',(-0.0011047150718045,-0.0141281377772198,0.00656551473461115));
#21385=CARTESIAN_POINT('',(-0.00199637333681911,-0.0141540034438866,0.00635144705478091));
#21386=CARTESIAN_POINT('',(-0.0036213371887919,-0.01420573477722,0.00558679549763209));
#21387=CARTESIAN_POINT('',(-0.00435464277575009,-0.0142316004438867,0.0050362116203135));
#21388=CARTESIAN_POINT('',(-0.00554228489245697,-0.0142833317772199,0.00368910381926132));
#21389=CARTESIAN_POINT('',(-0.00599662142220567,-0.0143091974438864,0.00289257989552772));
#21390=CARTESIAN_POINT('',(-0.00655157034730081,-0.0143609287772193,0.00118457476250214));
#21391=CARTESIAN_POINT('',(-0.00665218274264726,-0.0143867944438857,0.000273093553210163));
#21392=CARTESIAN_POINT('',(-0.00650920683035433,-0.0144305672297368,-0.00123970456363852));
#21393=CARTESIAN_POINT('',(-0.00636199969671684,-0.0144484743489216,-0.00185016371735931));
#21394=CARTESIAN_POINT('',(-0.00613338463102684,-0.0144663814681063,-0.00242837876415309));
#21395=CARTESIAN_POINT('',(-0.00592838410810722,-0.0134930745863413,-0.00234721800161112));
#21396=CARTESIAN_POINT('',(-0.00570688143060122,-0.01351098166225,-0.00290589620654406));
#21397=CARTESIAN_POINT('',(-0.00540668393937414,-0.0135288887381587,-0.00343342887925082));
#21398=CARTESIAN_POINT('',(-0.00450645736898467,-0.0135726614807338,-0.00459395376778235));
#21399=CARTESIAN_POINT('',(-0.00383246827817518,-0.0135985271474002,-0.00516961513239117));
#21400=CARTESIAN_POINT('',(-0.00231131812748966,-0.0136502584807331,-0.0060058908523253));
#21401=CARTESIAN_POINT('',(-0.00146415706761364,-0.0136761241473997,-0.0062665052076506));
#21402=CARTESIAN_POINT('',(0.000263997303215905,-0.0137278554807329,-0.00642985891570324));
#21403=CARTESIAN_POINT('',(0.00114499061416943,-0.0137537211473995,-0.00633259826843059));
#21404=CARTESIAN_POINT('',(0.00279589144081966,-0.013805452480733,-0.0057961895539996));
#21405=CARTESIAN_POINT('',(0.00356579895651638,-0.0138313181473997,-0.00535704148684126));
#21406=CARTESIAN_POINT('',(0.00486788627835968,-0.0138830494807333,-0.00420909664575433));
#21407=CARTESIAN_POINT('',(0.00540006608450626,-0.0139089151474001,-0.00350029987182574));
#21408=CARTESIAN_POINT('',(0.00613915913224366,-0.0139606464807339,-0.00192964734799033));
#21409=CARTESIAN_POINT('',(0.00634607237383448,-0.0139865121474007,-0.00106779159808351));
#21410=CARTESIAN_POINT('',(0.00640059703025495,-0.0140382434807345,0.000667211374263139));
#21411=CARTESIAN_POINT('',(0.0062482084450846,-0.0140641091474014,0.00154035859670296));
#21412=CARTESIAN_POINT('',(0.00560919595350616,-0.0141158404807352,0.00315431991637396));
#21413=CARTESIAN_POINT('',(0.00512257204709807,-0.0141417061474021,0.00389513401360513));
#21414=CARTESIAN_POINT('',(0.0038951340196436,-0.0141934374807359,0.00512257205316798));
#21415=CARTESIAN_POINT('',(0.00315431989859721,-0.0142193031474028,0.00560919599549966));
#21416=CARTESIAN_POINT('',(0.00154035861443853,-0.0142710344807365,0.00624820840310741));
#21417=CARTESIAN_POINT('',(0.000667211451326215,-0.0142969001474033,0.00640059686838347));
#21418=CARTESIAN_POINT('',(-0.00106779167519036,-0.0143486314807369,0.0063460725357046));
#21419=CARTESIAN_POINT('',(-0.00192964763859463,-0.0143744971474037,0.00613915973774967));
#21420=CARTESIAN_POINT('',(-0.00350029958126033,-0.0144262284807371,0.00540006547898196));
#21421=CARTESIAN_POINT('',(-0.00420909556052176,-0.0144520941474037,0.00486788401816917));
#21422=CARTESIAN_POINT('',(-0.00535704257210151,-0.0145038254807369,0.00356580121667547));
#21423=CARTESIAN_POINT('',(-0.00579619360441982,-0.0145296911474035,0.00279589987599456));
#21424=CARTESIAN_POINT('',(-0.00633259421802284,-0.0145814224807364,0.00114498217895613));
#21425=CARTESIAN_POINT('',(-0.00642984379930755,-0.0146072881474028,0.000263965822598622));
#21426=CARTESIAN_POINT('',(-0.0062916466362601,-0.0146510609332539,-0.00119826935155907));
#21427=CARTESIAN_POINT('',(-0.00614935967391244,-0.0146689680524387,-0.00178832485005251));
#21428=CARTESIAN_POINT('',(-0.00592838571402237,-0.0146868751716234,-0.00234721395113782));
#21429=CARTESIAN_POINT('',(-0.00586834133171724,-0.0136489871793071,-0.00232344533724942));
#21430=CARTESIAN_POINT('',(-0.0056490820371454,-0.0136668942552158,-0.00287646523969706));
#21431=CARTESIAN_POINT('',(-0.00535192495128173,-0.0136848013311246,-0.00339865505240552));
#21432=CARTESIAN_POINT('',(-0.0044608158911076,-0.0137285740736997,-0.00454742612487075));
#21433=CARTESIAN_POINT('',(-0.00379365297342232,-0.0137544397403661,-0.00511725718126045));
#21434=CARTESIAN_POINT('',(-0.0022879090576716,-0.013806171073699,-0.00594506308629447));
#21435=CARTESIAN_POINT('',(-0.00144932805960616,-0.0138320367403655,-0.00620303793493879));
#21436=CARTESIAN_POINT('',(0.000261323533980394,-0.0138837680736987,-0.00636473719382178));
#21437=CARTESIAN_POINT('',(0.00113339412950151,-0.0139096337403654,-0.00626846160406045));
#21438=CARTESIAN_POINT('',(0.00276757460413524,-0.0139613650736988,-0.00573748564633127));
#21439=CARTESIAN_POINT('',(0.00352968448324787,-0.0139872307403656,-0.00530278527836341));
#21440=CARTESIAN_POINT('',(0.00481858424226122,-0.0140389620736992,-0.00416646684240552));
#21441=CARTESIAN_POINT('',(0.00534537412216196,-0.014064827740366,-0.00346484877441549));
#21442=CARTESIAN_POINT('',(0.00607698162277768,-0.0141165590736997,-0.00191010384640304));
#21443=CARTESIAN_POINT('',(0.00628179924349266,-0.0141424247403666,-0.00105697698638061));
#21444=CARTESIAN_POINT('',(0.00633577167325347,-0.0141941560737004,0.00066045384596889));
#21445=CARTESIAN_POINT('',(0.0061849264822993,-0.0142200217403673,0.00152475781829596));
#21446=CARTESIAN_POINT('',(0.00555238592024542,-0.0142717530737011,0.00312237290991359));
#21447=CARTESIAN_POINT('',(0.00507069054914572,-0.014297618740368,0.00385568402920414));
#21448=CARTESIAN_POINT('',(0.00385568403518145,-0.0143493500737018,0.00507069055515415));
#21449=CARTESIAN_POINT('',(0.00312237289231688,-0.0143752157403686,0.00555238596181362));
#21450=CARTESIAN_POINT('',(0.00152475783585189,-0.0144269470737023,0.00618492644074726));
#21451=CARTESIAN_POINT('',(0.000660453922251468,-0.0144528127403692,0.00633577151302143));
#21452=CARTESIAN_POINT('',(-0.00105697706270652,-0.0145045440737028,0.00628179940372336));
#21453=CARTESIAN_POINT('',(-0.00191010413406409,-0.0145304097403695,0.00607698222215111));
#21454=CARTESIAN_POINT('',(-0.00346484848679293,-0.0145821410737029,0.00534537352277042));
#21455=CARTESIAN_POINT('',(-0.00416646576816421,-0.0146080067403696,0.00481858200496197));
#21456=CARTESIAN_POINT('',(-0.00530278635263212,-0.0146597380737028,0.00352968672051603));
#21457=CARTESIAN_POINT('',(-0.00573748965572876,-0.0146856037403693,0.00276758295387853));
#21458=CARTESIAN_POINT('',(-0.0062684575946753,-0.0147373350737023,0.00113338577972019));
#21459=CARTESIAN_POINT('',(-0.0063647222305252,-0.0147632007403686,0.000261292372199345));
#21460=CARTESIAN_POINT('',(-0.00622792473072616,-0.0148069735262198,-0.0011861332589209));
#21461=CARTESIAN_POINT('',(-0.00608707885318468,-0.0148248806454046,-0.00177021266515924));
#21462=CARTESIAN_POINT('',(-0.00586834292136765,-0.0148427877645893,-0.00232344132779938));
#21463=CARTESIAN_POINT('',(-0.00586834133171724,-0.0138052053248561,-0.00232344533724942));
#21464=CARTESIAN_POINT('',(-0.0056490820371454,-0.0138231124007648,-0.00287646523969706));
#21465=CARTESIAN_POINT('',(-0.00535192495128173,-0.0138410194766736,-0.00339865505240552));
#21466=CARTESIAN_POINT('',(-0.00446081589110761,-0.0138847922192487,-0.00454742612487075));
#21467=CARTESIAN_POINT('',(-0.00379365297342232,-0.0139106578859151,-0.00511725718126046));
#21468=CARTESIAN_POINT('',(-0.0022879090576716,-0.013962389219248,-0.00594506308629448));
#21469=CARTESIAN_POINT('',(-0.00144932805960616,-0.0139882548859145,-0.00620303793493879));
#21470=CARTESIAN_POINT('',(0.000261323533980396,-0.0140399862192477,-0.00636473719382177));
#21471=CARTESIAN_POINT('',(0.00113339412950151,-0.0140658518859144,-0.00626846160406045));
#21472=CARTESIAN_POINT('',(0.00276757460413524,-0.0141175832192478,-0.00573748564633127));
#21473=CARTESIAN_POINT('',(0.00352968448324786,-0.0141434488859146,-0.00530278527836341));
#21474=CARTESIAN_POINT('',(0.00481858424226122,-0.0141951802192481,-0.00416646684240552));
#21475=CARTESIAN_POINT('',(0.00534537412216197,-0.014221045885915,-0.00346484877441549));
#21476=CARTESIAN_POINT('',(0.00607698162277769,-0.0142727772192487,-0.00191010384640303));
#21477=CARTESIAN_POINT('',(0.00628179924349266,-0.0142986428859156,-0.00105697698638061));
#21478=CARTESIAN_POINT('',(0.00633577167325347,-0.0143503742192493,0.000660453845968888));
#21479=CARTESIAN_POINT('',(0.0061849264822993,-0.0143762398859163,0.00152475781829596));
#21480=CARTESIAN_POINT('',(0.00555238592024543,-0.0144279712192501,0.00312237290991359));
#21481=CARTESIAN_POINT('',(0.00507069054914573,-0.014453836885917,0.00385568402920414));
#21482=CARTESIAN_POINT('',(0.00385568403518145,-0.0145055682192507,0.00507069055515416));
#21483=CARTESIAN_POINT('',(0.00312237289231688,-0.0145314338859176,0.00555238596181362));
#21484=CARTESIAN_POINT('',(0.00152475783585189,-0.0145831652192513,0.00618492644074726));
#21485=CARTESIAN_POINT('',(0.000660453922251466,-0.0146090308859181,0.00633577151302142));
#21486=CARTESIAN_POINT('',(-0.00105697706270652,-0.0146607622192517,0.00628179940372335));
#21487=CARTESIAN_POINT('',(-0.00191010413406409,-0.0146866278859185,0.00607698222215111));
#21488=CARTESIAN_POINT('',(-0.00346484848679293,-0.0147383592192519,0.00534537352277042));
#21489=CARTESIAN_POINT('',(-0.00416646576816421,-0.0147642248859186,0.00481858200496197));
#21490=CARTESIAN_POINT('',(-0.00530278635263212,-0.0148159562192518,0.00352968672051603));
#21491=CARTESIAN_POINT('',(-0.00573748965572876,-0.0148418218859183,0.00276758295387854));
#21492=CARTESIAN_POINT('',(-0.0062684575946753,-0.0148935532192512,0.0011333857797202));
#21493=CARTESIAN_POINT('',(-0.0063647222305252,-0.0149194188859176,0.000261292372199344));
#21494=CARTESIAN_POINT('',(-0.00622792473072616,-0.0149631916717688,-0.00118613325892091));
#21495=CARTESIAN_POINT('',(-0.00608707885318469,-0.0149810987909535,-0.00177021266515924));
#21496=CARTESIAN_POINT('',(-0.00586834292136765,-0.0149990059101383,-0.00232344132779938));
#21497=CARTESIAN_POINT('',(-0.00586834156232308,-0.0138055108774392,-0.00232344542855291));
#21498=CARTESIAN_POINT('',(-0.0056490822591351,-0.0138234179533479,-0.00287646535273235));
#21499=CARTESIAN_POINT('',(-0.00535192516159416,-0.0138413250292567,-0.00339865518596109));
#21500=CARTESIAN_POINT('',(-0.00446081606640248,-0.0138850977718318,-0.00454742630356912));
#21501=CARTESIAN_POINT('',(-0.00379365312249997,-0.0139109634384982,-0.00511725738235125));
#21502=CARTESIAN_POINT('',(-0.00228790914757864,-0.0139626947718311,-0.00594506331991522));
#21503=CARTESIAN_POINT('',(-0.00144932811655982,-0.0139885604384977,-0.00620303817869707));
#21504=CARTESIAN_POINT('',(0.000261323544249522,-0.0140402917718309,-0.00636473744393428));
#21505=CARTESIAN_POINT('',(0.00113339417404004,-0.0140661574384975,-0.00626846185038965));
#21506=CARTESIAN_POINT('',(0.0027675747128915,-0.0141178887718309,-0.00573748587179492));
#21507=CARTESIAN_POINT('',(0.00352968462195244,-0.0141437544384977,-0.00530278548674482));
#21508=CARTESIAN_POINT('',(0.00481858443161518,-0.0141954857718313,-0.00416646700613348));
#21509=CARTESIAN_POINT('',(0.00534537433221698,-0.0142213514384981,-0.00346484891057225));
#21510=CARTESIAN_POINT('',(0.00607698186158238,-0.0142730827718318,-0.00191010392146361));
#21511=CARTESIAN_POINT('',(0.00628179949034599,-0.0142989484384987,-0.00105697702791621));
#21512=CARTESIAN_POINT('',(0.00633577192222773,-0.0143506797718325,0.000660453871922476));
#21513=CARTESIAN_POINT('',(0.00618492672534586,-0.0143765454384994,0.00152475787821375));
#21514=CARTESIAN_POINT('',(0.00555238613843529,-0.0144282767718332,0.00312237303261221));
#21515=CARTESIAN_POINT('',(0.00507069074840661,-0.0144541424385001,0.00385568418071939));
#21516=CARTESIAN_POINT('',(0.00385568418669671,-0.0145058737718339,0.00507069075441504));
#21517=CARTESIAN_POINT('',(0.00312237301501551,-0.0145317394385008,0.00555238618000349));
#21518=CARTESIAN_POINT('',(0.00152475789576968,-0.0145834707718345,0.00618492668379381));
#21519=CARTESIAN_POINT('',(0.000660453948205057,-0.0146093364385013,0.00633577176199567));
#21520=CARTESIAN_POINT('',(-0.00105697710424212,-0.0146610677718349,0.00628179965057668));
#21521=CARTESIAN_POINT('',(-0.00191010420912468,-0.0146869334385016,0.00607698246095582));
#21522=CARTESIAN_POINT('',(-0.00346484862294968,-0.0147386647718351,0.0053453737328254));
#21523=CARTESIAN_POINT('',(-0.00416646593189213,-0.0147645304385017,0.00481858219431584));
#21524=CARTESIAN_POINT('',(-0.00530278656101357,-0.0148162617718349,0.0035296868592207));
#21525=CARTESIAN_POINT('',(-0.00573748988119257,-0.0148421274385014,0.00276758306263513));
#21526=CARTESIAN_POINT('',(-0.00626845784100435,-0.0148938587718344,0.0011333858242584));
#21527=CARTESIAN_POINT('',(-0.00636472248063712,-0.0149197244385008,0.000261292382467245));
#21528=CARTESIAN_POINT('',(-0.0062279249754624,-0.0149634972243519,-0.00118613330553191));
#21529=CARTESIAN_POINT('',(-0.00608707909238616,-0.0149814043435367,-0.00177021273472257));
#21530=CARTESIAN_POINT('',(-0.00586834315197355,-0.0149993114627214,-0.00232344141910271));
#21531=CARTESIAN_POINT('',(-0.00586834202340238,-0.0138058164296786,-0.00232344561110749));
#21532=CARTESIAN_POINT('',(-0.00564908270298706,-0.0138237235055873,-0.00287646557873805));
#21533=CARTESIAN_POINT('',(-0.00535192558209831,-0.0138416305814961,-0.00339865545299558));
#21534=CARTESIAN_POINT('',(-0.00446081641689162,-0.0138854033240712,-0.00454742666086328));
#21535=CARTESIAN_POINT('',(-0.00379365342056969,-0.0139112689907376,-0.00511725778441739));
#21536=CARTESIAN_POINT('',(-0.00228790932734111,-0.0139630003240705,-0.0059450637870226));
#21537=CARTESIAN_POINT('',(-0.00144932823043444,-0.0139888659907371,-0.0062030386660737));
#21538=CARTESIAN_POINT('',(0.000261323564781878,-0.0140405973240703,-0.00636473794401572));
#21539=CARTESIAN_POINT('',(0.00113339426309154,-0.0140664629907369,-0.00626846234290666));
#21540=CARTESIAN_POINT('',(0.0027675749303416,-0.0141181943240703,-0.00573748632259282));
#21541=CARTESIAN_POINT('',(0.003529684899282,-0.0141440599907371,-0.00530278590338803));
#21542=CARTESIAN_POINT('',(0.0048185848102144,-0.0141957913240707,-0.00416646733349543));
#21543=CARTESIAN_POINT('',(0.00534537475220642,-0.0142216569907375,-0.00346484918280762));
#21544=CARTESIAN_POINT('',(0.00607698233905469,-0.0142733883240712,-0.00191010407154168));
#21545=CARTESIAN_POINT('',(0.00628179998391094,-0.0142992539907381,-0.00105697711096356));
#21546=CARTESIAN_POINT('',(0.00633577242003333,-0.0143509853240719,0.000660453923814754));
#21547=CARTESIAN_POINT('',(0.00618492721129946,-0.0143768509907388,0.00152475799801494));
#21548=CARTESIAN_POINT('',(0.00555238657468978,-0.0144285823240726,0.00312237327793903));
#21549=CARTESIAN_POINT('',(0.00507069114681398,-0.0144544479907395,0.00385568448366294));
#21550=CARTESIAN_POINT('',(0.00385568448964025,-0.0145061793240733,0.00507069115282241));
#21551=CARTESIAN_POINT('',(0.00312237326034233,-0.0145320449907402,0.00555238661625798));
#21552=CARTESIAN_POINT('',(0.00152475801557087,-0.0145837763240739,0.00618492716974741));
#21553=CARTESIAN_POINT('',(0.000660454000097341,-0.0146096419907407,0.00633577225980127));
#21554=CARTESIAN_POINT('',(-0.00105697718728948,-0.0146613733240743,0.00628180014414165));
#21555=CARTESIAN_POINT('',(-0.00191010435920278,-0.014687238990741,0.00607698293842818));
#21556=CARTESIAN_POINT('',(-0.00346484889518503,-0.0147389703240745,0.0053453741528148));
#21557=CARTESIAN_POINT('',(-0.00416646625925399,-0.0147648359907411,0.00481858257291489));
#21558=CARTESIAN_POINT('',(-0.00530278697765686,-0.0148165673240743,0.00352968713655043));
#21559=CARTESIAN_POINT('',(-0.00573749033199078,-0.0148424329907408,0.00276758328008588));
#21560=CARTESIAN_POINT('',(-0.00626845833352104,-0.0148941643240738,0.00113338591330924));
#21561=CARTESIAN_POINT('',(-0.00636472298071739,-0.0149200299907402,0.000261292402997153));
#21562=CARTESIAN_POINT('',(-0.0062279254647944,-0.0149638027765913,-0.00118613339872715));
#21563=CARTESIAN_POINT('',(-0.00608707957065181,-0.0149817098957761,-0.00177021287380931));
#21564=CARTESIAN_POINT('',(-0.00586834361305298,-0.0149996170149608,-0.00232344160165698));
#21565=CARTESIAN_POINT('',(-0.00697824894777635,-0.0138049000966563,-0.00276288972699073));
#21566=CARTESIAN_POINT('',(-0.00697824903105753,-0.0136489874497574,-0.00276288975996415));
#21567=CARTESIAN_POINT('',(-0.00685816354230486,-0.0133371620879765,-0.00271534445659099));
#21568=CARTESIAN_POINT('',(-0.0064232951405584,-0.0131434186147288,-0.00254316753244141));
#21569=CARTESIAN_POINT('',(-0.0059884267383218,-0.0133371620867462,-0.00237099060809777));
#21570=CARTESIAN_POINT('',(-0.00586834124883921,-0.0136489874481873,-0.00232344530443563));
#21571=CARTESIAN_POINT('',(-0.00586834133171732,-0.0138049000950862,-0.00232344533724946));
#21572=CARTESIAN_POINT('',(-0.0081026,0.0149987,0.00954659375251877));
#21573=CARTESIAN_POINT('',(-0.00586852288100303,0.0149987,0.00232350619462048));
#21574=CARTESIAN_POINT('',(-0.00599813361737052,0.0149987,0.00199544445134711));
#21575=CARTESIAN_POINT('',(-0.00615036467398835,0.0149987,0.00149215405397291));
#21576=CARTESIAN_POINT('',(-0.00626888096798645,0.0149987,0.000816811812020128));
#21577=CARTESIAN_POINT('',(-0.00631571566898991,0.0149987,0.000271946568879761));
#21578=CARTESIAN_POINT('',(-0.00631979103216071,0.0149987,-0.000166419746807652));
#21579=CARTESIAN_POINT('',(-0.00629286640124922,0.0149987,-0.0006317674431288));
#21580=CARTESIAN_POINT('',(-0.00623449486695781,0.0149987,-0.00107869939733934));
#21581=CARTESIAN_POINT('',(-0.0061347047227266,0.0149987,-0.00155532379232996));
#21582=CARTESIAN_POINT('',(-0.0060338297040928,0.0149987,-0.00191460501928228));
#21583=CARTESIAN_POINT('',(-0.00590240684976963,0.0149987,-0.00229687646076972));
#21584=CARTESIAN_POINT('',(-0.00575311671963906,0.0149987,-0.00265615694245076));
#21585=CARTESIAN_POINT('',(-0.00556470003546006,0.0149987,-0.00303603777911812));
#21586=CARTESIAN_POINT('',(-0.00540951335031477,0.0149987,-0.00330813488594238));
#21587=CARTESIAN_POINT('',(-0.00516748245708881,0.0149987,-0.00369094054829892));
#21588=CARTESIAN_POINT('',(-0.00482982949957805,0.0149987,-0.00413835572156689));
#21589=CARTESIAN_POINT('',(-0.00446112385613488,0.0149987,-0.00453464678378625));
#21590=CARTESIAN_POINT('',(-0.00418584385722875,0.0149987,-0.00479017172870383));
#21591=CARTESIAN_POINT('',(-0.00401225692663932,0.0149987,-0.00493819821573241));
#21592=CARTESIAN_POINT('',(-0.00390829841184597,0.0149987,-0.00502401671172254));
#21593=CARTESIAN_POINT('',(-0.00368920130906923,0.0149987,-0.00519269073095229));
#21594=CARTESIAN_POINT('',(-0.00342976117916472,0.0149987,-0.00537492155999436));
#21595=CARTESIAN_POINT('',(-0.00307976849749122,0.0149987,-0.00559356980612197));
#21596=CARTESIAN_POINT('',(-0.00265202463847078,0.0149987,-0.00581741034134192));
#21597=CARTESIAN_POINT('',(-0.00203200389002907,0.0149987,-0.00608060728739528));
#21598=CARTESIAN_POINT('',(-0.00137560083704515,0.0149987,-0.00628233330086265));
#21599=CARTESIAN_POINT('',(-0.000449164143146347,0.0149987,-0.00643265513261176));
#21600=CARTESIAN_POINT('',(0.000282590277332738,0.0149987,-0.00645692920940098));
#21601=CARTESIAN_POINT('',(0.00112268962581157,0.0149987,-0.00638463486570212));
#21602=CARTESIAN_POINT('',(0.00174144901375654,0.0149987,-0.00625866853906934));
#21603=CARTESIAN_POINT('',(0.00239194599947828,0.0149987,-0.00606587477666004));
#21604=CARTESIAN_POINT('',(0.00290790460604307,0.0149987,-0.00584976292120319));
#21605=CARTESIAN_POINT('',(0.00330462789445912,0.0149987,-0.00564960698791436));
#21606=CARTESIAN_POINT('',(0.00361882339497395,0.0149987,-0.00546923879547015));
#21607=CARTESIAN_POINT('',(0.00384299450027782,0.0149987,-0.00532662824985322));
#21608=CARTESIAN_POINT('',(0.00416212926193885,0.0149987,-0.00510689346148155));
#21609=CARTESIAN_POINT('',(0.00453521879647297,0.0149987,-0.00481256371189878));
#21610=CARTESIAN_POINT('',(0.00488723381178878,0.0149987,-0.00448669065789026));
#21611=CARTESIAN_POINT('',(0.00512661788284246,0.0149987,-0.00423556252169337));
#21612=CARTESIAN_POINT('',(0.00525204938765184,0.0149987,-0.00409682965133543));
#21613=CARTESIAN_POINT('',(0.00536734521233373,0.0149987,-0.00396297362800762));
#21614=CARTESIAN_POINT('',(0.00539352292456894,0.0149987,-0.00393124136567307));
#21615=CARTESIAN_POINT('',(0.00546027930440312,0.0149987,-0.00385046561140097));
#21616=CARTESIAN_POINT('',(0.00556424825583872,0.0149987,-0.0037198945025107));
#21617=CARTESIAN_POINT('',(0.00572426624445618,0.0149987,-0.00350871218461249));
#21618=CARTESIAN_POINT('',(0.00589047976960149,0.0149987,-0.00327366681131062));
#21619=CARTESIAN_POINT('',(0.00602152779309136,0.0149987,-0.00308108272382827));
#21620=CARTESIAN_POINT('',(0.00613846929603434,0.0149987,-0.00290345021921962));
#21621=CARTESIAN_POINT('',(0.00619281986756365,0.0149987,-0.00282009893917783));
#21622=CARTESIAN_POINT('',(0.00627282434906237,0.0149987,-0.00269243691200387));
#21623=CARTESIAN_POINT('',(0.00630906243799169,0.0149987,-0.00264532479259586));
#21624=CARTESIAN_POINT('',(0.00635875497946399,0.0149987,-0.00260087005047891));
#21625=CARTESIAN_POINT('',(0.00642241978508077,0.0149987,-0.00256956131751183));
#21626=CARTESIAN_POINT('',(0.00645179410204332,0.0149987,-0.00259471707091186));
#21627=CARTESIAN_POINT('',(0.00643651691696919,0.0149987,-0.00269405563403255));
#21628=CARTESIAN_POINT('',(0.00639400553087227,0.0149987,-0.00288451905087659));
#21629=CARTESIAN_POINT('',(0.00632909652561322,0.0149987,-0.00308798541396548));
#21630=CARTESIAN_POINT('',(0.00623507620707644,0.0149987,-0.00333292149193221));
#21631=CARTESIAN_POINT('',(0.00614730154764063,0.0149987,-0.00352716105907205));
#21632=CARTESIAN_POINT('',(0.00608699524330738,0.0149987,-0.0036536273522041));
#21633=CARTESIAN_POINT('',(0.00597346390559083,0.0149987,-0.0038717266200523));
#21634=CARTESIAN_POINT('',(0.00582819366820487,0.0149987,-0.00412439000312725));
#21635=CARTESIAN_POINT('',(0.0056212361382006,0.0149987,-0.00444390717139348));
#21636=CARTESIAN_POINT('',(0.00539548072186256,0.0149987,-0.00474309520366593));
#21637=CARTESIAN_POINT('',(0.00519017052664321,0.0149987,-0.00498568766096538));
#21638=CARTESIAN_POINT('',(0.00505399676650015,0.0149987,-0.00513815523356757));
#21639=CARTESIAN_POINT('',(0.00481388210436201,0.0149987,-0.00538561010023584));
#21640=CARTESIAN_POINT('',(0.00451483722849798,0.0149987,-0.00566364051147178));
#21641=CARTESIAN_POINT('',(0.00410549859317541,0.0149987,-0.005996807984814));
#21642=CARTESIAN_POINT('',(0.00367483036801044,0.0149987,-0.00628612149675208));
#21643=CARTESIAN_POINT('',(0.00330025304143102,0.0149987,-0.0065013399358742));
#21644=CARTESIAN_POINT('',(0.00304000119389682,0.0149987,-0.00663802952057298));
#21645=CARTESIAN_POINT('',(0.00265721623275325,0.0149987,-0.00681524311387696));
#21646=CARTESIAN_POINT('',(0.00217007333390863,0.0149987,-0.007003890009028));
#21647=CARTESIAN_POINT('',(0.0015636341380728,0.0149987,-0.00718940436680364));
#21648=CARTESIAN_POINT('',(0.000788625433471163,0.0149987,-0.00732937468007596));
#21649=CARTESIAN_POINT('',(0.000188561236036738,0.0149987,-0.00737459670681537));
#21650=CARTESIAN_POINT('',(-0.000245356403268555,0.0149987,-0.00738295831685497));
#21651=CARTESIAN_POINT('',(-0.000770556059278252,0.0149987,-0.00735815400665872));
#21652=CARTESIAN_POINT('',(-0.00126821903781768,0.0149987,-0.00729702843855239));
#21653=CARTESIAN_POINT('',(-0.00175951251098515,0.0149987,-0.00720405474476678));
#21654=CARTESIAN_POINT('',(-0.00227858648456211,0.0149987,-0.00706449573405289));
#21655=CARTESIAN_POINT('',(-0.00266767376332445,0.0149987,-0.00693282703917595));
#21656=CARTESIAN_POINT('',(-0.00308118761978522,0.0149987,-0.00676681939138545));
#21657=CARTESIAN_POINT('',(-0.00346455142098867,0.0149987,-0.00658612068558278));
#21658=CARTESIAN_POINT('',(-0.00388165842624475,0.0149987,-0.00635436861091288));
#21659=CARTESIAN_POINT('',(-0.00413151223126944,0.0149987,-0.00619736451589457));
#21660=CARTESIAN_POINT('',(-0.00450649725080915,0.0149987,-0.00594334153252775));
#21661=CARTESIAN_POINT('',(-0.00493277186581828,0.0149987,-0.00560710240166229));
#21662=CARTESIAN_POINT('',(-0.00532982478874629,0.0149987,-0.00523458823734003));
#21663=CARTESIAN_POINT('',(-0.00563417246466138,0.0149987,-0.00490502780542735));
#21664=CARTESIAN_POINT('',(-0.00583180618591253,0.0149987,-0.00467408667637399));
#21665=CARTESIAN_POINT('',(-0.0060998993556408,0.0149987,-0.00432721456698508));
#21666=CARTESIAN_POINT('',(-0.00640306507679717,0.0149987,-0.00387861753812989));
#21667=CARTESIAN_POINT('',(-0.00673091292818374,0.0149987,-0.00331234831644476));
#21668=CARTESIAN_POINT('',(-0.00711251338688112,0.0149987,-0.00240915825510923));
#21669=CARTESIAN_POINT('',(-0.00735180985367311,0.0149987,-0.00156460169581665));
#21670=CARTESIAN_POINT('',(-0.00750881517846443,0.0149987,-0.00047852369279238));
#21671=CARTESIAN_POINT('',(-0.00751054978552773,0.0149987,0.000332880065926781));
#21672=CARTESIAN_POINT('',(-0.00742945849251632,0.0149987,0.00111231420612745));
#21673=CARTESIAN_POINT('',(-0.00728986753147895,0.0149987,0.00185434184076015));
#21674=CARTESIAN_POINT('',(-0.00712035040730489,0.0149987,0.00240373416514147));
#21675=CARTESIAN_POINT('',(-0.00697841856488692,0.0149987,0.00276294376766862));
#21676=CARTESIAN_POINT('',(-0.0069782482656729,0.0138058421337995,0.00276288935849655));
#21677=CARTESIAN_POINT('',(-0.00671751942982434,0.0138237492104805,0.00342050453854716));
#21678=CARTESIAN_POINT('',(-0.00636415961979208,0.0138416562871614,0.00404145858742542));
#21679=CARTESIAN_POINT('',(-0.00530451090786062,0.0138854290305087,0.00540750214106635));
#21680=CARTESIAN_POINT('',(-0.00451116434064711,0.0139112946971751,0.0060851080158756));
#21681=CARTESIAN_POINT('',(-0.00272063202088324,0.0139630260305081,0.00706948073154804));
#21682=CARTESIAN_POINT('',(-0.00172344626833288,0.0139888916971746,0.00737624757241125));
#21683=CARTESIAN_POINT('',(0.000310748878751736,0.0140406230305078,0.00756852976999031));
#21684=CARTESIAN_POINT('',(0.00134775827328599,0.0140664886971745,0.00745404512670618));
#21685=CARTESIAN_POINT('',(0.00329101896027998,0.0141182200305079,0.00682264319747595));
#21686=CARTESIAN_POINT('',(0.00419727025273972,0.0141440856971746,0.00630572591152988));
#21687=CARTESIAN_POINT('',(0.00572994566408194,0.0141958170305082,0.00495449024400156));
#21688=CARTESIAN_POINT('',(0.00635636978296444,0.014221682697175,0.00412017186241933));
#21689=CARTESIAN_POINT('',(0.00722634963912147,0.0142734140305088,0.00227137073928324));
#21690=CARTESIAN_POINT('',(0.00746990537639599,0.0142992796971756,0.00125688799772938));
#21691=CARTESIAN_POINT('',(0.00753408586475928,0.0143510110305094,-0.000785368577318825));
#21692=CARTESIAN_POINT('',(0.00735471061584803,0.0143768766971763,-0.00181314241081318));
#21693=CARTESIAN_POINT('',(0.00660253469265701,0.0144286080305101,-0.00371292193252399));
#21694=CARTESIAN_POINT('',(0.00602973401837723,0.014454473697177,-0.00458492762074047));
#21695=CARTESIAN_POINT('',(0.00458492762784832,0.0145062050305108,-0.00602973402552206));
#21696=CARTESIAN_POINT('',(0.00371292191159918,0.0145320706971777,-0.00660253474208717));
#21697=CARTESIAN_POINT('',(0.00181314243168958,0.0145838020305114,-0.00735471056643703));
#21698=CARTESIAN_POINT('',(0.000785368668029122,0.0146096676971782,-0.00753408567422178));
#21699=CARTESIAN_POINT('',(-0.00125688808849114,0.0146613990305118,-0.00746990556693187));
#21700=CARTESIAN_POINT('',(-0.00227137108135095,0.0146872646971786,-0.0072263503518572));
#21701=CARTESIAN_POINT('',(-0.00412017152039734,0.014738996030512,-0.00635636907020718));
#21702=CARTESIAN_POINT('',(-0.00495448896658392,0.0147648616971786,-0.00572994300363182));
#21703=CARTESIAN_POINT('',(-0.00630572718898005,0.0148165930305118,-0.00419727291315293));
#21704=CARTESIAN_POINT('',(-0.00682264796518959,0.0148424586971784,-0.00329102888924939));
#21705=CARTESIAN_POINT('',(-0.00745404035900722,0.0148941900305113,-0.00134774834427143));
#21706=CARTESIAN_POINT('',(-0.00756851197661531,0.0149200556971777,-0.000310711823197));
#21707=CARTESIAN_POINT('',(-0.00740584132452708,0.0149638284830288,0.00141047220143395));
#21708=CARTESIAN_POINT('',(-0.00723835660603977,0.0149817356022136,0.00210502128327883));
#21709=CARTESIAN_POINT('',(-0.00697825012225115,0.0149996427213983,0.00276288467579534));
#21710=CARTESIAN_POINT('',(-0.00697824874285721,0.0138055280127714,0.00276288954742755));
#21711=CARTESIAN_POINT('',(-0.00671751988917958,0.0138234350894524,0.00342050477244699));
#21712=CARTESIAN_POINT('',(-0.00636416005498398,0.0138413421661333,0.00404145886378712));
#21713=CARTESIAN_POINT('',(-0.00530451127059196,0.0138851149094806,0.00540750251084041));
#21714=CARTESIAN_POINT('',(-0.00451116464912809,0.013910980576147,0.00608510843198548));
#21715=CARTESIAN_POINT('',(-0.00272063220692462,0.01396271190948,0.00706948121497098));
#21716=CARTESIAN_POINT('',(-0.00172344638618502,0.0139885775761465,0.00737624807681142));
#21717=CARTESIAN_POINT('',(0.000310748900001265,0.0140403089094797,0.00756853028753906));
#21718=CARTESIAN_POINT('',(0.00134775836544796,0.0140661745761464,0.00745404563642627));
#21719=CARTESIAN_POINT('',(0.00329101918532537,0.0141179059094798,0.00682264366401973));
#21720=CARTESIAN_POINT('',(0.00419727053975609,0.0141437715761465,0.00630572634272598));
#21721=CARTESIAN_POINT('',(0.00572994605590523,0.0141955029094801,0.00495449058279791));
#21722=CARTESIAN_POINT('',(0.00635637021762366,0.014221368576147,0.00412017214416358));
#21723=CARTESIAN_POINT('',(0.00722635013327136,0.0142730999094807,0.00227137089460337));
#21724=CARTESIAN_POINT('',(0.00746990588720064,0.0142989655761476,0.00125688808367749));
#21725=CARTESIAN_POINT('',(0.00753408637995269,0.0143506969094813,-0.000785368631023644));
#21726=CARTESIAN_POINT('',(0.00735471111877547,0.0143765625761482,-0.00181314253479889));
#21727=CARTESIAN_POINT('',(0.00660253514414939,0.014428293909482,-0.00371292218641982));
#21728=CARTESIAN_POINT('',(0.00602973443070055,0.0144541595761489,-0.0045849279342655));
#21729=CARTESIAN_POINT('',(0.00458492794137336,0.0145058909094827,-0.00602973443784537));
#21730=CARTESIAN_POINT('',(0.003712922165495,0.0145317565761496,-0.00660253519357956));
#21731=CARTESIAN_POINT('',(0.0018131425556753,0.0145834879094833,-0.00735471106936446));
#21732=CARTESIAN_POINT('',(0.000785368721733948,0.0146093535761501,-0.00753408618941518));
#21733=CARTESIAN_POINT('',(-0.00125688817443926,0.0146610849094837,-0.00746990607773653));
#21734=CARTESIAN_POINT('',(-0.00227137123667111,0.0146869505761505,-0.00722635084600715));
#21735=CARTESIAN_POINT('',(-0.00412017180214157,0.0147386819094839,-0.00635636950486635));
#21736=CARTESIAN_POINT('',(-0.00495448930538018,0.0147645475761505,-0.00572994339545493));
#21737=CARTESIAN_POINT('',(-0.00630572762017624,0.0148162789094838,-0.00419727320016948));
#21738=CARTESIAN_POINT('',(-0.00682264843173369,0.0148421445761503,-0.00329102911429546));
#21739=CARTESIAN_POINT('',(-0.00745404086872699,0.0148938759094832,-0.00134774843643272));
#21740=CARTESIAN_POINT('',(-0.00756851249416284,0.0149197415761496,-0.000310711844443995));
#21741=CARTESIAN_POINT('',(-0.00740584183095092,0.0149635143620007,0.0014104722978844));
#21742=CARTESIAN_POINT('',(-0.00723835710101072,0.0149814214811855,0.00210502142722371));
#21743=CARTESIAN_POINT('',(-0.00697825059943558,0.0149993286003702,0.00276288486472603));
#21744=CARTESIAN_POINT('',(-0.00697824898150667,0.0138052138913639,0.00276288964191574));
#21745=CARTESIAN_POINT('',(-0.00671752011891237,0.0138231209680448,0.003420504889425));
#21746=CARTESIAN_POINT('',(-0.0063641602726322,0.0138410280447258,0.00404145900200117));
#21747=CARTESIAN_POINT('',(-0.0053045114520012,0.0138848007880731,0.00540750269577185));
#21748=CARTESIAN_POINT('',(-0.00451116480340563,0.0139106664547395,0.0060851086400904));
#21749=CARTESIAN_POINT('',(-0.00272063229996765,0.0139623977880724,0.00706948145674051));
#21750=CARTESIAN_POINT('',(-0.00172344644512525,0.013988263454739,0.00737624832907208));
#21751=CARTESIAN_POINT('',(0.000310748910628582,0.0140399947880721,0.00756853054637559));
#21752=CARTESIAN_POINT('',(0.00134775841154001,0.0140658604547388,0.00745404589134754));
#21753=CARTESIAN_POINT('',(0.0032910192978751,0.0141175917880722,0.00682264389734765));
#21754=CARTESIAN_POINT('',(0.00419727068329875,0.014143457454739,0.00630572655837582));
#21755=CARTESIAN_POINT('',(0.00572994625186393,0.0141951887880726,0.00495449075223677));
#21756=CARTESIAN_POINT('',(0.00635637043500547,0.0142210544547394,0.00412017228506955));
#21757=CARTESIAN_POINT('',(0.00722635038040566,0.0142727857880731,0.0022713709722821));
#21758=CARTESIAN_POINT('',(0.00746990614266431,0.01429865145474,0.00125688812666186));
#21759=CARTESIAN_POINT('',(0.00753408663761128,0.0143503827880738,-0.000785368657882504));
#21760=CARTESIAN_POINT('',(0.00735471137029959,0.0143762484547407,-0.00181314259680664));
#21761=CARTESIAN_POINT('',(0.00660253536994981,0.0144279797880745,-0.00371292231339822));
#21762=CARTESIAN_POINT('',(0.00602973463691173,0.0144538454547414,-0.00458492809106567));
#21763=CARTESIAN_POINT('',(0.00458492809817353,0.0145055767880752,-0.00602973464405655));
#21764=CARTESIAN_POINT('',(0.00371292229247341,0.014531442454742,-0.00660253541937998));
#21765=CARTESIAN_POINT('',(0.00181314261768305,0.0145831737880757,-0.00735471132088858));
#21766=CARTESIAN_POINT('',(0.000785368748592811,0.0146090394547426,-0.00753408644707376));
#21767=CARTESIAN_POINT('',(-0.00125688821742364,0.0146607707880762,-0.00746990633320021));
#21768=CARTESIAN_POINT('',(-0.00227137131434984,0.0146866364547429,-0.00722635109314147));
#21769=CARTESIAN_POINT('',(-0.00412017194304752,0.0147383677880763,-0.00635636972224814));
#21770=CARTESIAN_POINT('',(-0.004954489474819,0.014764233454743,-0.00572994359141354));
#21771=CARTESIAN_POINT('',(-0.00630572783582612,0.0148159647880762,-0.00419727334371223));
#21772=CARTESIAN_POINT('',(-0.00682264866506177,0.0148418304547427,-0.00329102922684552));
#21773=CARTESIAN_POINT('',(-0.00745404112364809,0.0148935617880757,-0.00134774848252443));
#21774=CARTESIAN_POINT('',(-0.00756851275299877,0.0149194274547421,-0.000310711855070044));
#21775=CARTESIAN_POINT('',(-0.00740584208422367,0.0149632002405932,0.00141047234612122));
#21776=CARTESIAN_POINT('',(-0.00723835734855565,0.0149811073597779,0.00210502149921344));
#21777=CARTESIAN_POINT('',(-0.00697825083808511,0.0149990144789627,0.00276288495921406));
#21778=CARTESIAN_POINT('',(-0.00697824898150667,0.0136799987751258,0.00276288964191574));
#21779=CARTESIAN_POINT('',(-0.00671752011891237,0.0136979058518067,0.003420504889425));
#21780=CARTESIAN_POINT('',(-0.00636416027263221,0.0137158129284877,0.00404145900200118));
#21781=CARTESIAN_POINT('',(-0.00530451145200121,0.013759585671835,0.00540750269577187));
#21782=CARTESIAN_POINT('',(-0.00451116480340563,0.0137854513385014,0.00608510864009041));
#21783=CARTESIAN_POINT('',(-0.00272063229996765,0.0138371826718343,0.00706948145674051));
#21784=CARTESIAN_POINT('',(-0.00172344644512526,0.0138630483385009,0.00737624832907209));
#21785=CARTESIAN_POINT('',(0.000310748910628586,0.0139147796718341,0.00756853054637561));
#21786=CARTESIAN_POINT('',(0.00134775841154003,0.0139406453385007,0.00745404589134754));
#21787=CARTESIAN_POINT('',(0.00329101929787511,0.0139923766718341,0.00682264389734765));
#21788=CARTESIAN_POINT('',(0.00419727068329876,0.0140182423385009,0.00630572655837583));
#21789=CARTESIAN_POINT('',(0.00572994625186394,0.0140699736718345,0.00495449075223678));
#21790=CARTESIAN_POINT('',(0.00635637043500548,0.0140958393385013,0.00412017228506955));
#21791=CARTESIAN_POINT('',(0.00722635038040566,0.014147570671835,0.00227137097228209));
#21792=CARTESIAN_POINT('',(0.00746990614266432,0.0141734363385019,0.00125688812666186));
#21793=CARTESIAN_POINT('',(0.00753408663761128,0.0142251676718357,-0.000785368657882517));
#21794=CARTESIAN_POINT('',(0.00735471137029959,0.0142510333385026,-0.00181314259680666));
#21795=CARTESIAN_POINT('',(0.00660253536994981,0.0143027646718364,-0.00371292231339824));
#21796=CARTESIAN_POINT('',(0.00602973463691173,0.0143286303385033,-0.00458492809106568));
#21797=CARTESIAN_POINT('',(0.00458492809817352,0.0143803616718371,-0.00602973464405656));
#21798=CARTESIAN_POINT('',(0.00371292229247341,0.014406227338504,-0.00660253541937999));
#21799=CARTESIAN_POINT('',(0.00181314261768303,0.0144579586718377,-0.0073547113208886));
#21800=CARTESIAN_POINT('',(0.00078536874859279,0.0144838243385045,-0.00753408644707379));
#21801=CARTESIAN_POINT('',(-0.00125688821742367,0.0145355556718381,-0.00746990633320024));
#21802=CARTESIAN_POINT('',(-0.00227137131434988,0.0145614213385048,-0.00722635109314148));
#21803=CARTESIAN_POINT('',(-0.00412017194304755,0.0146131526718383,-0.00635636972224814));
#21804=CARTESIAN_POINT('',(-0.00495448947481901,0.0146390183385049,-0.00572994359141354));
#21805=CARTESIAN_POINT('',(-0.00630572783582613,0.0146907496718381,-0.00419727334371224));
#21806=CARTESIAN_POINT('',(-0.00682264866506178,0.0147166153385046,-0.00329102922684553));
#21807=CARTESIAN_POINT('',(-0.00745404112364811,0.0147683466718376,-0.00134774848252442));
#21808=CARTESIAN_POINT('',(-0.00756851275299878,0.014794212338504,-0.000310711855070028));
#21809=CARTESIAN_POINT('',(-0.00740584208422367,0.0148379851243551,0.00141047234612124));
#21810=CARTESIAN_POINT('',(-0.00723835734855564,0.0148558922435399,0.00210502149921347));
#21811=CARTESIAN_POINT('',(-0.0069782508380851,0.0148737993627246,0.00276288495921409));
#21812=CARTESIAN_POINT('',(-0.00694051807885813,0.0135550977802952,0.00274795089146644));
#21813=CARTESIAN_POINT('',(-0.00668119895893111,0.0135730048569762,0.00340201045947075));
#21814=CARTESIAN_POINT('',(-0.00632974970454803,0.0135909119336571,0.00401960711672642));
#21815=CARTESIAN_POINT('',(-0.00527583033074515,0.0136346846770044,0.00537826470808661));
#21816=CARTESIAN_POINT('',(-0.00448677325181727,0.0136605503436708,0.00605220688460511));
#21817=CARTESIAN_POINT('',(-0.00270592203200149,0.0137122816770038,0.00703125726649926));
#21818=CARTESIAN_POINT('',(-0.00171412789111359,0.0137381473436703,0.00733636547187492));
#21819=CARTESIAN_POINT('',(0.000309068713070982,0.0137898786770035,0.00752760803272001));
#21820=CARTESIAN_POINT('',(0.00134047117636765,0.0138157443436701,0.00741374238818944));
#21821=CARTESIAN_POINT('',(0.00327322498742965,0.0138674756770036,0.00678575434047189));
#21822=CARTESIAN_POINT('',(0.00417457633519497,0.0138933413436703,0.00627163193728492));
#21823=CARTESIAN_POINT('',(0.00569896483449356,0.0139450726770039,0.00492770216834686));
#21824=CARTESIAN_POINT('',(0.00632200198602682,0.0139709383436707,0.00409789480259576));
#21825=CARTESIAN_POINT('',(0.00718727801090008,0.0140226696770045,0.00225908982879452));
#21826=CARTESIAN_POINT('',(0.00742951688424009,0.0140485353436713,0.00125009222074437));
#21827=CARTESIAN_POINT('',(0.00749335035975379,0.0141002666770051,-0.000781122224650859));
#21828=CARTESIAN_POINT('',(0.00731494496192747,0.014126132343672,-0.00180333906199593));
#21829=CARTESIAN_POINT('',(0.00656683592443887,0.0141778636770058,-0.00369284680294858));
#21830=CARTESIAN_POINT('',(0.00599713228477658,0.0142037293436727,-0.00456013770655617));
#21831=CARTESIAN_POINT('',(0.0045601377136256,0.0142554606770065,-0.00599713229188276));
#21832=CARTESIAN_POINT('',(0.0036928467821369,0.0142813263436734,-0.00656683597360176));
#21833=CARTESIAN_POINT('',(0.00180333908275946,0.0143330576770071,-0.00731494491278364));
#21834=CARTESIAN_POINT('',(0.000781122314870693,0.0143589233436739,-0.00749335017024651));
#21835=CARTESIAN_POINT('',(-0.0012500923110154,0.0144106546770075,-0.00742951707374578));
#21836=CARTESIAN_POINT('',(-0.00225909016901274,0.0144365203436743,-0.00718727871978218));
#21837=CARTESIAN_POINT('',(-0.00409789446242304,0.0144882516770077,-0.00632200127712331));
#21838=CARTESIAN_POINT('',(-0.00492770089783601,0.0145141173436743,-0.00569896218842803));
#21839=CARTESIAN_POINT('',(-0.00627163320782814,0.0145658486770075,-0.00417457898122379));
#21840=CARTESIAN_POINT('',(-0.00678575908240731,0.0145917143436741,-0.00327323486271482));
#21841=CARTESIAN_POINT('',(-0.00741373764626861,0.014643445677007,-0.00134046130103755));
#21842=CARTESIAN_POINT('',(-0.00752759033555073,0.0146693113436734,-0.000309031857869243));
#21843=CARTESIAN_POINT('',(-0.0073657992156687,0.0147130841295245,0.00140284602110459));
#21844=CARTESIAN_POINT('',(-0.0071992200582157,0.0147309912487093,0.00209363979565566));
#21845=CARTESIAN_POINT('',(-0.00694051992539818,0.014748898367894,0.00274794623408381));
#21846=CARTESIAN_POINT('',(-0.00680400639064949,0.0133530037254307,0.00269390198459144));
#21847=CARTESIAN_POINT('',(-0.00654978776760812,0.0133709108021116,0.00333509698329374));
#21848=CARTESIAN_POINT('',(-0.00620525109964731,0.0133888178787926,0.00394054625308408));
#21849=CARTESIAN_POINT('',(-0.00517206105920528,0.0134325906221399,0.00527248067487872));
#21850=CARTESIAN_POINT('',(-0.00439852378913224,0.0134584562888063,0.00593316721496976));
#21851=CARTESIAN_POINT('',(-0.00265269978251629,0.0135101876221392,0.00689296084701396));
#21852=CARTESIAN_POINT('',(-0.00168041304597339,0.0135360532888058,0.00719206793896711));
#21853=CARTESIAN_POINT('',(0.000302989701199763,0.013587784622139,0.007379548987409));
#21854=CARTESIAN_POINT('',(0.00131410571183001,0.0136136502888056,0.00726792294389772));
#21855=CARTESIAN_POINT('',(0.00320884456743163,0.013665381622139,0.00665228666986547));
#21856=CARTESIAN_POINT('',(0.004092467412403,0.0136912472888058,0.00614827643934451));
#21857=CARTESIAN_POINT('',(0.0055868730134279,0.0137429786221394,0.00483078016132269));
#21858=CARTESIAN_POINT('',(0.00619765576948143,0.0137688442888062,0.00401729411382185));
#21859=CARTESIAN_POINT('',(0.00704591285000791,0.0138205756221399,0.00221465623423577));
#21860=CARTESIAN_POINT('',(0.00728338717448087,0.0138464412888068,0.00122550440215052));
#21861=CARTESIAN_POINT('',(0.00734596512189023,0.0138981726221406,-0.000765758484887794));
#21862=CARTESIAN_POINT('',(0.00717106874482664,0.0139240382888075,-0.00176786953984086));
#21863=CARTESIAN_POINT('',(0.00643767411720073,0.0139757696221413,-0.00362021292380028));
#21864=CARTESIAN_POINT('',(0.0058791758666384,0.0140016352888082,-0.00447044525280663));
#21865=CARTESIAN_POINT('',(0.00447044525973701,0.014053366622142,-0.00587917587360481));
#21866=CARTESIAN_POINT('',(0.00362021290339795,0.0140792322888089,-0.00643767416539665));
#21867=CARTESIAN_POINT('',(0.00176786956019601,0.0141309636221426,-0.0071710686966494));
#21868=CARTESIAN_POINT('',(0.000765758573333131,0.0141568292888094,-0.00734596493611032));
#21869=CARTESIAN_POINT('',(-0.00122550449064601,0.014208560622143,-0.00728338736025919));
#21870=CARTESIAN_POINT('',(-0.00221465656776228,0.0142344262888097,-0.00704591354494715));
#21871=CARTESIAN_POINT('',(-0.00401729378033991,0.0142861576221432,-0.00619765507452121));
#21872=CARTESIAN_POINT('',(-0.00483077891580127,0.0143120232888098,-0.00558687041940731));
#21873=CARTESIAN_POINT('',(-0.00614827768489766,0.014363754622143,-0.00409247000638758));
#21874=CARTESIAN_POINT('',(-0.0066522913185327,0.0143896202888096,-0.00320885424848175));
#21875=CARTESIAN_POINT('',(-0.0072679182952448,0.0144413516221425,-0.00131409603073584));
#21876=CARTESIAN_POINT('',(-0.00737953163832187,0.0144672172888089,-0.000302953570895764));
#21877=CARTESIAN_POINT('',(-0.00722092275622978,0.01451099007466,0.00137525371798514));
#21878=CARTESIAN_POINT('',(-0.00705762001153818,0.0145288971938448,0.00205246040533372));
#21879=CARTESIAN_POINT('',(-0.00680400820087031,0.0145468043130295,0.00269389741881393));
#21880=CARTESIAN_POINT('',(-0.00670522560508939,0.0132758106653968,0.00265479182816572));
#21881=CARTESIAN_POINT('',(-0.00645469773626639,0.0132937177420777,0.00328667793707097));
#21882=CARTESIAN_POINT('',(-0.00611516306283078,0.0133116248187586,0.0038833372747165));
#21883=CARTESIAN_POINT('',(-0.00509697290892147,0.0133553975621059,0.00519593462935609));
#21884=CARTESIAN_POINT('',(-0.00433466587803557,0.0133812632287723,0.00584702930081972));
#21885=CARTESIAN_POINT('',(-0.00261418780099727,0.0134329945621053,0.00679288861776991));
#21886=CARTESIAN_POINT('',(-0.00165601675484486,0.0134588602287718,0.00708765326325648));
#21887=CARTESIAN_POINT('',(0.000298590886886145,0.013510591562105,0.00727241245575358));
#21888=CARTESIAN_POINT('',(0.00129502748246474,0.0135364572287717,0.00716240700276411));
#21889=CARTESIAN_POINT('',(0.00316225845787907,0.0135881885621051,0.00655570855613482));
#21890=CARTESIAN_POINT('',(0.00403305283771479,0.0136140542287718,0.00605901556249499));
#21891=CARTESIAN_POINT('',(0.00550576260973261,0.0136657855621054,0.00476064673818844));
#21892=CARTESIAN_POINT('',(0.00610767800191469,0.0136916512287723,0.00395897090752172));
#21893=CARTESIAN_POINT('',(0.00694362005862132,0.013743382562106,0.00218250378316458));
#21894=CARTESIAN_POINT('',(0.00717764672314586,0.0137692482287729,0.00120771248947416));
#21895=CARTESIAN_POINT('',(0.00723931616188417,0.0138209795621066,-0.000754641178356387));
#21896=CARTESIAN_POINT('',(0.00706695893609794,0.0138468452287735,-0.00174220355249652));
#21897=CARTESIAN_POINT('',(0.00634421175547354,0.0138985765621073,-0.00356765455510162));
#21898=CARTESIAN_POINT('',(0.00579382180063537,0.0139244422287742,-0.00440554318356659));
#21899=CARTESIAN_POINT('',(0.00440554319039635,0.013976173562108,-0.00579382180750065));
#21900=CARTESIAN_POINT('',(0.00356765453499548,0.0140020392287749,-0.00634421180296975));
#21901=CARTESIAN_POINT('',(0.00174220357255614,0.0140537705621086,-0.00706695888862013));
#21902=CARTESIAN_POINT('',(0.000754641265517664,0.0140796362287754,-0.00723931597880142));
#21903=CARTESIAN_POINT('',(-0.00120771257668489,0.014131367562109,-0.00717764690622705));
#21904=CARTESIAN_POINT('',(-0.00218250411184896,0.0141572332287758,-0.0069436207434714));
#21905=CARTESIAN_POINT('',(-0.00395897057888128,0.0142089645621092,-0.00610767731704393));
#21906=CARTESIAN_POINT('',(-0.00476064551074954,0.0142348302287759,-0.0055057600533721));
#21907=CARTESIAN_POINT('',(-0.00605901678996516,0.0142865615621091,-0.00403305539403983));
#21908=CARTESIAN_POINT('',(-0.00655571313731254,0.0143124272287756,-0.00316226799837939));
#21909=CARTESIAN_POINT('',(-0.00716240242160049,0.0143641585621085,-0.00129501794192101));
#21910=CARTESIAN_POINT('',(-0.00727239535854106,0.0143900242287749,-0.000298555281123069));
#21911=CARTESIAN_POINT('',(-0.00711608916534582,0.014433797014626,0.00135528773988235));
#21912=CARTESIAN_POINT('',(-0.0069551572552006,0.0144517041338108,0.00202266271856957));
#21913=CARTESIAN_POINT('',(-0.00670522738902937,0.0144696112529955,0.00265478732867433));
#21914=CARTESIAN_POINT('',(-0.00648434505370619,0.0131986176053628,0.00256733885978718));
#21915=CARTESIAN_POINT('',(-0.00624206996220368,0.0132165246820437,0.00317840965831116));
#21916=CARTESIAN_POINT('',(-0.00591372008854949,0.0132344317587247,0.00375541411016327));
#21917=CARTESIAN_POINT('',(-0.00492907070058216,0.013278204502072,0.00502477246815869));
#21918=CARTESIAN_POINT('',(-0.00419187524792228,0.0133040701687384,0.00565441906934018));
#21919=CARTESIAN_POINT('',(-0.00252807239237249,0.0133558015020713,0.00656912031052029));
#21920=CARTESIAN_POINT('',(-0.00160146498948258,0.0133816671687379,0.0068541749505189));
#21921=CARTESIAN_POINT('',(0.0002887548390605,0.0134333985020711,0.00703284788809851));
#21922=CARTESIAN_POINT('',(0.00125236726471367,0.0134592641687377,0.0069264661856795));
#21923=CARTESIAN_POINT('',(0.00305808875011229,0.0135109955020711,0.00633975332869436));
#21924=CARTESIAN_POINT('',(0.00390019780985773,0.0135368611687379,0.00585942217412824));
#21925=CARTESIAN_POINT('',(0.00532439423338749,0.0135885925020715,0.00460382363656549));
#21926=CARTESIAN_POINT('',(0.0059064815971718,0.0136144581687383,0.00382855625356888));
#21927=CARTESIAN_POINT('',(0.00671488642347269,0.013666189502072,0.00211060871692618));
#21928=CARTESIAN_POINT('',(0.00694120388598927,0.0136920551687389,0.00116792856328009));
#21929=CARTESIAN_POINT('',(0.00700084183758095,0.0137437865020727,-0.000729782125225456));
#21930=CARTESIAN_POINT('',(0.00683416232665604,0.0137696521687396,-0.00168481266008492));
#21931=CARTESIAN_POINT('',(0.00613522356131386,0.0138213835020734,-0.00345013046990492));
#21932=CARTESIAN_POINT('',(0.0056029643068966,0.0138472491687403,-0.00426041774486545));
#21933=CARTESIAN_POINT('',(0.00426041775147022,0.0138989805020741,-0.00560296431353573));
#21934=CARTESIAN_POINT('',(0.00345013045046111,0.0139248461687409,-0.00613522360724548));
#21935=CARTESIAN_POINT('',(0.00168481267948375,0.0139765775020746,-0.00683416228074223));
#21936=CARTESIAN_POINT('',(0.000729782209515497,0.0140024431687415,-0.00700084166052923));
#21937=CARTESIAN_POINT('',(-0.00116792864761797,0.0140541745020751,-0.00694120406303949));
#21938=CARTESIAN_POINT('',(-0.00211060903478319,0.0140800401687418,-0.00671488708576275));
#21939=CARTESIAN_POINT('',(-0.00382855593575437,0.0141317715020752,-0.00590648093486174));
#21940=CARTESIAN_POINT('',(-0.00460382244956033,0.0141576371687419,-0.00532439176123747));
#21941=CARTESIAN_POINT('',(-0.00585942336116364,0.0142093685020751,-0.00390020028197345));
#21942=CARTESIAN_POINT('',(-0.00633975775896097,0.0142352341687416,-0.0030580979763337));
#21943=CARTESIAN_POINT('',(-0.00692646175542652,0.0142869655020746,-0.00125235803845027));
#21944=CARTESIAN_POINT('',(-0.00703283135409474,0.014312831168741,-0.000288720406206587));
#21945=CARTESIAN_POINT('',(-0.0068816741298039,0.0143566039545921,0.00131064245560722));
#21946=CARTESIAN_POINT('',(-0.00672604356686779,0.0143745110737768,0.00195603306539268));
#21947=CARTESIAN_POINT('',(-0.00648434677888041,0.0143924181929616,0.00256733450851603));
#21948=CARTESIAN_POINT('',(-0.00636224528788308,0.0131986176053628,0.00251899604783435));
#21949=CARTESIAN_POINT('',(-0.0061245322194827,0.0132165246820437,0.00311856042577412));
#21950=CARTESIAN_POINT('',(-0.00580236515108474,0.0132344317587247,0.00368469992397763));
#21951=CARTESIAN_POINT('',(-0.00483625664252665,0.013278204502072,0.00493015635248392));
#21952=CARTESIAN_POINT('',(-0.00411294252890567,0.0133040701687384,0.00554794675201068));
#21953=CARTESIAN_POINT('',(-0.00248046896526676,0.0133558015020713,0.0064454242325147));
#21954=CARTESIAN_POINT('',(-0.00157130951524884,0.0133816671687378,0.00672511131349196));
#21955=CARTESIAN_POINT('',(0.000283317605548472,0.013433398502071,0.00690041985209886));
#21956=CARTESIAN_POINT('',(0.00122878527632786,0.0134592641687377,0.00679604130972849));
#21957=CARTESIAN_POINT('',(0.00300050515189806,0.0135109955020711,0.00622037621498456));
#21958=CARTESIAN_POINT('',(0.00382675735668888,0.0135368611687379,0.00574908966261099));
#21959=CARTESIAN_POINT('',(0.00522413626073766,0.0135885925020715,0.0045171339580768));
#21960=CARTESIAN_POINT('',(0.00579526295999564,0.0136144581687383,0.00375646480591617));
#21961=CARTESIAN_POINT('',(0.00658844557971066,0.013666189502072,0.00207086610175896));
#21962=CARTESIAN_POINT('',(0.0068105015001677,0.0136920551687389,0.00114593654976238));
#21963=CARTESIAN_POINT('',(0.0068690164732838,0.0137437865020727,-0.000716040378625932));
#21964=CARTESIAN_POINT('',(0.00670547552594286,0.0137696521687396,-0.00165308775501766));
#21965=CARTESIAN_POINT('',(0.00601969772888139,0.0138213835020734,-0.00338516475340688));
#21966=CARTESIAN_POINT('',(0.00549746087916086,0.0138472491687403,-0.00418019437540436));
#21967=CARTESIAN_POINT('',(0.00418019438188476,0.0138989805020741,-0.00549746088567498));
#21968=CARTESIAN_POINT('',(0.00338516473432919,0.0139248461687409,-0.00601969777394812));
#21969=CARTESIAN_POINT('',(0.0016530877740512,0.0139765775020746,-0.0067054754808936));
#21970=CARTESIAN_POINT('',(0.000716040461328796,0.0140024431687415,-0.00686901629956595));
#21971=CARTESIAN_POINT('',(-0.00114593663251218,0.0140541745020751,-0.00681050167388407));
#21972=CARTESIAN_POINT('',(-0.00207086641363074,0.0140800401687418,-0.00658844622952984));
#21973=CARTESIAN_POINT('',(-0.00375646449408609,0.0141317715020752,-0.00579526231015683));
#21974=CARTESIAN_POINT('',(-0.00451713279342287,0.0141576371687419,-0.00522413383513805));
#21975=CARTESIAN_POINT('',(-0.0057490908272946,0.0142093685020751,-0.00382675978225482));
#21976=CARTESIAN_POINT('',(-0.00622038056182956,0.0142352341687416,-0.00300051420439038));
#21977=CARTESIAN_POINT('',(-0.00679603696289687,0.0142869655020746,-0.00122877622379436));
#21978=CARTESIAN_POINT('',(-0.00690040362942923,0.014312831168741,-0.0002832838210628));
#21979=CARTESIAN_POINT('',(-0.00675209268514594,0.0143566039545921,0.00128596314943489));
#21980=CARTESIAN_POINT('',(-0.00659939263487256,0.0143745110737768,0.00191920109897995));
#21981=CARTESIAN_POINT('',(-0.00636224698057239,0.0143924181929616,0.00251899177849733));
#21982=CARTESIAN_POINT('',(-0.00614136473649988,0.0132758106653968,0.00243154307945581));
#21983=CARTESIAN_POINT('',(-0.00591190444542,0.0132937177420777,0.0030102921470143));
#21984=CARTESIAN_POINT('',(-0.00560092217680345,0.0133116248187586,0.00355677675942441));
#21985=CARTESIAN_POINT('',(-0.00466835443418733,0.0133553975621059,0.00475899419128651));
#21986=CARTESIAN_POINT('',(-0.00397015189879237,0.0133812632287723,0.00535533652053114));
#21987=CARTESIAN_POINT('',(-0.00239435355664199,0.0134329945621053,0.00622165592526508));
#21988=CARTESIAN_POINT('',(-0.00151675774988656,0.0134588602287718,0.00649163300075439));
#21989=CARTESIAN_POINT('',(0.000273481557722826,0.013510591562105,0.00666085528444379));
#21990=CARTESIAN_POINT('',(0.00118612505857678,0.0135364572287717,0.00656010049264387));
#21991=CARTESIAN_POINT('',(0.00289633544413128,0.0135881885621051,0.0060044209875441));
#21992=CARTESIAN_POINT('',(0.00369390232883181,0.0136140542287718,0.00554949627424424));
#21993=CARTESIAN_POINT('',(0.00504276788439255,0.0136657855621054,0.00436031085645385));
#21994=CARTESIAN_POINT('',(0.00559406655525274,0.0136916512287723,0.00362605015196332));
#21995=CARTESIAN_POINT('',(0.00635971194456203,0.013743382562106,0.00199897103552055));
#21996=CARTESIAN_POINT('',(0.00657405866301112,0.0137692482287729,0.00110615262356831));
#21997=CARTESIAN_POINT('',(0.00663054214898058,0.0138209795621066,-0.000691181325494998));
#21998=CARTESIAN_POINT('',(0.00647267891650096,0.0138468452287735,-0.00159569686260606));
#21999=CARTESIAN_POINT('',(0.00581070953472172,0.0138985765621073,-0.00326764066821018));
#22000=CARTESIAN_POINT('',(0.00530660338542209,0.0139244422287742,-0.00403506893670322));
#22001=CARTESIAN_POINT('',(0.00403506894295864,0.013976173562108,-0.00530660339171005));
#22002=CARTESIAN_POINT('',(0.00326764064979481,0.0140020392287749,-0.00581070957822385));
#22003=CARTESIAN_POINT('',(0.0015956968809788,0.0140537705621086,-0.0064726788730157));
#22004=CARTESIAN_POINT('',(0.00069118140532663,0.0140796362287754,-0.00663054198129377));
#22005=CARTESIAN_POINT('',(-0.00110615270344525,0.014131367562109,-0.00657405883069651));
#22006=CARTESIAN_POINT('',(-0.00199897133656496,0.0141572332287758,-0.00635971257182118));
#22007=CARTESIAN_POINT('',(-0.00362604985095917,0.0142089645621092,-0.00559406592797464));
#22008=CARTESIAN_POINT('',(-0.00436030973223366,0.0142348302287759,-0.00504276554300342));
#22009=CARTESIAN_POINT('',(-0.00554949739849307,0.0142865615621091,-0.00369390467018844));
#22010=CARTESIAN_POINT('',(-0.00600442518347799,0.0143124272287756,-0.00289634418234468));
#22011=CARTESIAN_POINT('',(-0.00656009629672291,0.0143641585621085,-0.00118611632032362));
#22012=CARTESIAN_POINT('',(-0.00666083962498291,0.0143900242287749,-0.00027344894614632));
#22013=CARTESIAN_POINT('',(-0.00651767764960402,0.014433797014626,0.00124131786515975));
#22014=CARTESIAN_POINT('',(-0.00637027894653976,0.0144517041338108,0.00185257144580306));
#22015=CARTESIAN_POINT('',(-0.00614136637042343,0.0144696112529955,0.00243153895833903));
#22016=CARTESIAN_POINT('',(-0.00604258395093978,0.0133530037254307,0.0023924329230301));
#22017=CARTESIAN_POINT('',(-0.00581681441407825,0.0133709108021116,0.00296187310079154));
#22018=CARTESIAN_POINT('',(-0.0055108341399869,0.0133888178787926,0.00349956778105683));
#22019=CARTESIAN_POINT('',(-0.00459326628390352,0.0134325906221399,0.00468244814576388));
#22020=CARTESIAN_POINT('',(-0.00390629398769571,0.0134584562888063,0.0052691986063811));
#22021=CARTESIAN_POINT('',(-0.00235584157512295,0.0135101876221392,0.00612158369602103));
#22022=CARTESIAN_POINT('',(-0.00149236145875803,0.0135360532888058,0.00638721832504376));
#22023=CARTESIAN_POINT('',(0.000269082743409209,0.013587784622139,0.00655371875278837));
#22024=CARTESIAN_POINT('',(0.00116704682921151,0.0136136502888056,0.00645458455151027));
#22025=CARTESIAN_POINT('',(0.00284974933457871,0.013665381622139,0.00590784287381344));
#22026=CARTESIAN_POINT('',(0.00363448775414361,0.0136912472888058,0.00546023539739472));
#22027=CARTESIAN_POINT('',(0.00496165748069726,0.0137429786221394,0.00429017743331959));
#22028=CARTESIAN_POINT('',(0.00550408878768601,0.0137688442888062,0.00356772694566319));
#22029=CARTESIAN_POINT('',(0.00625741915317544,0.0138205756221399,0.00196681858444937));
#22030=CARTESIAN_POINT('',(0.00646831821167611,0.0138464412888068,0.00108836071089196));
#22031=CARTESIAN_POINT('',(0.00652389318897452,0.0138981726221406,-0.000680064018963589));
#22032=CARTESIAN_POINT('',(0.00636856910777225,0.0139240382888075,-0.00157003087526173));
#22033=CARTESIAN_POINT('',(0.00571724717299453,0.0139757696221413,-0.00321508229951151));
#22034=CARTESIAN_POINT('',(0.00522124931941907,0.0140016352888082,-0.00397016686746317));
#22035=CARTESIAN_POINT('',(0.00397016687361797,0.014053366622142,-0.00522124932560588));
#22036=CARTESIAN_POINT('',(0.00321508228139235,0.0140792322888089,-0.00571724721579695));
#22037=CARTESIAN_POINT('',(0.00157003089333894,0.0141309636221426,-0.00636856906498643));
#22038=CARTESIAN_POINT('',(0.000680064097511164,0.0141568292888094,-0.00652389302398486));
#22039=CARTESIAN_POINT('',(-0.00108836078948412,0.014208560622143,-0.00646831837666436));
#22040=CARTESIAN_POINT('',(-0.00196681888065163,0.0142344262888097,-0.00625741977034544));
#22041=CARTESIAN_POINT('',(-0.00356772664950053,0.0142861576221432,-0.00550408817049736));
#22042=CARTESIAN_POINT('',(-0.00429017632718193,0.0143120232888098,-0.00496165517696821));
#22043=CARTESIAN_POINT('',(-0.00546023650356058,0.014363754622143,-0.00363449005784069));
#22044=CARTESIAN_POINT('',(-0.00590784700225783,0.0143896202888096,-0.00284975793224231));
#22045=CARTESIAN_POINT('',(-0.00645458042307859,0.0144413516221425,-0.00116703823150879));
#22046=CARTESIAN_POINT('',(-0.0065537033452021,0.0144672172888089,-0.000269050656373628));
#22047=CARTESIAN_POINT('',(-0.00641284405872006,0.01451099007466,0.00122135188705695));
#22048=CARTESIAN_POINT('',(-0.00626781619020218,0.0145288971938448,0.00182277375903891));
#22049=CARTESIAN_POINT('',(-0.00604258555858249,0.0145468043130295,0.00239242886819942));
#22050=CARTESIAN_POINT('',(-0.00590607226273114,0.0135550977802952,0.00233838401615509));
#22051=CARTESIAN_POINT('',(-0.00568540322275527,0.0135730048569762,0.00289495962461452));
#22052=CARTESIAN_POINT('',(-0.0053863355350862,0.0135909119336571,0.00342050691741449));
#22053=CARTESIAN_POINT('',(-0.00448949701236366,0.0136346846770044,0.004576664112556));
#22054=CARTESIAN_POINT('',(-0.00381804452501068,0.0136605503436708,0.00515015893674575));
#22055=CARTESIAN_POINT('',(-0.00230261932563777,0.0137122816770038,0.00598328727653573));
#22056=CARTESIAN_POINT('',(-0.00145864661361783,0.0137381473436703,0.00624292079213596));
#22057=CARTESIAN_POINT('',(0.000263003731537994,0.0137898786770035,0.00640565970747737));
#22058=CARTESIAN_POINT('',(0.00114068136467388,0.0138157443436702,0.00630876510721855));
#22059=CARTESIAN_POINT('',(0.0027853689145807,0.0138674756770036,0.00577437520320703));
#22060=CARTESIAN_POINT('',(0.00355237883135163,0.0138933413436703,0.00533687989945431));
#22061=CARTESIAN_POINT('',(0.00484956565963159,0.0139450726770039,0.00419325542629543));
#22062=CARTESIAN_POINT('',(0.00537974257114062,0.0139709383436707,0.00348712625688928));
#22063=CARTESIAN_POINT('',(0.00611605399228327,0.0140226696770045,0.00192238498989061));
#22064=CARTESIAN_POINT('',(0.00632218850191688,0.0140485353436713,0.0010637728922981));
#22065=CARTESIAN_POINT('',(0.00637650795111096,0.0141002666770051,-0.000664700279200532));
#22066=CARTESIAN_POINT('',(0.00622469289067143,0.014126132343672,-0.00153456135310666));
#22067=CARTESIAN_POINT('',(0.00558808536575639,0.0141778636770058,-0.00314244842036322));
#22068=CARTESIAN_POINT('',(0.00510329290128088,0.0142037293436727,-0.00388047441371363));
#22069=CARTESIAN_POINT('',(0.00388047441972938,0.0142554606770065,-0.00510329290732795));
#22070=CARTESIAN_POINT('',(0.00314244840265338,0.0142813263436734,-0.00558808540759184));
#22071=CARTESIAN_POINT('',(0.00153456137077549,0.0143330576770071,-0.00622469284885221));
#22072=CARTESIAN_POINT('',(0.000664700355973588,0.0143589233436739,-0.00637650778984869));
#22073=CARTESIAN_POINT('',(-0.00106377296911475,0.0144106546770075,-0.00632218866317778));
#22074=CARTESIAN_POINT('',(-0.00192238527940119,0.0144365203436743,-0.00611605459551041));
#22075=CARTESIAN_POINT('',(-0.00348712596741742,0.0144882516770077,-0.00537974196789526));
#22076=CARTESIAN_POINT('',(-0.0041932543451472,0.0145141173436743,-0.00484956340794749));
#22077=CARTESIAN_POINT('',(-0.0053368809806301,0.0145658486770075,-0.00355238108300448));
#22078=CARTESIAN_POINT('',(-0.00577437923838321,0.0145917143436741,-0.00278537731800925));
#22079=CARTESIAN_POINT('',(-0.00630876107205479,0.014643445677007,-0.00114067296120708));
#22080=CARTESIAN_POINT('',(-0.00640564464797325,0.0146693113436734,-0.00026297236940014));
#22081=CARTESIAN_POINT('',(-0.00626796759928114,0.0147130841295245,0.00119375958393752));
#22082=CARTESIAN_POINT('',(-0.00612621614352466,0.0147309912487093,0.00178159436871697));
#22083=CARTESIAN_POINT('',(-0.00590607383405462,0.014748898367894,0.00233838005292956));
#22084=CARTESIAN_POINT('',(-0.00586834136008259,0.0136799987751258,0.00232344526570579));
#22085=CARTESIAN_POINT('',(-0.00564908206277401,0.0136979058518067,0.00287646519466028));
#22086=CARTESIAN_POINT('',(-0.00535192496700203,0.0137158129284877,0.00339865503213973));
#22087=CARTESIAN_POINT('',(-0.00446081589110761,0.013759585671835,0.00454742612487075));
#22088=CARTESIAN_POINT('',(-0.00379365297342232,0.0137854513385014,0.00511725718126046));
#22089=CARTESIAN_POINT('',(-0.00228790905767161,0.0138371826718343,0.00594506308629448));
#22090=CARTESIAN_POINT('',(-0.00144932805960617,0.0138630483385009,0.00620303793493879));
#22091=CARTESIAN_POINT('',(0.000261323533980394,0.0139147796718341,0.00636473719382177));
#22092=CARTESIAN_POINT('',(0.00113339412950152,0.0139406453385007,0.00626846160406045));
#22093=CARTESIAN_POINT('',(0.00276757460413525,0.0139923766718341,0.00573748564633127));
#22094=CARTESIAN_POINT('',(0.00352968448324786,0.0140182423385009,0.00530278527836341));
#22095=CARTESIAN_POINT('',(0.00481858424226123,0.0140699736718345,0.00416646684240553));
#22096=CARTESIAN_POINT('',(0.00534537412216198,0.0140958393385013,0.0034648487744155));
#22097=CARTESIAN_POINT('',(0.00607698162277769,0.014147570671835,0.00191010384640304));
#22098=CARTESIAN_POINT('',(0.00628179924349266,0.0141734363385019,0.00105697698638061));
#22099=CARTESIAN_POINT('',(0.00633577167325347,0.0142251676718357,-0.000660453845968885));
#22100=CARTESIAN_POINT('',(0.00618492648229931,0.0142510333385026,-0.00152475781829594));
#22101=CARTESIAN_POINT('',(0.00555238592024544,0.0143027646718364,-0.00312237290991358));
#22102=CARTESIAN_POINT('',(0.00507069054914573,0.0143286303385033,-0.00385568402920415));
#22103=CARTESIAN_POINT('',(0.00385568403518145,0.0143803616718371,-0.00507069055515418));
#22104=CARTESIAN_POINT('',(0.00312237289231687,0.014406227338504,-0.00555238596181364));
#22105=CARTESIAN_POINT('',(0.00152475783585189,0.0144579586718377,-0.00618492644074726));
#22106=CARTESIAN_POINT('',(0.000660453922251477,0.0144838243385045,-0.00633577151302142));
#22107=CARTESIAN_POINT('',(-0.00105697706270651,0.0145355556718381,-0.00628179940372335));
#22108=CARTESIAN_POINT('',(-0.00191010413406409,0.0145614213385048,-0.00607698222215112));
#22109=CARTESIAN_POINT('',(-0.00346484848679293,0.0146131526718383,-0.00534537352277043));
#22110=CARTESIAN_POINT('',(-0.0041664657681642,0.0146390183385049,-0.00481858200496197));
#22111=CARTESIAN_POINT('',(-0.00530278635263212,0.0146907496718381,-0.00352968672051604));
#22112=CARTESIAN_POINT('',(-0.00573748965572876,0.0147166153385046,-0.00276758295387855));
#22113=CARTESIAN_POINT('',(-0.0062684575946753,0.0147683466718376,-0.00113338577972021));
#22114=CARTESIAN_POINT('',(-0.0063647222305252,0.014794212338504,-0.000261292372199345));
#22115=CARTESIAN_POINT('',(-0.00622792473072616,0.0148379851243551,0.00118613325892089));
#22116=CARTESIAN_POINT('',(-0.0060870788531847,0.0148558922435399,0.00177021266515919));
#22117=CARTESIAN_POINT('',(-0.00586834292136768,0.0148737993627246,0.0023234413277993));
#22118=CARTESIAN_POINT('',(-0.00586834136008259,0.0138052138913639,0.00232344526570579));
#22119=CARTESIAN_POINT('',(-0.00564908206277401,0.0138231209680448,0.00287646519466028));
#22120=CARTESIAN_POINT('',(-0.00535192496700203,0.0138410280447258,0.00339865503213973));
#22121=CARTESIAN_POINT('',(-0.00446081589110761,0.0138848007880731,0.00454742612487075));
#22122=CARTESIAN_POINT('',(-0.00379365297342232,0.0139106664547395,0.00511725718126046));
#22123=CARTESIAN_POINT('',(-0.00228790905767161,0.0139623977880724,0.00594506308629448));
#22124=CARTESIAN_POINT('',(-0.00144932805960617,0.013988263454739,0.00620303793493879));
#22125=CARTESIAN_POINT('',(0.000261323533980394,0.0140399947880722,0.00636473719382177));
#22126=CARTESIAN_POINT('',(0.00113339412950152,0.0140658604547388,0.00626846160406045));
#22127=CARTESIAN_POINT('',(0.00276757460413525,0.0141175917880722,0.00573748564633127));
#22128=CARTESIAN_POINT('',(0.00352968448324786,0.014143457454739,0.00530278527836341));
#22129=CARTESIAN_POINT('',(0.00481858424226122,0.0141951887880726,0.00416646684240553));
#22130=CARTESIAN_POINT('',(0.00534537412216197,0.0142210544547394,0.0034648487744155));
#22131=CARTESIAN_POINT('',(0.00607698162277769,0.0142727857880731,0.00191010384640304));
#22132=CARTESIAN_POINT('',(0.00628179924349266,0.01429865145474,0.00105697698638061));
#22133=CARTESIAN_POINT('',(0.00633577167325347,0.0143503827880738,-0.000660453845968886));
#22134=CARTESIAN_POINT('',(0.00618492648229931,0.0143762484547407,-0.00152475781829595));
#22135=CARTESIAN_POINT('',(0.00555238592024544,0.0144279797880745,-0.00312237290991358));
#22136=CARTESIAN_POINT('',(0.00507069054914573,0.0144538454547414,-0.00385568402920414));
#22137=CARTESIAN_POINT('',(0.00385568403518145,0.0145055767880752,-0.00507069055515416));
#22138=CARTESIAN_POINT('',(0.00312237289231689,0.014531442454742,-0.00555238596181362));
#22139=CARTESIAN_POINT('',(0.0015247578358519,0.0145831737880757,-0.00618492644074725));
#22140=CARTESIAN_POINT('',(0.000660453922251479,0.0146090394547426,-0.00633577151302142));
#22141=CARTESIAN_POINT('',(-0.00105697706270651,0.0146607707880762,-0.00628179940372335));
#22142=CARTESIAN_POINT('',(-0.00191010413406409,0.0146866364547429,-0.00607698222215112));
#22143=CARTESIAN_POINT('',(-0.00346484848679293,0.0147383677880763,-0.00534537352277043));
#22144=CARTESIAN_POINT('',(-0.0041664657681642,0.014764233454743,-0.00481858200496198));
#22145=CARTESIAN_POINT('',(-0.00530278635263212,0.0148159647880762,-0.00352968672051604));
#22146=CARTESIAN_POINT('',(-0.00573748965572876,0.0148418304547427,-0.00276758295387855));
#22147=CARTESIAN_POINT('',(-0.0062684575946753,0.0148935617880757,-0.0011333857797202));
#22148=CARTESIAN_POINT('',(-0.0063647222305252,0.0149194274547421,-0.000261292372199344));
#22149=CARTESIAN_POINT('',(-0.00622792473072616,0.0149632002405932,0.00118613325892089));
#22150=CARTESIAN_POINT('',(-0.0060870788531847,0.014981107359778,0.00177021266515919));
#22151=CARTESIAN_POINT('',(-0.00586834292136768,0.0149990144789627,0.0023234413277993));
#22152=CARTESIAN_POINT('',(-0.00586834159873206,0.0138055280127714,0.00232344536019399));
#22153=CARTESIAN_POINT('',(-0.0056490822925068,0.0138234350894524,0.00287646531163829));
#22154=CARTESIAN_POINT('',(-0.00535192518465025,0.0138413421661333,0.00339865517035378));
#22155=CARTESIAN_POINT('',(-0.00446081607251684,0.0138851149094806,0.00454742630980219));
#22156=CARTESIAN_POINT('',(-0.00379365312769986,0.0139109805761471,0.00511725738936538));
#22157=CARTESIAN_POINT('',(-0.00228790915071464,0.01396271190948,0.00594506332806401));
#22158=CARTESIAN_POINT('',(-0.00144932811854639,0.0139885775761465,0.00620303818719946));
#22159=CARTESIAN_POINT('',(0.00026132354460771,0.0140403089094797,0.00636473745265831));
#22160=CARTESIAN_POINT('',(0.00113339417559357,0.0140661745761464,0.00626846185898172));
#22161=CARTESIAN_POINT('',(0.00276757471668497,0.0141179059094798,0.00573748587965919));
#22162=CARTESIAN_POINT('',(0.00352968462679052,0.0141437715761466,0.00530278549401325));
#22163=CARTESIAN_POINT('',(0.00481858443821992,0.0141955029094801,0.00416646701184439));
#22164=CARTESIAN_POINT('',(0.00534537433954379,0.014221368576147,0.00346484891532146));
#22165=CARTESIAN_POINT('',(0.00607698186991199,0.0142730999094807,0.00191010392408176));
#22166=CARTESIAN_POINT('',(0.00628179949895633,0.0142989655761476,0.00105697702936498));
#22167=CARTESIAN_POINT('',(0.00633577193091206,0.0143506969094813,-0.000660453872827746));
#22168=CARTESIAN_POINT('',(0.00618492673382343,0.0143765625761482,-0.0015247578803037));
#22169=CARTESIAN_POINT('',(0.00555238614604586,0.014428293909482,-0.00312237303689198));
#22170=CARTESIAN_POINT('',(0.00507069075535691,0.0144541595761489,-0.00385568418600431));
#22171=CARTESIAN_POINT('',(0.00385568419198163,0.0145058909094827,-0.00507069076136534));
#22172=CARTESIAN_POINT('',(0.00312237301929529,0.0145317565761496,-0.00555238618761404));
#22173=CARTESIAN_POINT('',(0.00152475789785965,0.0145834879094833,-0.00618492669227137));
#22174=CARTESIAN_POINT('',(0.000660453949110342,0.0146093535761501,-0.00633577177068));
#22175=CARTESIAN_POINT('',(-0.00105697710569089,0.0146610849094837,-0.00628179965918703));
#22176=CARTESIAN_POINT('',(-0.00191010421174282,0.0146869505761505,-0.00607698246928544));
#22177=CARTESIAN_POINT('',(-0.00346484862769889,0.0147386819094839,-0.00534537374015222));
#22178=CARTESIAN_POINT('',(-0.00416646593760302,0.0147645475761506,-0.00481858220092059));
#22179=CARTESIAN_POINT('',(-0.00530278656828201,0.0148162789094838,-0.00352968686405879));
#22180=CARTESIAN_POINT('',(-0.00573748988905685,0.0148421445761503,-0.00276758306642861));
#22181=CARTESIAN_POINT('',(-0.00626845784959641,0.0148938759094832,-0.00113338582581192));
#22182=CARTESIAN_POINT('',(-0.00636472248936113,0.0149197415761496,-0.000261292382825393));
#22183=CARTESIAN_POINT('',(-0.00622792498399891,0.0149635143620007,0.0011861333071577));
#22184=CARTESIAN_POINT('',(-0.00608707910072962,0.0149814214811855,0.00177021273714892));
#22185=CARTESIAN_POINT('',(-0.00586834316001721,0.0149993286003702,0.00232344142228734));
#22186=CARTESIAN_POINT('',(-0.00586834207591637,0.0138058421337995,0.00232344554912499));
#22187=CARTESIAN_POINT('',(-0.00564908275186204,0.0138237492104805,0.00287646554553812));
#22188=CARTESIAN_POINT('',(-0.00535192561984214,0.0138416562871614,0.00339865544671549));
#22189=CARTESIAN_POINT('',(-0.00446081643524819,0.0138854290305087,0.00454742667957625));
#22190=CARTESIAN_POINT('',(-0.00379365343618084,0.0139112946971751,0.00511725780547526));
#22191=CARTESIAN_POINT('',(-0.00228790933675601,0.0139630260305081,0.00594506381148695));
#22192=CARTESIAN_POINT('',(-0.00144932823639854,0.0139888916971746,0.00620303869159962));
#22193=CARTESIAN_POINT('',(0.000261323565857239,0.0140406230305078,0.00636473797020705));
#22194=CARTESIAN_POINT('',(0.00113339426775554,0.0140664886971744,0.00626846236870181));
#22195=CARTESIAN_POINT('',(0.00276757494173037,0.0141182200305079,0.00573748634620296));
#22196=CARTESIAN_POINT('',(0.00352968491380689,0.0141440856971746,0.00530278592520935));
#22197=CARTESIAN_POINT('',(0.00481858483004321,0.0141958170305082,0.00416646735064073));
#22198=CARTESIAN_POINT('',(0.005345374774203,0.014221682697175,0.00346484919706572));
#22199=CARTESIAN_POINT('',(0.00607698236406188,0.0142734140305088,0.0019101040794019));
#22200=CARTESIAN_POINT('',(0.00628180000976098,0.0142992796971756,0.00105697711531309));
#22201=CARTESIAN_POINT('',(0.00633577244610547,0.0143510110305094,-0.000660453926532565));
#22202=CARTESIAN_POINT('',(0.00618492723675087,0.0143768766971763,-0.00152475800428941));
#22203=CARTESIAN_POINT('',(0.00555238659753824,0.0144286080305101,-0.0031223732907878));
#22204=CARTESIAN_POINT('',(0.00507069116768023,0.014454473697177,-0.00385568449952934));
#22205=CARTESIAN_POINT('',(0.00385568450550666,0.0145062050305108,-0.00507069117368866));
#22206=CARTESIAN_POINT('',(0.00312237327319112,0.0145320706971777,-0.00555238663910643));
#22207=CARTESIAN_POINT('',(0.00152475802184537,0.0145838020305114,-0.0061849271951988));
#22208=CARTESIAN_POINT('',(0.000660454002815167,0.0146096676971782,-0.0063357722858734));
#22209=CARTESIAN_POINT('',(-0.00105697719163901,0.0146613990305118,-0.00628180016999169));
#22210=CARTESIAN_POINT('',(-0.00191010436706298,0.0146872646971786,-0.00607698296343539));
#22211=CARTESIAN_POINT('',(-0.00346484890944312,0.014738996030512,-0.00534537417481139));
#22212=CARTESIAN_POINT('',(-0.00416646627639928,0.0147648616971786,-0.00481858259274369));
#22213=CARTESIAN_POINT('',(-0.0053027869994782,0.0148165930305118,-0.00352968715107534));
#22214=CARTESIAN_POINT('',(-0.00573749035560094,0.0148424586971784,-0.00276758329147468));
#22215=CARTESIAN_POINT('',(-0.00626845835931617,0.0148941900305113,-0.00113338591797321));
#22216=CARTESIAN_POINT('',(-0.00636472300690866,0.0149200556971777,-0.000261292404072388));
#22217=CARTESIAN_POINT('',(-0.00622792549042275,0.0149638284830288,0.00118613340360815));
#22218=CARTESIAN_POINT('',(-0.00608707959570058,0.0149817356022136,0.0017702128810938));
#22219=CARTESIAN_POINT('',(-0.00586834363720165,0.0149996427213983,0.00232344161121802));
#22220=CARTESIAN_POINT('',(-0.00697824898150658,0.0138049000959188,0.00276288964191571));
#22221=CARTESIAN_POINT('',(-0.00697824906356397,0.0136487737981127,0.00276288967440459));
#22222=CARTESIAN_POINT('',(-0.00685805201880862,0.013337416869826,0.00271530020449264));
#22223=CARTESIAN_POINT('',(-0.00642329517116088,0.0131436916720262,0.00254316745395578));
#22224=CARTESIAN_POINT('',(-0.00598853832329639,0.0133374168692714,0.00237103470333308));
#22225=CARTESIAN_POINT('',(-0.00586834127820382,0.0136487737974034,0.00232344523328764));
#22226=CARTESIAN_POINT('',(-0.00586834136008268,0.0138049000952095,0.00232344526570583));
#22227=CARTESIAN_POINT('',(-0.00586849431301164,0.0138048999661087,0.00232350129736579));
#22228=CARTESIAN_POINT('',(-0.00697843088154052,0.0138048999657524,0.00276295622455691));
#22229=CARTESIAN_POINT('',(-0.00586834293970373,0.0138048997127905,0.00232344128155169));
#22230=CARTESIAN_POINT('',(-0.00525929270757257,0.0138546414019838,0.00385960227976077));
#22231=CARTESIAN_POINT('',(-0.00277900226167641,0.013954124780371,0.00641767178053703));
#22232=CARTESIAN_POINT('',(0.00257509559256523,0.0141033498479532,0.00650393974269634));
#22233=CARTESIAN_POINT('',(0.00641940303122683,0.0142525749155366,0.00277792062510722));
#22234=CARTESIAN_POINT('',(0.00650365220007484,0.0144017999831204,-0.0025749745534683));
#22235=CARTESIAN_POINT('',(0.00277793188520664,0.0145510250507043,-0.00641939815574492));
#22236=CARTESIAN_POINT('',(-0.00257508315426317,0.0147002501182876,-0.00650394466354535));
#22237=CARTESIAN_POINT('',(-0.00641900150925783,0.0148494751858699,-0.00277592942708743));
#22238=CARTESIAN_POINT('',(-0.0064759396950849,0.0149489585642571,0.000786698577753388));
#22239=CARTESIAN_POINT('',(-0.00586834507057426,0.0149987002534503,0.00232343589200159));
#22240=CARTESIAN_POINT('',(-0.00697825340504447,0.0149987003172936,0.00276287846683115));
#22241=CARTESIAN_POINT('',(-0.00770076531559239,0.0149489586280798,0.000935490630701186));
#22242=CARTESIAN_POINT('',(-0.00763305811880626,0.0148494752496517,-0.00330095434255674));
#22243=CARTESIAN_POINT('',(-0.00306212097811945,0.014700250182008,-0.00773406700938429));
#22244=CARTESIAN_POINT('',(0.0033033355401448,0.0145510251143632,-0.00763352978283033));
#22245=CARTESIAN_POINT('',(0.00773371923288734,0.0144018000467179,-0.00306199183214668));
#22246=CARTESIAN_POINT('',(0.00763353557833258,0.0142525749790727,0.00330332215531694));
#22247=CARTESIAN_POINT('',(0.00306213575895693,0.0141033499114279,0.00773406116183527));
#22248=CARTESIAN_POINT('',(-0.00330460837197012,0.0139541248437842,0.00763147688575125));
#22249=CARTESIAN_POINT('',(-0.00625400805880451,0.0138546414653561,0.00458958737822419));
#22250=CARTESIAN_POINT('',(-0.00697825087833439,0.0138048997761423,0.00276288485769634));
#22251=CARTESIAN_POINT('',(-0.0060046989412083,-0.00989161587683944,-0.00195124705900381));
#22252=CARTESIAN_POINT('',(-0.00574417341912455,-0.0100289714560031,-0.00275297912024915));
#22253=CARTESIAN_POINT('',(-0.00532098773851402,-0.0101627927695994,-0.00350163042607414));
#22254=CARTESIAN_POINT('',(-0.00421612753807775,-0.0104233668656572,-0.00477475344855832));
#22255=CARTESIAN_POINT('',(-0.00353445301825201,-0.0105501196481187,-0.00529922516521753));
#22256=CARTESIAN_POINT('',(-0.00202057350610914,-0.0107965566819069,-0.00604082678144128));
#22257=CARTESIAN_POINT('',(-0.00118836851379201,-0.0109162409332336,-0.00625795668100582));
#22258=CARTESIAN_POINT('',(0.000494838502468597,-0.0111485409047524,-0.00635053704198387));
#22259=CARTESIAN_POINT('',(0.00134584052641207,-0.0112611566249443,-0.00622598750339738));
#22260=CARTESIAN_POINT('',(0.0029319176516602,-0.0114793195341935,-0.00565491662083544));
#22261=CARTESIAN_POINT('',(0.00366699275296484,-0.0115848667232507,-0.00520839527685999));
#22262=CARTESIAN_POINT('',(0.00490484825389108,-0.0117888925702303,-0.00406407147112351));
#22263=CARTESIAN_POINT('',(0.00540762865351265,-0.0118873712281527,-0.00336626900936249));
#22264=CARTESIAN_POINT('',(0.0061013001303894,-0.0120772600128628,-0.00182985032013212));
#22265=CARTESIAN_POINT('',(0.00629219120764457,-0.0121686701396505,-0.000991234092662768));
#22266=CARTESIAN_POINT('',(0.00633186442354634,-0.012344421862091,0.000694051892870558));
#22267=CARTESIAN_POINT('',(0.00618064656219294,-0.0124287634577439,0.00154072165093454));
#22268=CARTESIAN_POINT('',(0.00556004095928272,-0.0125903781179149,0.00310807973892309));
#22269=CARTESIAN_POINT('',(0.00509065321772592,-0.012667651182433,0.00382876806884765));
#22270=CARTESIAN_POINT('',(0.00390801589266107,-0.0128151287803345,0.00503007226615351));
#22271=CARTESIAN_POINT('',(0.00319476630915303,-0.0128853333137179,0.00551068813353479));
#22272=CARTESIAN_POINT('',(0.0016373188335356,-0.0130186738493498,0.00615576166977231));
#22273=CARTESIAN_POINT('',(0.000793120941426222,-0.0130818098515984,0.00632021933862854));
#22274=CARTESIAN_POINT('',(-0.000892579781795836,-0.0132010133249608,0.0063069420913346));
#22275=CARTESIAN_POINT('',(-0.00173408261290851,-0.0132570807960746,0.00612920717518441));
#22276=CARTESIAN_POINT('',(-0.00328117503347942,-0.0133621472071675,0.00545967925016396));
#22277=CARTESIAN_POINT('',(-0.00398676462293764,-0.0134111461471466,0.0049678862412937));
#22278=CARTESIAN_POINT('',(-0.00515033405494463,-0.0135020754959699,0.00374810627762913));
#22279=CARTESIAN_POINT('',(-0.00560831389749338,-0.0135440059048142,0.00302011932283482));
#22280=CARTESIAN_POINT('',(-0.00620414568196542,-0.013620798191368,0.00144316383230204));
#22281=CARTESIAN_POINT('',(-0.00634199762388869,-0.0136556600690776,0.000594195296563549));
#22282=CARTESIAN_POINT('',(-0.0062758104309332,-0.0137183152933619,-0.00109019704146796));
#22283=CARTESIAN_POINT('',(-0.00607177129605443,-0.0137461086399366,-0.00192562084376098));
#22284=CARTESIAN_POINT('',(-0.00571282530871555,-0.013770367720944,-0.00268838268330946));
#22285=CARTESIAN_POINT('',(-0.00600351494261159,-0.00990699069817707,-0.00195086231468902));
#22286=CARTESIAN_POINT('',(-0.00574304079060577,-0.0100443462773407,-0.00275243629146672));
#22287=CARTESIAN_POINT('',(-0.00531993855318813,-0.010178167590937,-0.00350093997921721));
#22288=CARTESIAN_POINT('',(-0.00421529620762514,-0.0104387416869948,-0.00477381196898739));
#22289=CARTESIAN_POINT('',(-0.00353375609947977,-0.0105654944694563,-0.00529818027100706));
#22290=CARTESIAN_POINT('',(-0.00202017509209718,-0.0108119315032446,-0.0060396356592048));
#22291=CARTESIAN_POINT('',(-0.00118813419285994,-0.0109316157545713,-0.00625672274538287));
#22292=CARTESIAN_POINT('',(0.000494740930867046,-0.0111639157260901,-0.00634928485148777));
#22293=CARTESIAN_POINT('',(0.00134557515535679,-0.011276531446282,-0.0062247598714146));
#22294=CARTESIAN_POINT('',(0.00293133954001475,-0.0114946943555312,-0.00565380159185411));
#22295=CARTESIAN_POINT('',(0.00366626970018299,-0.0116002415445884,-0.00520736829236679));
#22296=CARTESIAN_POINT('',(0.00490388112239846,-0.0118042673915681,-0.0040632701228851));
#22297=CARTESIAN_POINT('',(0.00540656238444571,-0.0119027460494905,-0.00336560525289072));
#22298=CARTESIAN_POINT('',(0.00610009708409794,-0.0120926348342006,-0.00182948951266575));
#22299=CARTESIAN_POINT('',(0.00629095052170294,-0.0121840449609883,-0.000991038642435168));
#22300=CARTESIAN_POINT('',(0.00633061591489246,-0.0123597966834289,0.000693915040636124));
#22301=CARTESIAN_POINT('',(0.00617942787047698,-0.0124441382790818,0.00154041785347683));
#22302=CARTESIAN_POINT('',(0.00555894463775888,-0.0126057529392528,0.00310746689187024));
#22303=CARTESIAN_POINT('',(0.00508964944945624,-0.0126830260037709,0.00382801311742294));
#22304=CARTESIAN_POINT('',(0.00390724531525524,-0.0128305036016724,0.00502908044315575));
#22305=CARTESIAN_POINT('',(0.0031941363693569,-0.0129007081350558,0.00550960154333586));
#22306=CARTESIAN_POINT('',(0.00163699598917317,-0.0130340486706877,0.00615454788482654));
#22307=CARTESIAN_POINT('',(0.000792964554887801,-0.0130971846729363,0.0063189731261371));
#22308=CARTESIAN_POINT('',(-0.000892403784094794,-0.0132163881462987,0.00630569849683322));
#22309=CARTESIAN_POINT('',(-0.00173374068879202,-0.0132724556174126,0.00612799862621877));
#22310=CARTESIAN_POINT('',(-0.00328052805572528,-0.0133775220285054,0.0054586027178292));
#22311=CARTESIAN_POINT('',(-0.00398597851796133,-0.0134265209684845,0.00496690668005409));
#22312=CARTESIAN_POINT('',(-0.00514931851888639,-0.0135174503173078,0.00374736723098974));
#22313=CARTESIAN_POINT('',(-0.00560720805757541,-0.0135593807261521,0.0030195238197005));
#22314=CARTESIAN_POINT('',(-0.0062029223567241,-0.0136361730127058,0.001442879271166));
#22315=CARTESIAN_POINT('',(-0.00634074711718376,-0.0136710348904153,0.000594078133920726));
#22316=CARTESIAN_POINT('',(-0.00627457297493145,-0.0137336901146996,-0.00108998207785698));
#22317=CARTESIAN_POINT('',(-0.00607057407221948,-0.0137614834612743,-0.00192524115238941));
#22318=CARTESIAN_POINT('',(-0.00571169886137573,-0.0137857425422816,-0.00268785259156703));
#22319=CARTESIAN_POINT('',(-0.00600291424347733,-0.00992240968822442,-0.00195066711549076));
#22320=CARTESIAN_POINT('',(-0.00574246615396974,-0.0100597652673881,-0.00275216088845478));
#22321=CARTESIAN_POINT('',(-0.00531940625127604,-0.0101935865809844,-0.0035005896824936));
#22322=CARTESIAN_POINT('',(-0.00421487443391311,-0.0104541606770422,-0.00477333431135777));
#22323=CARTESIAN_POINT('',(-0.00353340251924388,-0.0105809134595037,-0.00529765014618313));
#22324=CARTESIAN_POINT('',(-0.00201997295760755,-0.010827350493292,-0.00603903134590728));
#22325=CARTESIAN_POINT('',(-0.00118801531064046,-0.0109470347446187,-0.00625609671080606));
#22326=CARTESIAN_POINT('',(0.000494691428125452,-0.0111793347161375,-0.00634864955534044));
#22327=CARTESIAN_POINT('',(0.00134544051992427,-0.0112919504363294,-0.00622413703497603));
#22328=CARTESIAN_POINT('',(0.00293104623631838,-0.0115101133455787,-0.00565323588430545));
#22329=CARTESIAN_POINT('',(0.00366590286091367,-0.0116156605346359,-0.00520684725399928));
#22330=CARTESIAN_POINT('',(0.0049033904503217,-0.0118196863816156,-0.00406286356058477));
#22331=CARTESIAN_POINT('',(0.00540602141513444,-0.011918165039538,-0.00336526849747643));
#22332=CARTESIAN_POINT('',(0.00609948672115684,-0.0121080538242481,-0.00182930645777592));
#22333=CARTESIAN_POINT('',(0.0062903210623665,-0.0121994639510358,-0.000990939481183764));
#22334=CARTESIAN_POINT('',(0.00632998248671984,-0.0123752156734764,0.000693845608950162));
#22335=CARTESIAN_POINT('',(0.00617880956986351,-0.0124595572691293,0.00154026372249193));
#22336=CARTESIAN_POINT('',(0.00555838842139842,-0.0126211719293004,0.00310715596523984));
#22337=CARTESIAN_POINT('',(0.00508914018978966,-0.0126984449938185,0.00382763009444597));
#22338=CARTESIAN_POINT('',(0.00390685436447048,-0.01284592259172,0.00502857724389711));
#22339=CARTESIAN_POINT('',(0.00319381677076005,-0.0129161271251034,0.00550905026414212));
#22340=CARTESIAN_POINT('',(0.00163683219478224,-0.0130494676607354,0.00615393207365233));
#22341=CARTESIAN_POINT('',(0.000792885212514845,-0.0131126036629839,0.00631834086291754));
#22342=CARTESIAN_POINT('',(-0.000892314492040781,-0.0132318071363464,0.00630506756184527));
#22343=CARTESIAN_POINT('',(-0.00173356721432902,-0.0132878746074602,0.00612738547150779));
#22344=CARTESIAN_POINT('',(-0.0032801998129572,-0.013392941018553,0.00545805654147115));
#22345=CARTESIAN_POINT('',(-0.00398557968929714,-0.013441939958532,0.004966409701772));
#22346=CARTESIAN_POINT('',(-0.00514880328885766,-0.0135328693073553,0.0037469922772713));
#22347=CARTESIAN_POINT('',(-0.00560664701207823,-0.0135747997161996,0.00301922169246975));
#22348=CARTESIAN_POINT('',(-0.00620230170530153,-0.0136515920027533,0.0014427348996874));
#22349=CARTESIAN_POINT('',(-0.00634011267530426,-0.0136864538804628,0.0005940186917066));
#22350=CARTESIAN_POINT('',(-0.00627394515429805,-0.013749109104747,-0.0010898730165326));
#22351=CARTESIAN_POINT('',(-0.00606996666328913,-0.0137769024513216,-0.00192504851679101));
#22352=CARTESIAN_POINT('',(-0.00571112736074751,-0.0138011615323289,-0.00268758365066487));
#22353=CARTESIAN_POINT('',(-0.00600291424347732,-0.0100937412712376,-0.00195066711549076));
#22354=CARTESIAN_POINT('',(-0.00574246615396973,-0.0102310968504013,-0.00275216088845478));
#22355=CARTESIAN_POINT('',(-0.00531940625127603,-0.0103649181639975,-0.00350058968249358));
#22356=CARTESIAN_POINT('',(-0.0042148744339131,-0.0106254922600554,-0.00477333431135776));
#22357=CARTESIAN_POINT('',(-0.00353340251924387,-0.010752245042517,-0.00529765014618313));
#22358=CARTESIAN_POINT('',(-0.00201997295760755,-0.0109986820763054,-0.00603903134590728));
#22359=CARTESIAN_POINT('',(-0.00118801531064047,-0.0111183663276323,-0.00625609671080605));
#22360=CARTESIAN_POINT('',(0.000494691428125445,-0.0113506662991512,-0.00634864955534043));
#22361=CARTESIAN_POINT('',(0.00134544051992427,-0.0114632820193433,-0.00622413703497602));
#22362=CARTESIAN_POINT('',(0.00293104623631838,-0.0116814449285928,-0.00565323588430546));
#22363=CARTESIAN_POINT('',(0.00366590286091366,-0.0117869921176501,-0.00520684725399929));
#22364=CARTESIAN_POINT('',(0.00490339045032169,-0.0119910179646301,-0.00406286356058478));
#22365=CARTESIAN_POINT('',(0.00540602141513444,-0.0120894966225526,-0.00336526849747642));
#22366=CARTESIAN_POINT('',(0.00609948672115685,-0.012279385407263,-0.00182930645777591));
#22367=CARTESIAN_POINT('',(0.0062903210623665,-0.0123707955340508,-0.000990939481183761));
#22368=CARTESIAN_POINT('',(0.00632998248671984,-0.0125465472564916,0.000693845608950159));
#22369=CARTESIAN_POINT('',(0.00617880956986352,-0.0126308888521447,0.00154026372249192));
#22370=CARTESIAN_POINT('',(0.00555838842139841,-0.0127925035123159,0.00310715596523981));
#22371=CARTESIAN_POINT('',(0.00508914018978966,-0.0128697765768341,0.00382763009444594));
#22372=CARTESIAN_POINT('',(0.00390685436447047,-0.0130172541747358,0.0050285772438971));
#22373=CARTESIAN_POINT('',(0.00319381677076006,-0.0130874587081192,0.0055090502641421));
#22374=CARTESIAN_POINT('',(0.00163683219478224,-0.0132207992437512,0.00615393207365233));
#22375=CARTESIAN_POINT('',(0.000792885212514844,-0.0132839352459997,0.00631834086291754));
#22376=CARTESIAN_POINT('',(-0.000892314492040773,-0.0134031387193621,0.00630506756184528));
#22377=CARTESIAN_POINT('',(-0.00173356721432899,-0.0134592061904759,0.00612738547150781));
#22378=CARTESIAN_POINT('',(-0.00328019981295716,-0.0135642726015686,0.00545805654147116));
#22379=CARTESIAN_POINT('',(-0.00398557968929713,-0.0136132715415475,0.004966409701772));
#22380=CARTESIAN_POINT('',(-0.00514880328885766,-0.0137042008903706,0.00374699227727129));
#22381=CARTESIAN_POINT('',(-0.00560664701207822,-0.0137461312992146,0.00301922169246975));
#22382=CARTESIAN_POINT('',(-0.00620230170530152,-0.0138229235857679,0.0014427348996874));
#22383=CARTESIAN_POINT('',(-0.00634011267530425,-0.0138577854634772,0.000594018691706603));
#22384=CARTESIAN_POINT('',(-0.00627394515429805,-0.0139204406877607,-0.0010898730165326));
#22385=CARTESIAN_POINT('',(-0.00606996666328912,-0.0139482340343351,-0.001925048516791));
#22386=CARTESIAN_POINT('',(-0.0057111273607475,-0.013972493115342,-0.00268758365066487));
#22387=CARTESIAN_POINT('',(-0.00606433392192398,-0.0102496538642035,-0.0019706256459862));
#22388=CARTESIAN_POINT('',(-0.00580122102041663,-0.0103870094433671,-0.00278032001749549));
#22389=CARTESIAN_POINT('',(-0.0053738325196232,-0.0105208307569634,-0.00353640646813335));
#22390=CARTESIAN_POINT('',(-0.00425799952648047,-0.0107814048530212,-0.00482217336629522));
#22391=CARTESIAN_POINT('',(-0.00356955503413119,-0.0109081576354828,-0.00535185381381923));
#22392=CARTESIAN_POINT('',(-0.00204064060077138,-0.0111545946692711,-0.00610082056166993));
#22393=CARTESIAN_POINT('',(-0.00120017065976085,-0.0112742789205979,-0.00632010686199661));
#22394=CARTESIAN_POINT('',(0.000499752934456115,-0.0115065788921167,-0.00641360667424035));
#22395=CARTESIAN_POINT('',(0.00135920658766256,-0.0116191946123087,-0.0062878201861574));
#22396=CARTESIAN_POINT('',(0.0029610356564642,-0.011837357521558,-0.00571107777844453));
#22397=CARTESIAN_POINT('',(0.00370341107205939,-0.0119429047106153,-0.0052601218588146));
#22398=CARTESIAN_POINT('',(0.00495356019330685,-0.012146930557595,-0.00410443333208948));
#22399=CARTESIAN_POINT('',(0.00546133389895912,-0.0122454092155175,-0.00339970072499429));
#22400=CARTESIAN_POINT('',(0.00616189449476616,-0.0124352980002277,-0.00184802326928778));
#22401=CARTESIAN_POINT('',(0.00635468138492093,-0.0125267081270155,-0.00100107842067645));
#22402=CARTESIAN_POINT('',(0.0063947486108286,-0.0127024598494561,0.000700944789858774));
#22403=CARTESIAN_POINT('',(0.0062420289465815,-0.0127868014451091,0.00155602315178267));
#22404=CARTESIAN_POINT('',(0.005615259870111,-0.0129484161052802,0.00313894727734728));
#22405=CARTESIAN_POINT('',(0.00514121045788761,-0.0130256891697984,0.00386679304098799));
#22406=CARTESIAN_POINT('',(0.00394682790549922,-0.0131731667676999,0.00508002785352392));
#22407=CARTESIAN_POINT('',(0.00322649476533423,-0.0132433713010833,0.00556541690241914));
#22408=CARTESIAN_POINT('',(0.00165357967825393,-0.0133767118367152,0.00621689691269813));
#22409=CARTESIAN_POINT('',(0.00080099773133863,-0.0134398478389638,0.0063829878740819));
#22410=CARTESIAN_POINT('',(-0.000901444335805242,-0.0135590513123262,0.00636957876532512));
#22411=CARTESIAN_POINT('',(-0.00175130445603381,-0.01361511878344,0.00619007869518455));
#22412=CARTESIAN_POINT('',(-0.0033137616480228,-0.0137201851945328,0.00551390143015753));
#22413=CARTESIAN_POINT('',(-0.00402635871978323,-0.0137691841345118,0.00501722423527106));
#22414=CARTESIAN_POINT('',(-0.00520148400851484,-0.013860113483335,0.00378533016641609));
#22415=CARTESIAN_POINT('',(-0.00566401222548603,-0.0139020438921792,0.00305011329244757));
#22416=CARTESIAN_POINT('',(-0.00626576144517416,-0.0139788361787328,0.00145749644883311));
#22417=CARTESIAN_POINT('',(-0.00640498244789111,-0.0140136980564422,0.000600096479187168));
#22418=CARTESIAN_POINT('',(-0.00633813792439929,-0.0140763532807262,-0.00110102420868829));
#22419=CARTESIAN_POINT('',(-0.00613207239819051,-0.0141041466273008,-0.0019447449269178));
#22420=CARTESIAN_POINT('',(-0.00576956157983471,-0.0141284057083079,-0.00271508204843087));
#22421=CARTESIAN_POINT('',(-0.00627403382107316,-0.0104701475677205,-0.00203876833148874));
#22422=CARTESIAN_POINT('',(-0.00600182268229503,-0.0106075031468842,-0.00287646129777087));
#22423=CARTESIAN_POINT('',(-0.00555965542316345,-0.0107413244604805,-0.0036586926234252));
#22424=CARTESIAN_POINT('',(-0.00440523780240261,-0.0110018985565383,-0.00498892033003615));
#22425=CARTESIAN_POINT('',(-0.00369298744077334,-0.0111286513389998,-0.00553691671099277));
#22426=CARTESIAN_POINT('',(-0.00211120434836357,-0.011375088372788,-0.00631178214013517));
#22427=CARTESIAN_POINT('',(-0.00124167161758307,-0.0114947726241148,-0.00653865118832096));
#22428=CARTESIAN_POINT('',(0.00051703399801631,-0.0117270725956335,-0.00663538415056112));
#22429=CARTESIAN_POINT('',(0.00140620688283519,-0.0118396883158255,-0.00650524806461549));
#22430=CARTESIAN_POINT('',(0.00306342594145377,-0.0120578512250747,-0.00590856235788749));
#22431=CARTESIAN_POINT('',(0.00383147211525347,-0.0121633984141319,-0.00544201273710512));
#22432=CARTESIAN_POINT('',(0.00512485041022755,-0.0123674242611115,-0.00424636140974563));
#22433=CARTESIAN_POINT('',(0.00565018253140191,-0.0124659029190339,-0.00351725970316851));
#22434=CARTESIAN_POINT('',(0.00637496796182063,-0.0126557917037441,-0.00191192646099593));
#22435=CARTESIAN_POINT('',(0.00657442127106498,-0.0127472018305317,-0.00103569492540046));
#22436=CARTESIAN_POINT('',(0.00661587399014308,-0.0129229535529723,0.000725182909598715));
#22437=CARTESIAN_POINT('',(0.00645787339997682,-0.0130072951486252,0.00160982920900241));
#22438=CARTESIAN_POINT('',(0.00580943114161729,-0.0131689098087962,0.00324748960631019));
#22439=CARTESIAN_POINT('',(0.00531898947342402,-0.0132461828733143,0.00400050370421426));
#22440=CARTESIAN_POINT('',(0.00408330611141565,-0.0133936604712158,0.00525569122270414));
#22441=CARTESIAN_POINT('',(0.00333806441760055,-0.0134638650045992,0.00575786464328995));
#22442=CARTESIAN_POINT('',(0.00171075916345863,-0.0135972055402311,0.00643187232012095));
#22443=CARTESIAN_POINT('',(0.000828695603131797,-0.0136603415424797,0.00660370657636615));
#22444=CARTESIAN_POINT('',(-0.00093261557220824,-0.0137795450158421,0.00658983379117099));
#22445=CARTESIAN_POINT('',(-0.00181186318722145,-0.0138356124869559,0.00640412674973063));
#22446=CARTESIAN_POINT('',(-0.00342834892048198,-0.0139406788980488,0.00570456780649976));
#22447=CARTESIAN_POINT('',(-0.00416558703872929,-0.0139896778380279,0.00519071590470924));
#22448=CARTESIAN_POINT('',(-0.00538134723604398,-0.0140806071868512,0.00391622390748699));
#22449=CARTESIAN_POINT('',(-0.00585986931511135,-0.0141225375956955,0.00315558381205526));
#22450=CARTESIAN_POINT('',(-0.00648242654971197,-0.0141993298822493,0.00150789553012803));
#22451=CARTESIAN_POINT('',(-0.00662646170524521,-0.0142341917599588,0.000620847343632541));
#22452=CARTESIAN_POINT('',(-0.00655730575068522,-0.014296846984243,-0.00113909676018287));
#22453=CARTESIAN_POINT('',(-0.00634411464059197,-0.0143246403308177,-0.00201199267750278));
#22454=CARTESIAN_POINT('',(-0.00596906848314891,-0.0143488994118251,-0.00280896745102709));
#22455=CARTESIAN_POINT('',(-0.00642231404177568,-0.0105347286782718,-0.00208695248649585));
#22456=CARTESIAN_POINT('',(-0.00614366947772652,-0.0106720842574354,-0.00294444344900556));
#22457=CARTESIAN_POINT('',(-0.00569105205835654,-0.0108059055710317,-0.0037451619930773));
#22458=CARTESIAN_POINT('',(-0.00450935098575737,-0.0110664796670895,-0.00510682823883964));
#22459=CARTESIAN_POINT('',(-0.00378026733252819,-0.011193232449551,-0.00566777594053021));
#22460=CARTESIAN_POINT('',(-0.00216110045279195,-0.0114396694833393,-0.00646095450283777));
#22461=CARTESIAN_POINT('',(-0.0012710172262849,-0.0115593537346661,-0.00669318536345474));
#22462=CARTESIAN_POINT('',(0.000529253555245836,-0.0117916537061849,-0.00679220450798196));
#22463=CARTESIAN_POINT('',(0.00143944111026952,-0.0119042694263769,-0.00665899279189221));
#22464=CARTESIAN_POINT('',(0.00313582680629751,-0.0121224323356261,-0.00604820504319139));
#22465=CARTESIAN_POINT('',(0.00392202494730184,-0.0122279795246833,-0.00557062901058033));
#22466=CARTESIAN_POINT('',(0.00524597088416309,-0.012432005371663,-0.00434671971589707));
#22467=CARTESIAN_POINT('',(0.00578371868002001,-0.0125304840295855,-0.00360038645382486));
#22468=CARTESIAN_POINT('',(0.00652563365526577,-0.0127203728142956,-0.00195711284119222));
#22469=CARTESIAN_POINT('',(0.0067298008346546,-0.0128117829410833,-0.00106017249063177));
#22470=CARTESIAN_POINT('',(0.00677223324534879,-0.012987534663524,0.00074232184843004));
#22471=CARTESIAN_POINT('',(0.00661049847665415,-0.0130718762591769,0.0016478758369314));
#22472=CARTESIAN_POINT('',(0.005946730964411,-0.0132334909193479,0.00332424062316563));
#22473=CARTESIAN_POINT('',(0.00544469822086248,-0.0133107639838661,0.00409505142089849));
#22474=CARTESIAN_POINT('',(0.00417981077630333,-0.0134582415817676,0.00537990398225753));
#22475=CARTESIAN_POINT('',(0.00341695607529269,-0.013528446115151,0.00589394574588372));
#22476=CARTESIAN_POINT('',(0.00175119116519162,-0.0136617866507829,0.00658388288849797));
#22477=CARTESIAN_POINT('',(0.000848280956101178,-0.0137249226530315,0.00675977826748603));
#22478=CARTESIAN_POINT('',(-0.000954656964846768,-0.0138441261263939,0.00674557761353703));
#22479=CARTESIAN_POINT('',(-0.00185468467670427,-0.0139001935975077,0.00655548158059996));
#22480=CARTESIAN_POINT('',(-0.00350937435787551,-0.0140052600086006,0.00583938929415562));
#22481=CARTESIAN_POINT('',(-0.00426403632718924,-0.0140542589485796,0.00531339304064835));
#22482=CARTESIAN_POINT('',(-0.00550852974391592,-0.0141451882974029,0.0040087797594131));
#22483=CARTESIAN_POINT('',(-0.00599836119132887,-0.0141871187062471,0.00323016273168512));
#22484=CARTESIAN_POINT('',(-0.00663563191437714,-0.0142639109928008,0.00154353306227724));
#22485=CARTESIAN_POINT('',(-0.00678307119001246,-0.0142987728705102,0.000635520420597347));
#22486=CARTESIAN_POINT('',(-0.00671228080686991,-0.0143614280947944,-0.00116601811952175));
#22487=CARTESIAN_POINT('',(-0.00649405114809204,-0.014389221441369,-0.00205954401796095));
#22488=CARTESIAN_POINT('',(-0.00611014116737591,-0.0144134805223763,-0.0028753544558573));
#22489=CARTESIAN_POINT('',(-0.00671887448318071,-0.0105347286782718,-0.00218332079651008));
#22490=CARTESIAN_POINT('',(-0.00642736306858952,-0.0106720842574354,-0.00308040775147493));
#22491=CARTESIAN_POINT('',(-0.0059538453287427,-0.0108059055710317,-0.00391810073238151));
#22492=CARTESIAN_POINT('',(-0.00471757735246687,-0.0110664796670895,-0.0053426440564466));
#22493=CARTESIAN_POINT('',(-0.00395482711603786,-0.011193232449551,-0.00592949439960509));
#22494=CARTESIAN_POINT('',(-0.00226089266164871,-0.0114396694833393,-0.00675929922824295));
#22495=CARTESIAN_POINT('',(-0.00132970844368856,-0.0115593537346661,-0.00700225371372231));
#22496=CARTESIAN_POINT('',(0.000553692669704887,-0.0117916537061849,-0.00710584522282366));
#22497=CARTESIAN_POINT('',(0.00150590956513818,-0.0119042694263769,-0.00696648224644565));
#22498=CARTESIAN_POINT('',(0.00328062853598501,-0.0121224323356261,-0.0063274904137992));
#22499=CARTESIAN_POINT('',(0.00410313061139855,-0.0122279795246833,-0.00582786155753075));
#22500=CARTESIAN_POINT('',(0.00548821183203415,-0.012432005371663,-0.00454743632819994));
#22501=CARTESIAN_POINT('',(0.00605079097725621,-0.0125304840295855,-0.00376663995513757));
#22502=CARTESIAN_POINT('',(0.00682696504215606,-0.0127203728142956,-0.00204748560158481));
#22503=CARTESIAN_POINT('',(0.00704055996183384,-0.0128117829410833,-0.00110912762109441));
#22504=CARTESIAN_POINT('',(0.00708495175576022,-0.012987534663524,0.000776599726092681));
#22505=CARTESIAN_POINT('',(0.00691574863000881,-0.0130718762591769,0.00172396909278938));
#22506=CARTESIAN_POINT('',(0.00622133060999841,-0.0132334909193479,0.00347774265687652));
#22507=CARTESIAN_POINT('',(0.00569611571573941,-0.0133107639838661,0.00428414685426696));
#22508=CARTESIAN_POINT('',(0.00437282010607869,-0.0134582415817676,0.00562832950136433));
#22509=CARTESIAN_POINT('',(0.00357473939067698,-0.013528446115151,0.00616610795107127));
#22510=CARTESIAN_POINT('',(0.0018320551686576,-0.0136617866507829,0.006887904025252));
#22511=CARTESIAN_POINT('',(0.000887451662039945,-0.0137249226530315,0.00707192164972581));
#22512=CARTESIAN_POINT('',(-0.000998739750123817,-0.0138441261263939,0.00705706525826912));
#22513=CARTESIAN_POINT('',(-0.00194032765566992,-0.0139001935975077,0.00685819124233862));
#22514=CARTESIAN_POINT('',(-0.00367142523266258,-0.0140052600086006,0.00610903226946734));
#22515=CARTESIAN_POINT('',(-0.00446093490410914,-0.0140542589485796,0.00555874731252656));
#22516=CARTESIAN_POINT('',(-0.00576289475965981,-0.0141451882974029,0.00419389146326531));
#22517=CARTESIAN_POINT('',(-0.00627534494376392,-0.0141871187062471,0.00337932057094484));
#22518=CARTESIAN_POINT('',(-0.00694204264370749,-0.0142639109928008,0.00161480812657567));
#22519=CARTESIAN_POINT('',(-0.00709629015954695,-0.0142987728705102,0.00066486657452696));
#22520=CARTESIAN_POINT('',(-0.0070222309192393,-0.0143614280947944,-0.00121986083819952));
#22521=CARTESIAN_POINT('',(-0.00679392416309219,-0.014389221441369,-0.00215464669887731));
#22522=CARTESIAN_POINT('',(-0.00639228653582991,-0.0144134805223763,-0.00300812846551772));
#22523=CARTESIAN_POINT('',(-0.00686715470388324,-0.0104701475677205,-0.00223150495151719));
#22524=CARTESIAN_POINT('',(-0.00656920986402103,-0.0106075031468842,-0.00314838990270961));
#22525=CARTESIAN_POINT('',(-0.00608524196393579,-0.0107413244604805,-0.00400457010203361));
#22526=CARTESIAN_POINT('',(-0.00482169053582163,-0.0110018985565383,-0.00546055196525008));
#22527=CARTESIAN_POINT('',(-0.00404210700779271,-0.0111286513389998,-0.00606035362914253));
#22528=CARTESIAN_POINT('',(-0.00231078876607709,-0.011375088372788,-0.00690847159094555));
#22529=CARTESIAN_POINT('',(-0.00135905405239039,-0.0114947726241148,-0.0071567878888561));
#22530=CARTESIAN_POINT('',(0.000565912226934413,-0.0117270725956335,-0.00726266558024451));
#22531=CARTESIAN_POINT('',(0.00153914379257251,-0.0118396883158255,-0.00712022697372237));
#22532=CARTESIAN_POINT('',(0.00335302940082875,-0.0120578512250747,-0.00646713309910309));
#22533=CARTESIAN_POINT('',(0.0041936834434469,-0.0121633984141319,-0.00595647783100596));
#22534=CARTESIAN_POINT('',(0.00560933230596968,-0.0123674242611115,-0.00464779463435138));
#22535=CARTESIAN_POINT('',(0.00618432712587431,-0.0124659029190339,-0.00384976670579392));
#22536=CARTESIAN_POINT('',(0.0069776307356012,-0.012655791703744,-0.00209267198178111));
#22537=CARTESIAN_POINT('',(0.00719593952542346,-0.0127472018305317,-0.00113360518632574));
#22538=CARTESIAN_POINT('',(0.00724131101096593,-0.0129229535529723,0.000793738664923998));
#22539=CARTESIAN_POINT('',(0.00706837370668615,-0.0130072951486252,0.00176201572071837));
#22540=CARTESIAN_POINT('',(0.00635863043279212,-0.0131689098087962,0.00355449367373196));
#22541=CARTESIAN_POINT('',(0.00582182446317788,-0.0132461828733143,0.00437869457095119));
#22542=CARTESIAN_POINT('',(0.00446932477096638,-0.0133936604712158,0.00575254226091774));
#22543=CARTESIAN_POINT('',(0.00365363104836912,-0.0134638650045992,0.00630218905366504));
#22544=CARTESIAN_POINT('',(0.0018724871703906,-0.0135972055402311,0.00703991459362902));
#22545=CARTESIAN_POINT('',(0.000907037015009332,-0.0136603415424797,0.0072279933408457));
#22546=CARTESIAN_POINT('',(-0.00102078114276234,-0.0137795450158421,0.00721280908063516));
#22547=CARTESIAN_POINT('',(-0.00198314914515274,-0.0138356124869559,0.00700954607320794));
#22548=CARTESIAN_POINT('',(-0.00375245067005612,-0.0139406788980488,0.0062438537571232));
#22549=CARTESIAN_POINT('',(-0.0045593841925691,-0.0139896778380279,0.00568142444846567));
#22550=CARTESIAN_POINT('',(-0.00589007726753176,-0.0140806071868512,0.00428644731519142));
#22551=CARTESIAN_POINT('',(-0.00641383681998145,-0.0141225375956955,0.0034538994905747));
#22552=CARTESIAN_POINT('',(-0.00709524800837267,-0.0141993298822493,0.00165044565872487));
#22553=CARTESIAN_POINT('',(-0.00725289964431421,-0.0142341917599588,0.000679539651491767));
#22554=CARTESIAN_POINT('',(-0.007177205975424,-0.014296846984243,-0.00124678219753841));
#22555=CARTESIAN_POINT('',(-0.00694386067059227,-0.0143246403308177,-0.00220219803933549));
#22556=CARTESIAN_POINT('',(-0.0065333592200569,-0.0143488994118251,-0.00307451547034793));
#22557=CARTESIAN_POINT('',(-0.00707685460303241,-0.0102496538642035,-0.00229964763701973));
#22558=CARTESIAN_POINT('',(-0.00676981152589942,-0.0103870094433671,-0.003244531182985));
#22559=CARTESIAN_POINT('',(-0.00627106486747605,-0.0105208307569634,-0.00412685625732547));
#22560=CARTESIAN_POINT('',(-0.00496892881174377,-0.0107814048530212,-0.00562729892899101));
#22561=CARTESIAN_POINT('',(-0.00416553941443487,-0.0109081576354828,-0.00624541652631608));
#22562=CARTESIAN_POINT('',(-0.00238135251366929,-0.0111545946692711,-0.00711943316941079));
#22563=CARTESIAN_POINT('',(-0.00140055501021261,-0.0112742789205979,-0.00737533221518044));
#22564=CARTESIAN_POINT('',(0.000583193290494599,-0.0115065788921167,-0.00748444305656528));
#22565=CARTESIAN_POINT('',(0.00158614408774513,-0.0116191946123087,-0.00733765485218046));
#22566=CARTESIAN_POINT('',(0.00345541968581831,-0.011837357521558,-0.00666461767854607));
#22567=CARTESIAN_POINT('',(0.00432174448664098,-0.0119429047106153,-0.00613836870929649));
#22568=CARTESIAN_POINT('',(0.00578062252289037,-0.012146930557595,-0.00478972271200754));
#22569=CARTESIAN_POINT('',(0.00637317575831709,-0.0122454092155175,-0.00396732568396815));
#22570=CARTESIAN_POINT('',(0.00719070420265566,-0.0124352980002277,-0.00215657517348927));
#22571=CARTESIAN_POINT('',(0.00741567941156751,-0.0125267081270155,-0.00116822169104975));
#22572=CARTESIAN_POINT('',(0.00746243639028041,-0.0127024598494561,0.000817976784663933));
#22573=CARTESIAN_POINT('',(0.00728421816008148,-0.0127868014451091,0.0018158217779381));
#22574=CARTESIAN_POINT('',(0.00655280170429842,-0.0129484161052802,0.00366303600269487));
#22575=CARTESIAN_POINT('',(0.0059996034787143,-0.0130256891697984,0.00451240523417745));
#22576=CARTESIAN_POINT('',(0.00460580297688281,-0.0131731667676999,0.00592820563009794));
#22577=CARTESIAN_POINT('',(0.00376520070063544,-0.0132433713010833,0.00649463679453584));
#22578=CARTESIAN_POINT('',(0.00192966665559529,-0.0133767118367153,0.00725489000105184));
#22579=CARTESIAN_POINT('',(0.000934734886802505,-0.0134398478389638,0.00744871204312994));
#22580=CARTESIAN_POINT('',(-0.00105195237916532,-0.0135590513123262,0.00743306410648104));
#22581=CARTESIAN_POINT('',(-0.00204370787634037,-0.01361511878344,0.00722359412775403));
#22582=CARTESIAN_POINT('',(-0.00386703794251528,-0.0137201851945328,0.00643452013346544));
#22583=CARTESIAN_POINT('',(-0.00469861251151514,-0.0137691841345118,0.00585491611790385));
#22584=CARTESIAN_POINT('',(-0.00606994049506089,-0.013860113483335,0.00441734105626232));
#22585=CARTESIAN_POINT('',(-0.00660969390960677,-0.0139020438921792,0.00355937001018238));
#22586=CARTESIAN_POINT('',(-0.00731191311291048,-0.0139788361787328,0.00170084474001979));
#22587=CARTESIAN_POINT('',(-0.0074743789016683,-0.0140136980564422,0.000700290515937141));
#22588=CARTESIAN_POINT('',(-0.00739637380170993,-0.0140763532807262,-0.00128485474903298));
#22589=CARTESIAN_POINT('',(-0.00715590291299373,-0.0141041466273008,-0.00226944578992046));
#22590=CARTESIAN_POINT('',(-0.00673286612337111,-0.014128405708308,-0.00316840087294414));
#22591=CARTESIAN_POINT('',(-0.00713827428147907,-0.0100937412712376,-0.00231960616751517));
#22592=CARTESIAN_POINT('',(-0.00682856639234631,-0.0102310968504013,-0.00327269031202571));
#22593=CARTESIAN_POINT('',(-0.00632549113582322,-0.0103649181639976,-0.00416267304296523));
#22594=CARTESIAN_POINT('',(-0.00501205390431115,-0.0106254922600555,-0.00567613798392846));
#22595=CARTESIAN_POINT('',(-0.00420169192932218,-0.010752245042517,-0.00629962019395218));
#22596=CARTESIAN_POINT('',(-0.0024020201568331,-0.0109986820763054,-0.00718122238517345));
#22597=CARTESIAN_POINT('',(-0.001412710359333,-0.0111183663276323,-0.007439342366371));
#22598=CARTESIAN_POINT('',(0.00058825479682526,-0.0113506662991512,-0.00754940017546519));
#22599=CARTESIAN_POINT('',(0.00159991015548341,-0.0114632820193433,-0.00740133800336183));
#22600=CARTESIAN_POINT('',(0.00348540910596414,-0.0116814449285928,-0.00672245957268514));
#22601=CARTESIAN_POINT('',(0.00435925269778671,-0.0117869921176501,-0.0061916433141118));
#22602=CARTESIAN_POINT('',(0.00583079226587554,-0.0119910179646301,-0.00483129248351225));
#22603=CARTESIAN_POINT('',(0.00642848824214178,-0.0120894966225526,-0.00400175791148603));
#22604=CARTESIAN_POINT('',(0.00725311197626499,-0.012279385407263,-0.00217529198500113));
#22605=CARTESIAN_POINT('',(0.00748003973412194,-0.0123707955340508,-0.00117836063054244));
#22606=CARTESIAN_POINT('',(0.00752720251438918,-0.0125465472564916,0.000825075965572551));
#22607=CARTESIAN_POINT('',(0.00734743753679947,-0.0126308888521447,0.00183158120722885));
#22608=CARTESIAN_POINT('',(0.006609673153011,-0.0127925035123159,0.00369482731480231));
#22609=CARTESIAN_POINT('',(0.00605167374681224,-0.0128697765768341,0.00455156818071947));
#22610=CARTESIAN_POINT('',(0.00464577651791155,-0.0130172541747358,0.00597965623972474));
#22611=CARTESIAN_POINT('',(0.00379787869520962,-0.0130874587081192,0.00655100343281285));
#22612=CARTESIAN_POINT('',(0.00194641413906699,-0.0132207992437512,0.00731785484009763));
#22613=CARTESIAN_POINT('',(0.00094284740562629,-0.0132839352459998,0.0075133590542943));
#22614=CARTESIAN_POINT('',(-0.00106108222292979,-0.0134031387193622,0.00749757530996088));
#22615=CARTESIAN_POINT('',(-0.00206144511804517,-0.0134592061904759,0.00728628735143079));
#22616=CARTESIAN_POINT('',(-0.0039005997775809,-0.0135642726015686,0.00649036502215181));
#22617=CARTESIAN_POINT('',(-0.00473939154200123,-0.0136132715415475,0.00590573065140292));
#22618=CARTESIAN_POINT('',(-0.00612262121471807,-0.0137042008903706,0.00445567894540712));
#22619=CARTESIAN_POINT('',(-0.00666705912301456,-0.0137461312992147,0.00359026161016021));
#22620=CARTESIAN_POINT('',(-0.0073753728527831,-0.0138229235857679,0.00171560628916551));
#22621=CARTESIAN_POINT('',(-0.00753924867425515,-0.0138577854634772,0.000706368303417708));
#22622=CARTESIAN_POINT('',(-0.00746056657181116,-0.0139204406877607,-0.00129600594118867));
#22623=CARTESIAN_POINT('',(-0.00721800864789512,-0.0139482340343351,-0.00228914220004725));
#22624=CARTESIAN_POINT('',(-0.00679130034245832,-0.013972493115342,-0.00319589927071014));
#22625=CARTESIAN_POINT('',(-0.00713827428147907,-0.00992240968822442,-0.00231960616751517));
#22626=CARTESIAN_POINT('',(-0.00682856639234631,-0.0100597652673881,-0.00327269031202571));
#22627=CARTESIAN_POINT('',(-0.00632549113582321,-0.0101935865809844,-0.00416267304296523));
#22628=CARTESIAN_POINT('',(-0.00501205390431114,-0.0104541606770422,-0.00567613798392846));
#22629=CARTESIAN_POINT('',(-0.00420169192932218,-0.0105809134595037,-0.00629962019395218));
#22630=CARTESIAN_POINT('',(-0.00240202015683311,-0.010827350493292,-0.00718122238517345));
#22631=CARTESIAN_POINT('',(-0.001412710359333,-0.0109470347446187,-0.00743934236637099));
#22632=CARTESIAN_POINT('',(0.000588254796825264,-0.0111793347161375,-0.00754940017546519));
#22633=CARTESIAN_POINT('',(0.00159991015548341,-0.0112919504363294,-0.00740133800336183));
#22634=CARTESIAN_POINT('',(0.00348540910596414,-0.0115101133455787,-0.00672245957268514));
#22635=CARTESIAN_POINT('',(0.00435925269778671,-0.0116156605346359,-0.0061916433141118));
#22636=CARTESIAN_POINT('',(0.00583079226587553,-0.0118196863816156,-0.00483129248351225));
#22637=CARTESIAN_POINT('',(0.00642848824214178,-0.011918165039538,-0.00400175791148602));
#22638=CARTESIAN_POINT('',(0.00725311197626499,-0.0121080538242482,-0.00217529198500112));
#22639=CARTESIAN_POINT('',(0.00748003973412194,-0.0121994639510358,-0.00117836063054243));
#22640=CARTESIAN_POINT('',(0.00752720251438917,-0.0123752156734764,0.000825075965572551));
#22641=CARTESIAN_POINT('',(0.00734743753679946,-0.0124595572691293,0.00183158120722885));
#22642=CARTESIAN_POINT('',(0.00660967315301099,-0.0126211719293004,0.00369482731480231));
#22643=CARTESIAN_POINT('',(0.00605167374681224,-0.0126984449938185,0.00455156818071947));
#22644=CARTESIAN_POINT('',(0.00464577651791156,-0.01284592259172,0.00597965623972475));
#22645=CARTESIAN_POINT('',(0.00379787869520962,-0.0129161271251034,0.00655100343281287));
#22646=CARTESIAN_POINT('',(0.00194641413906699,-0.0130494676607354,0.00731785484009764));
#22647=CARTESIAN_POINT('',(0.000942847405626288,-0.0131126036629839,0.0075133590542943));
#22648=CARTESIAN_POINT('',(-0.00106108222292979,-0.0132318071363463,0.00749757530996088));
#22649=CARTESIAN_POINT('',(-0.00206144511804517,-0.0132878746074602,0.00728628735143079));
#22650=CARTESIAN_POINT('',(-0.0039005997775809,-0.013392941018553,0.00649036502215181));
#22651=CARTESIAN_POINT('',(-0.00473939154200124,-0.013441939958532,0.00590573065140291));
#22652=CARTESIAN_POINT('',(-0.00612262121471807,-0.0135328693073553,0.00445567894540711));
#22653=CARTESIAN_POINT('',(-0.00666705912301456,-0.0135747997161996,0.00359026161016021));
#22654=CARTESIAN_POINT('',(-0.00737537285278311,-0.0136515920027533,0.00171560628916551));
#22655=CARTESIAN_POINT('',(-0.00753924867425516,-0.0136864538804628,0.000706368303417708));
#22656=CARTESIAN_POINT('',(-0.00746056657181117,-0.013749109104747,-0.00129600594118867));
#22657=CARTESIAN_POINT('',(-0.00721800864789512,-0.0137769024513216,-0.00228914220004726));
#22658=CARTESIAN_POINT('',(-0.00679130034245831,-0.0138011615323289,-0.00319589927071015));
#22659=CARTESIAN_POINT('',(-0.00713767358234481,-0.00990699069817707,-0.00231941096831691));
#22660=CARTESIAN_POINT('',(-0.00682799175571029,-0.0100443462773407,-0.00327241490901377));
#22661=CARTESIAN_POINT('',(-0.00632495883391112,-0.010178167590937,-0.00416232274624161));
#22662=CARTESIAN_POINT('',(-0.00501163213059911,-0.0104387416869948,-0.00567566032629884));
#22663=CARTESIAN_POINT('',(-0.00420133834908628,-0.0105654944694563,-0.00629909006912824));
#22664=CARTESIAN_POINT('',(-0.00240181802234349,-0.0108119315032446,-0.00718061807187592));
#22665=CARTESIAN_POINT('',(-0.00141259147711352,-0.0109316157545713,-0.00743871633179419));
#22666=CARTESIAN_POINT('',(0.000588205294083671,-0.01116391572609,-0.00754876487931786));
#22667=CARTESIAN_POINT('',(0.0015997755200509,-0.011276531446282,-0.00740071516692327));
#22668=CARTESIAN_POINT('',(0.00348511580226776,-0.0114946943555312,-0.00672189386513648));
#22669=CARTESIAN_POINT('',(0.00435888585851739,-0.0116002415445884,-0.0061911222757443));
#22670=CARTESIAN_POINT('',(0.00583030159379877,-0.0118042673915681,-0.00483088592121192));
#22671=CARTESIAN_POINT('',(0.00642794727283052,-0.0119027460494905,-0.00400142115607174));
#22672=CARTESIAN_POINT('',(0.00725250161332388,-0.0120926348342006,-0.00217510893011129));
#22673=CARTESIAN_POINT('',(0.00747941027478551,-0.0121840449609883,-0.00117826146929103));
#22674=CARTESIAN_POINT('',(0.00752656908621655,-0.0123597966834289,0.00082500653388659));
#22675=CARTESIAN_POINT('',(0.00734681923618598,-0.0124441382790818,0.00183142707624395));
#22676=CARTESIAN_POINT('',(0.00660911693665054,-0.0126057529392528,0.00369451638817191));
#22677=CARTESIAN_POINT('',(0.00605116448714566,-0.0126830260037709,0.00455118515774251));
#22678=CARTESIAN_POINT('',(0.00464538556712678,-0.0128305036016724,0.00597915304046611));
#22679=CARTESIAN_POINT('',(0.00379755909661278,-0.0129007081350558,0.00655045215361912));
#22680=CARTESIAN_POINT('',(0.00194625034467605,-0.0130340486706877,0.00731723902892344));
#22681=CARTESIAN_POINT('',(0.000942768063253332,-0.0130971846729363,0.00751272679107474));
#22682=CARTESIAN_POINT('',(-0.00106099293087578,-0.0132163881462987,0.00749694437497293));
#22683=CARTESIAN_POINT('',(-0.00206127164358217,-0.0132724556174126,0.00728567419671981));
#22684=CARTESIAN_POINT('',(-0.00390027153481281,-0.0133775220285054,0.00648981884579376));
#22685=CARTESIAN_POINT('',(-0.00473899271333706,-0.0134265209684845,0.00590523367312083));
#22686=CARTESIAN_POINT('',(-0.00612210598468935,-0.0135174503173078,0.00445530399168868));
#22687=CARTESIAN_POINT('',(-0.00666649807751738,-0.013559380726152,0.00358995948292945));
#22688=CARTESIAN_POINT('',(-0.00737475220136054,-0.0136361730127058,0.00171546191768691));
#22689=CARTESIAN_POINT('',(-0.00753861423237565,-0.0136710348904153,0.000706308861203582));
#22690=CARTESIAN_POINT('',(-0.00745993875117777,-0.0137336901146995,-0.0012958968798643));
#22691=CARTESIAN_POINT('',(-0.00721740123896477,-0.0137614834612743,-0.00228894956444885));
#22692=CARTESIAN_POINT('',(-0.0067907288418301,-0.0137857425422816,-0.00319563032980799));
#22693=CARTESIAN_POINT('',(-0.0071364895837481,-0.00989161587683944,-0.00231902622400212));
#22694=CARTESIAN_POINT('',(-0.0068268591271915,-0.0100289714560031,-0.00327187208023133));
#22695=CARTESIAN_POINT('',(-0.00632390964858522,-0.0101627927695994,-0.00416163229938468));
#22696=CARTESIAN_POINT('',(-0.00501080080014649,-0.0104233668656572,-0.00567471884672791));
#22697=CARTESIAN_POINT('',(-0.00420064143031404,-0.0105501196481187,-0.00629804517491777));
#22698=CARTESIAN_POINT('',(-0.00240141960833152,-0.0107965566819069,-0.00717942694963944));
#22699=CARTESIAN_POINT('',(-0.00141235715618145,-0.0109162409332336,-0.00743748239617125));
#22700=CARTESIAN_POINT('',(0.000588107722482121,-0.0111485409047524,-0.00754751268882177));
#22701=CARTESIAN_POINT('',(0.00159951014899562,-0.0112611566249443,-0.00739948753494049));
#22702=CARTESIAN_POINT('',(0.00348453769062233,-0.0114793195341935,-0.00672077883615515));
#22703=CARTESIAN_POINT('',(0.00435816280573553,-0.0115848667232507,-0.0061900952912511));
#22704=CARTESIAN_POINT('',(0.00582933446230616,-0.0117888925702303,-0.00483008457297351));
#22705=CARTESIAN_POINT('',(0.00642688100376357,-0.0118873712281527,-0.00400075739959997));
#22706=CARTESIAN_POINT('',(0.00725129856703243,-0.0120772600128628,-0.00217474812264493));
#22707=CARTESIAN_POINT('',(0.00747816958884387,-0.0121686701396505,-0.00117806601906343));
#22708=CARTESIAN_POINT('',(0.00752532057756267,-0.012344421862091,0.000824869681652156));
#22709=CARTESIAN_POINT('',(0.00734560054447003,-0.0124287634577439,0.00183112327878624));
#22710=CARTESIAN_POINT('',(0.00660802061512669,-0.0125903781179149,0.00369390354111906));
#22711=CARTESIAN_POINT('',(0.00605016071887598,-0.012667651182433,0.00455043020631779));
#22712=CARTESIAN_POINT('',(0.00464461498972096,-0.0128151287803345,0.00597816121746836));
#22713=CARTESIAN_POINT('',(0.00379692915681664,-0.0128853333137179,0.00654936556342019));
#22714=CARTESIAN_POINT('',(0.00194592750031362,-0.0130186738493498,0.00731602524397766));
#22715=CARTESIAN_POINT('',(0.000942611676714912,-0.0130818098515984,0.0075114805785833));
#22716=CARTESIAN_POINT('',(-0.00106081693317474,-0.0132010133249608,0.00749570078047156));
#22717=CARTESIAN_POINT('',(-0.00206092971946568,-0.0132570807960746,0.00728446564775417));
#22718=CARTESIAN_POINT('',(-0.00389962455705868,-0.0133621472071675,0.006488742313459));
#22719=CARTESIAN_POINT('',(-0.00473820660836074,-0.0134111461471466,0.00590425411188122));
#22720=CARTESIAN_POINT('',(-0.00612109044863111,-0.0135020754959699,0.00445456494504928));
#22721=CARTESIAN_POINT('',(-0.00666539223759941,-0.0135440059048142,0.00358936397979514));
#22722=CARTESIAN_POINT('',(-0.00737352887611922,-0.013620798191368,0.00171517735655088));
#22723=CARTESIAN_POINT('',(-0.00753736372567072,-0.0136556600690776,0.000706191698560759));
#22724=CARTESIAN_POINT('',(-0.00745870129517602,-0.0137183152933619,-0.00129568191625332));
#22725=CARTESIAN_POINT('',(-0.00721620401512981,-0.0137461086399366,-0.00228856987307729));
#22726=CARTESIAN_POINT('',(-0.00678960239449027,-0.013770367720944,-0.00319510023806557));
#22727=CARTESIAN_POINT('',(-0.00586854477794281,-0.0138049051783931,-0.00232352128445575));
#22728=CARTESIAN_POINT('',(-0.00647608624973171,-0.0137551635056439,-0.000786833552677216));
#22729=CARTESIAN_POINT('',(-0.00641918266558093,-0.0136285038708237,0.00277611211943972));
#22730=CARTESIAN_POINT('',(-0.00257506117324275,-0.0133569855506279,0.00650403957094241));
#22731=CARTESIAN_POINT('',(0.00277796776553595,-0.0130039383624667,0.00641940533627276));
#22732=CARTESIAN_POINT('',(0.00650363167066124,-0.0125693623063402,0.00257497225928561));
#22733=CARTESIAN_POINT('',(0.00641943847793923,-0.0120532573822484,-0.00277789137493516));
#22734=CARTESIAN_POINT('',(0.00257518666651457,-0.0114556235901914,-0.0065039899999209));
#22735=CARTESIAN_POINT('',(-0.00277899926821046,-0.0107764609301692,-0.00641793340392155));
#22736=CARTESIAN_POINT('',(-0.00525948636061672,-0.0102693332448443,-0.0038596124225381));
#22737=CARTESIAN_POINT('',(-0.00586854353305237,-0.010002181257521,-0.00232352483973746));
#22738=CARTESIAN_POINT('',(-0.00586720610780115,-0.0100021881219798,-0.0023229945466064));
#22739=CARTESIAN_POINT('',(-0.00586854353315033,-0.0100021880910911,-0.00232352483977624));
#22740=CARTESIAN_POINT('',(-0.00586854666154146,-0.0101580986507601,-0.00232352603135712));
#22741=CARTESIAN_POINT('',(-0.00598863875979985,-0.0104699172300717,-0.00237107384600943));
#22742=CARTESIAN_POINT('',(-0.00642351653109598,-0.0106636552715684,-0.00254325427496914));
#22743=CARTESIAN_POINT('',(-0.00685839433219838,-0.0104699172424568,-0.00271543469247471));
#22744=CARTESIAN_POINT('',(-0.00697848647290429,-0.0101580986499977,-0.00276298249495351));
#22745=CARTESIAN_POINT('',(-0.00697848962230257,-0.0100021880761874,-0.00276298368595471));
#22746=CARTESIAN_POINT('',(-0.00697689923797853,-0.0100021880392446,-0.00276235310573588));
#22747=CARTESIAN_POINT('',(-0.00697848962239398,-0.0100021820184533,-0.00276298368599091));
#22748=CARTESIAN_POINT('',(-0.00625423868271113,-0.0102693340114975,-0.00458959897989776));
#22749=CARTESIAN_POINT('',(-0.00330460534139247,-0.0107764617076857,-0.00763178778113441));
#22750=CARTESIAN_POINT('',(0.00306224359742731,-0.0114556243822671,-0.00773412112575933));
#22751=CARTESIAN_POINT('',(0.00763357757233496,-0.0120532581871476,-0.00330328777955172));
#22752=CARTESIAN_POINT('',(0.00773369497252947,-0.0125693631223272,0.0030619887676494));
#22753=CARTESIAN_POINT('',(0.00330337849061272,-0.0130039391878057,0.00763353821745889));
#22754=CARTESIAN_POINT('',(-0.00306209462755998,-0.0133569863835833,0.00773417996973019));
#22755=CARTESIAN_POINT('',(-0.0076332734872252,-0.0136285047096598,0.00330117174949463));
#22756=CARTESIAN_POINT('',(-0.00770093960740274,-0.0137551643472433,-0.000935651021456268));
#22757=CARTESIAN_POINT('',(-0.00697849091759819,-0.0138049060210849,-0.00276297992488766));
#22758=CARTESIAN_POINT('',(-0.0071364895837481,-0.00998404147970407,-0.00231902622400212));
#22759=CARTESIAN_POINT('',(-0.0068268591271915,-0.0101213970588677,-0.00327187208023133));
#22760=CARTESIAN_POINT('',(-0.00632390964858522,-0.010255218372464,-0.00416163229938468));
#22761=CARTESIAN_POINT('',(-0.00501080080014649,-0.0105157924685218,-0.00567471884672791));
#22762=CARTESIAN_POINT('',(-0.00420064143031404,-0.0106425452509834,-0.00629804517491777));
#22763=CARTESIAN_POINT('',(-0.00240141960833152,-0.0108889822847717,-0.00717942694963944));
#22764=CARTESIAN_POINT('',(-0.00141235715618145,-0.0110086665360985,-0.00743748239617125));
#22765=CARTESIAN_POINT('',(0.000588107722482121,-0.0112409665076173,-0.00754751268882177));
#22766=CARTESIAN_POINT('',(0.00159951014899562,-0.0113535822278093,-0.00739948753494049));
#22767=CARTESIAN_POINT('',(0.00348453769062233,-0.0115717451370586,-0.00672077883615515));
#22768=CARTESIAN_POINT('',(0.00435816280573553,-0.0116772923261159,-0.0061900952912511));
#22769=CARTESIAN_POINT('',(0.00582933446230616,-0.0118813181730956,-0.00483008457297351));
#22770=CARTESIAN_POINT('',(0.00642688100376358,-0.0119797968310181,-0.00400075739959997));
#22771=CARTESIAN_POINT('',(0.00725129856703243,-0.0121696856157283,-0.00217474812264493));
#22772=CARTESIAN_POINT('',(0.00747816958884387,-0.0122610957425161,-0.00117806601906343));
#22773=CARTESIAN_POINT('',(0.00752532057756267,-0.0124368474649567,0.000824869681652156));
#22774=CARTESIAN_POINT('',(0.00734560054447003,-0.0125211890606097,0.00183112327878624));
#22775=CARTESIAN_POINT('',(0.00660802061512669,-0.0126828037207808,0.00369390354111907));
#22776=CARTESIAN_POINT('',(0.00605016071887599,-0.0127600767852989,0.00455043020631779));
#22777=CARTESIAN_POINT('',(0.00464461498972096,-0.0129075543832005,0.00597816121746836));
#22778=CARTESIAN_POINT('',(0.00379692915681664,-0.0129777589165839,0.00654936556342019));
#22779=CARTESIAN_POINT('',(0.00194592750031363,-0.0131110994522158,0.00731602524397766));
#22780=CARTESIAN_POINT('',(0.000942611676714919,-0.0131742354544644,0.00751148057858331));
#22781=CARTESIAN_POINT('',(-0.00106081693317473,-0.0132934389278268,0.00749570078047156));
#22782=CARTESIAN_POINT('',(-0.00206092971946568,-0.0133495063989406,0.00728446564775417));
#22783=CARTESIAN_POINT('',(-0.00389962455705868,-0.0134545728100334,0.006488742313459));
#22784=CARTESIAN_POINT('',(-0.00473820660836074,-0.0135035717500124,0.00590425411188122));
#22785=CARTESIAN_POINT('',(-0.00612109044863111,-0.0135945010988356,0.00445456494504928));
#22786=CARTESIAN_POINT('',(-0.00666539223759941,-0.0136364315076798,0.00358936397979514));
#22787=CARTESIAN_POINT('',(-0.00737352887611922,-0.0137132237942334,0.00171517735655088));
#22788=CARTESIAN_POINT('',(-0.00753736372567072,-0.0137480856719428,0.000706191698560759));
#22789=CARTESIAN_POINT('',(-0.00745870129517602,-0.0138107408962268,-0.00129568191625332));
#22790=CARTESIAN_POINT('',(-0.00721620401512982,-0.0138385342428014,-0.00228856987307729));
#22791=CARTESIAN_POINT('',(-0.00678960239449027,-0.0138627933238085,-0.00319510023806557));
#22792=CARTESIAN_POINT('',(-0.00713767358234481,-0.00996866665836644,-0.00231941096831692));
#22793=CARTESIAN_POINT('',(-0.00682799175571029,-0.0101060222375301,-0.00327241490901377));
#22794=CARTESIAN_POINT('',(-0.00632495883391112,-0.0102398435511264,-0.00416232274624161));
#22795=CARTESIAN_POINT('',(-0.00501163213059911,-0.0105004176471842,-0.00567566032629884));
#22796=CARTESIAN_POINT('',(-0.00420133834908628,-0.0106271704296457,-0.00629909006912824));
#22797=CARTESIAN_POINT('',(-0.00240181802234349,-0.0108736074634341,-0.00718061807187592));
#22798=CARTESIAN_POINT('',(-0.00141259147711352,-0.0109932917147608,-0.00743871633179419));
#22799=CARTESIAN_POINT('',(0.000588205294083671,-0.0112255916862796,-0.00754876487931786));
#22800=CARTESIAN_POINT('',(0.00159977552005091,-0.0113382074064716,-0.00740071516692327));
#22801=CARTESIAN_POINT('',(0.00348511580226776,-0.0115563703157209,-0.00672189386513648));
#22802=CARTESIAN_POINT('',(0.00435888585851739,-0.0116619175047782,-0.0061911222757443));
#22803=CARTESIAN_POINT('',(0.00583030159379877,-0.0118659433517579,-0.00483088592121192));
#22804=CARTESIAN_POINT('',(0.00642794727283052,-0.0119644220096804,-0.00400142115607174));
#22805=CARTESIAN_POINT('',(0.00725250161332388,-0.0121543107943906,-0.00217510893011129));
#22806=CARTESIAN_POINT('',(0.0074794102747855,-0.0122457209211783,-0.00117826146929103));
#22807=CARTESIAN_POINT('',(0.00752656908621655,-0.012421472643619,0.000825006533886589));
#22808=CARTESIAN_POINT('',(0.00734681923618598,-0.0125058142392719,0.00183142707624395));
#22809=CARTESIAN_POINT('',(0.00660911693665054,-0.012667428899443,0.00369451638817191));
#22810=CARTESIAN_POINT('',(0.00605116448714566,-0.0127447019639612,0.00455118515774251));
#22811=CARTESIAN_POINT('',(0.00464538556712678,-0.0128921795618627,0.00597915304046612));
#22812=CARTESIAN_POINT('',(0.00379755909661278,-0.0129623840952461,0.00655045215361912));
#22813=CARTESIAN_POINT('',(0.00194625034467606,-0.0130957246308781,0.00731723902892344));
#22814=CARTESIAN_POINT('',(0.00094276806325334,-0.0131588606331266,0.00751272679107474));
#22815=CARTESIAN_POINT('',(-0.00106099293087577,-0.013278064106489,0.00749694437497293));
#22816=CARTESIAN_POINT('',(-0.00206127164358217,-0.0133341315776028,0.00728567419671981));
#22817=CARTESIAN_POINT('',(-0.00390027153481281,-0.0134391979886957,0.00648981884579376));
#22818=CARTESIAN_POINT('',(-0.00473899271333706,-0.0134881969286747,0.00590523367312083));
#22819=CARTESIAN_POINT('',(-0.00612210598468935,-0.0135791262774979,0.00445530399168868));
#22820=CARTESIAN_POINT('',(-0.00666649807751738,-0.0136210566863421,0.00358995948292946));
#22821=CARTESIAN_POINT('',(-0.00737475220136054,-0.0136978489728957,0.00171546191768691));
#22822=CARTESIAN_POINT('',(-0.00753861423237565,-0.0137327108506051,0.000706308861203582));
#22823=CARTESIAN_POINT('',(-0.00745993875117777,-0.0137953660748891,-0.0012958968798643));
#22824=CARTESIAN_POINT('',(-0.00721740123896477,-0.0138231594214637,-0.00228894956444885));
#22825=CARTESIAN_POINT('',(-0.0067907288418301,-0.0138474185024709,-0.00319563032980799));
#22826=CARTESIAN_POINT('',(-0.00713827428147907,-0.0099532476683191,-0.00231960616751517));
#22827=CARTESIAN_POINT('',(-0.00682856639234631,-0.0100906032474828,-0.00327269031202571));
#22828=CARTESIAN_POINT('',(-0.00632549113582321,-0.010224424561079,-0.00416267304296523));
#22829=CARTESIAN_POINT('',(-0.00501205390431114,-0.0104849986571369,-0.00567613798392846));
#22830=CARTESIAN_POINT('',(-0.00420169192932218,-0.0106117514395984,-0.00629962019395218));
#22831=CARTESIAN_POINT('',(-0.00240202015683311,-0.0108581884733867,-0.00718122238517345));
#22832=CARTESIAN_POINT('',(-0.001412710359333,-0.0109778727247135,-0.007439342366371));
#22833=CARTESIAN_POINT('',(0.000588254796825264,-0.0112101726962322,-0.00754940017546519));
#22834=CARTESIAN_POINT('',(0.00159991015548341,-0.0113227884164243,-0.00740133800336183));
#22835=CARTESIAN_POINT('',(0.00348540910596414,-0.0115409513256735,-0.00672245957268514));
#22836=CARTESIAN_POINT('',(0.00435925269778671,-0.0116464985147308,-0.0061916433141118));
#22837=CARTESIAN_POINT('',(0.00583079226587553,-0.0118505243617105,-0.00483129248351225));
#22838=CARTESIAN_POINT('',(0.00642848824214178,-0.011949003019633,-0.00400175791148602));
#22839=CARTESIAN_POINT('',(0.00725311197626499,-0.0121388918043431,-0.00217529198500112));
#22840=CARTESIAN_POINT('',(0.00748003973412194,-0.0122303019311308,-0.00117836063054243));
#22841=CARTESIAN_POINT('',(0.00752720251438918,-0.0124060536535715,0.000825075965572551));
#22842=CARTESIAN_POINT('',(0.00734743753679946,-0.0124903952492244,0.00183158120722885));
#22843=CARTESIAN_POINT('',(0.00660967315301099,-0.0126520099093955,0.00369482731480231));
#22844=CARTESIAN_POINT('',(0.00605167374681224,-0.0127292829739137,0.00455156818071947));
#22845=CARTESIAN_POINT('',(0.00464577651791156,-0.0128767605718152,0.00597965623972475));
#22846=CARTESIAN_POINT('',(0.00379787869520962,-0.0129469651051986,0.00655100343281287));
#22847=CARTESIAN_POINT('',(0.00194641413906699,-0.0130803056408305,0.00731785484009764));
#22848=CARTESIAN_POINT('',(0.000942847405626291,-0.0131434416430791,0.0075133590542943));
#22849=CARTESIAN_POINT('',(-0.00106108222292979,-0.0132626451164415,0.00749757530996088));
#22850=CARTESIAN_POINT('',(-0.00206144511804517,-0.0133187125875553,0.00728628735143079));
#22851=CARTESIAN_POINT('',(-0.0039005997775809,-0.0134237789986481,0.00649036502215181));
#22852=CARTESIAN_POINT('',(-0.00473939154200124,-0.0134727779386271,0.00590573065140291));
#22853=CARTESIAN_POINT('',(-0.00612262121471807,-0.0135637072874504,0.00445567894540711));
#22854=CARTESIAN_POINT('',(-0.00666705912301456,-0.0136056376962946,0.00359026161016021));
#22855=CARTESIAN_POINT('',(-0.00737537285278311,-0.0136824299828483,0.00171560628916551));
#22856=CARTESIAN_POINT('',(-0.00753924867425516,-0.0137172918605577,0.000706368303417708));
#22857=CARTESIAN_POINT('',(-0.00746056657181117,-0.0137799470848417,-0.00129600594118867));
#22858=CARTESIAN_POINT('',(-0.00721800864789512,-0.0138077404314164,-0.00228914220004726));
#22859=CARTESIAN_POINT('',(-0.00679130034245831,-0.0138319995124236,-0.00319589927071015));
#22860=CARTESIAN_POINT('',(-0.00713827428147908,-0.00978191608530591,-0.00231960616751517));
#22861=CARTESIAN_POINT('',(-0.00682856639234631,-0.00991927166446956,-0.0032726903120257));
#22862=CARTESIAN_POINT('',(-0.00632549113582322,-0.0100530929780658,-0.00416267304296523));
#22863=CARTESIAN_POINT('',(-0.00501205390431114,-0.0103136670741236,-0.00567613798392846));
#22864=CARTESIAN_POINT('',(-0.00420169192932218,-0.0104404198565851,-0.00629962019395217));
#22865=CARTESIAN_POINT('',(-0.0024020201568331,-0.0106868568903732,-0.00718122238517344));
#22866=CARTESIAN_POINT('',(-0.001412710359333,-0.0108065411416999,-0.007439342366371));
#22867=CARTESIAN_POINT('',(0.000588254796825258,-0.0110388411132185,-0.0075494001754652));
#22868=CARTESIAN_POINT('',(0.00159991015548341,-0.0111514568334104,-0.00740133800336183));
#22869=CARTESIAN_POINT('',(0.00348540910596413,-0.0113696197426594,-0.00672245957268514));
#22870=CARTESIAN_POINT('',(0.00435925269778671,-0.0114751669317165,-0.00619164331411181));
#22871=CARTESIAN_POINT('',(0.00583079226587553,-0.011679192778696,-0.00483129248351226));
#22872=CARTESIAN_POINT('',(0.00642848824214178,-0.0117776714366183,-0.00400175791148603));
#22873=CARTESIAN_POINT('',(0.00725311197626498,-0.0119675602213283,-0.00217529198500112));
#22874=CARTESIAN_POINT('',(0.00748003973412194,-0.0120589703481159,-0.00117836063054244));
#22875=CARTESIAN_POINT('',(0.00752720251438918,-0.0122347220705563,0.000825075965572557));
#22876=CARTESIAN_POINT('',(0.00734743753679946,-0.0123190636662091,0.00183158120722885));
#22877=CARTESIAN_POINT('',(0.00660967315301099,-0.01248067832638,0.00369482731480231));
#22878=CARTESIAN_POINT('',(0.00605167374681224,-0.0125579513908981,0.00455156818071948));
#22879=CARTESIAN_POINT('',(0.00464577651791155,-0.0127054289887995,0.00597965623972473));
#22880=CARTESIAN_POINT('',(0.00379787869520963,-0.0127756335221828,0.00655100343281285));
#22881=CARTESIAN_POINT('',(0.00194641413906698,-0.0129089740578147,0.00731785484009762));
#22882=CARTESIAN_POINT('',(0.00094284740562626,-0.0129721100600632,0.0075133590542943));
#22883=CARTESIAN_POINT('',(-0.00106108222292982,-0.0130913135334257,0.00749757530996088));
#22884=CARTESIAN_POINT('',(-0.00206144511804518,-0.0131473810045395,0.00728628735143079));
#22885=CARTESIAN_POINT('',(-0.00390059977758088,-0.0132524474156325,0.00649036502215181));
#22886=CARTESIAN_POINT('',(-0.00473939154200123,-0.0133014463556117,0.00590573065140293));
#22887=CARTESIAN_POINT('',(-0.00612262121471807,-0.0133923757044352,0.00445567894540711));
#22888=CARTESIAN_POINT('',(-0.00666705912301456,-0.0134343061132796,0.0035902616101602));
#22889=CARTESIAN_POINT('',(-0.0073753728527831,-0.0135110983998337,0.00171560628916551));
#22890=CARTESIAN_POINT('',(-0.00753924867425516,-0.0135459602775433,0.000706368303417707));
#22891=CARTESIAN_POINT('',(-0.00746056657181116,-0.013608615501828,-0.00129600594118867));
#22892=CARTESIAN_POINT('',(-0.00721800864789512,-0.013636408848403,-0.00228914220004726));
#22893=CARTESIAN_POINT('',(-0.00679130034245831,-0.0136606679294106,-0.00319589927071014));
#22894=CARTESIAN_POINT('',(-0.00707685460303241,-0.00962600349234004,-0.00229964763701973));
#22895=CARTESIAN_POINT('',(-0.00676981152589942,-0.00976335907150373,-0.00324453118298499));
#22896=CARTESIAN_POINT('',(-0.00627106486747605,-0.00989718038509995,-0.00412685625732547));
#22897=CARTESIAN_POINT('',(-0.00496892881174377,-0.0101577544811575,-0.00562729892899101));
#22898=CARTESIAN_POINT('',(-0.00416553941443487,-0.0102845072636188,-0.00624541652631607));
#22899=CARTESIAN_POINT('',(-0.00238135251366929,-0.0105309442974066,-0.00711943316941079));
#22900=CARTESIAN_POINT('',(-0.00140055501021261,-0.0106506285487331,-0.00737533221518044));
#22901=CARTESIAN_POINT('',(0.000583193290494599,-0.0108829285202512,-0.00748444305656528));
#22902=CARTESIAN_POINT('',(0.00158614408774513,-0.0109955442404428,-0.00733765485218046));
#22903=CARTESIAN_POINT('',(0.00345541968581831,-0.0112137071496912,-0.00666461767854607));
#22904=CARTESIAN_POINT('',(0.00432174448664098,-0.011319254338748,-0.00613836870929649));
#22905=CARTESIAN_POINT('',(0.00578062252289037,-0.0115232801857269,-0.00478972271200753));
#22906=CARTESIAN_POINT('',(0.00637317575831709,-0.0116217588436489,-0.00396732568396815));
#22907=CARTESIAN_POINT('',(0.00719070420265566,-0.0118116476283582,-0.00215657517348927));
#22908=CARTESIAN_POINT('',(0.00741567941156751,-0.0119030577551455,-0.00116822169104975));
#22909=CARTESIAN_POINT('',(0.00746243639028041,-0.0120788094775854,0.000817976784663933));
#22910=CARTESIAN_POINT('',(0.00728421816008147,-0.0121631510732379,0.00181582177793811));
#22911=CARTESIAN_POINT('',(0.00655280170429841,-0.0123247657334084,0.00366303600269487));
#22912=CARTESIAN_POINT('',(0.00599960347871429,-0.0124020387979262,0.00451240523417745));
#22913=CARTESIAN_POINT('',(0.00460580297688281,-0.0125495163958273,0.00592820563009794));
#22914=CARTESIAN_POINT('',(0.00376520070063544,-0.0126197209292105,0.00649463679453584));
#22915=CARTESIAN_POINT('',(0.00192966665559529,-0.0127530614648423,0.00725489000105184));
#22916=CARTESIAN_POINT('',(0.000934734886802496,-0.0128161974670908,0.00744871204312994));
#22917=CARTESIAN_POINT('',(-0.00105195237916533,-0.0129354009404534,0.00743306410648104));
#22918=CARTESIAN_POINT('',(-0.00204370787634037,-0.0129914684115673,0.00722359412775403));
#22919=CARTESIAN_POINT('',(-0.00386703794251527,-0.0130965348226607,0.00643452013346544));
#22920=CARTESIAN_POINT('',(-0.00469861251151514,-0.0131455337626401,0.00585491611790385));
#22921=CARTESIAN_POINT('',(-0.00606994049506089,-0.0132364631114643,0.00441734105626232));
#22922=CARTESIAN_POINT('',(-0.00660969390960677,-0.0132783935203091,0.00355937001018238));
#22923=CARTESIAN_POINT('',(-0.00731191311291048,-0.0133551858068643,0.00170084474001979));
#22924=CARTESIAN_POINT('',(-0.00747437890166831,-0.0133900476845746,0.000700290515937141));
#22925=CARTESIAN_POINT('',(-0.00739637380170993,-0.0134527029088608,-0.00128485474903298));
#22926=CARTESIAN_POINT('',(-0.00715590291299373,-0.0134804962554366,-0.00226944578992046));
#22927=CARTESIAN_POINT('',(-0.00673286612337111,-0.0135047553364452,-0.00316840087294414));
#22928=CARTESIAN_POINT('',(-0.00686715470388323,-0.00940550978882296,-0.00223150495151719));
#22929=CARTESIAN_POINT('',(-0.00656920986402103,-0.00954286536798665,-0.00314838990270961));
#22930=CARTESIAN_POINT('',(-0.00608524196393579,-0.00967668668158289,-0.00400457010203361));
#22931=CARTESIAN_POINT('',(-0.00482169053582163,-0.00993726077764047,-0.00546055196525008));
#22932=CARTESIAN_POINT('',(-0.00404210700779271,-0.0100640135601018,-0.00606035362914253));
#22933=CARTESIAN_POINT('',(-0.00231078876607709,-0.0103104505938897,-0.00690847159094555));
#22934=CARTESIAN_POINT('',(-0.00135905405239039,-0.0104301348452162,-0.0071567878888561));
#22935=CARTESIAN_POINT('',(0.000565912226934413,-0.0106624348167344,-0.00726266558024452));
#22936=CARTESIAN_POINT('',(0.00153914379257251,-0.010775050536926,-0.00712022697372237));
#22937=CARTESIAN_POINT('',(0.00335302940082875,-0.0109932134461746,-0.00646713309910309));
#22938=CARTESIAN_POINT('',(0.0041936834434469,-0.0110987606352314,-0.00595647783100596));
#22939=CARTESIAN_POINT('',(0.00560933230596968,-0.0113027864822104,-0.00464779463435138));
#22940=CARTESIAN_POINT('',(0.00618432712587431,-0.0114012651401325,-0.00384976670579392));
#22941=CARTESIAN_POINT('',(0.00697763073560119,-0.0115911539248419,-0.00209267198178111));
#22942=CARTESIAN_POINT('',(0.00719593952542345,-0.0116825640516293,-0.00113360518632574));
#22943=CARTESIAN_POINT('',(0.00724131101096593,-0.0118583157740692,0.000793738664923998));
#22944=CARTESIAN_POINT('',(0.00706837370668615,-0.0119426573697218,0.00176201572071837));
#22945=CARTESIAN_POINT('',(0.00635863043279213,-0.0121042720298923,0.00355449367373196));
#22946=CARTESIAN_POINT('',(0.00582182446317788,-0.0121815450944102,0.00437869457095119));
#22947=CARTESIAN_POINT('',(0.00446932477096638,-0.0123290226923114,0.00575254226091774));
#22948=CARTESIAN_POINT('',(0.00365363104836911,-0.0123992272256946,0.00630218905366504));
#22949=CARTESIAN_POINT('',(0.0018724871703906,-0.0125325677613264,0.00703991459362902));
#22950=CARTESIAN_POINT('',(0.000907037015009341,-0.012595703763575,0.00722799334084569));
#22951=CARTESIAN_POINT('',(-0.00102078114276233,-0.0127149072369375,0.00721280908063516));
#22952=CARTESIAN_POINT('',(-0.00198314914515274,-0.0127709747080514,0.00700954607320794));
#22953=CARTESIAN_POINT('',(-0.00375245067005612,-0.0128760411191447,0.0062438537571232));
#22954=CARTESIAN_POINT('',(-0.0045593841925691,-0.012925040059124,0.00568142444846567));
#22955=CARTESIAN_POINT('',(-0.00589007726753176,-0.0130159694079481,0.00428644731519142));
#22956=CARTESIAN_POINT('',(-0.00641383681998144,-0.0130578998167929,0.0034538994905747));
#22957=CARTESIAN_POINT('',(-0.00709524800837267,-0.0131346921033478,0.00165044565872487));
#22958=CARTESIAN_POINT('',(-0.00725289964431421,-0.0131695539810581,0.000679539651491767));
#22959=CARTESIAN_POINT('',(-0.007177205975424,-0.0132322092053439,-0.00124678219753841));
#22960=CARTESIAN_POINT('',(-0.00694386067059226,-0.0132600025519196,-0.00220219803933548));
#22961=CARTESIAN_POINT('',(-0.00653335922005691,-0.013284261632928,-0.00307451547034793));
#22962=CARTESIAN_POINT('',(-0.00671887448318071,-0.00934092867827176,-0.00218332079651008));
#22963=CARTESIAN_POINT('',(-0.00642736306858953,-0.00947828425743542,-0.00308040775147493));
#22964=CARTESIAN_POINT('',(-0.00595384532874271,-0.0096121055710317,-0.00391810073238151));
#22965=CARTESIAN_POINT('',(-0.00471757735246688,-0.00987267966708951,-0.00534264405644659));
#22966=CARTESIAN_POINT('',(-0.00395482711603787,-0.00999943244955104,-0.00592949439960509));
#22967=CARTESIAN_POINT('',(-0.00226089266164871,-0.0102458694833393,-0.00675929922824295));
#22968=CARTESIAN_POINT('',(-0.00132970844368856,-0.0103655537346661,-0.00700225371372232));
#22969=CARTESIAN_POINT('',(0.000553692669704888,-0.0105978537061848,-0.00710584522282366));
#22970=CARTESIAN_POINT('',(0.00150590956513818,-0.0107104694263768,-0.00696648224644565));
#22971=CARTESIAN_POINT('',(0.00328062853598501,-0.0109286323356261,-0.00632749041379919));
#22972=CARTESIAN_POINT('',(0.00410313061139855,-0.0110341795246833,-0.00582786155753075));
#22973=CARTESIAN_POINT('',(0.00548821183203415,-0.011238205371663,-0.00454743632819994));
#22974=CARTESIAN_POINT('',(0.00605079097725621,-0.0113366840295855,-0.00376663995513757));
#22975=CARTESIAN_POINT('',(0.00682696504215606,-0.0115265728142956,-0.00204748560158481));
#22976=CARTESIAN_POINT('',(0.00704055996183384,-0.0116179829410833,-0.00110912762109441));
#22977=CARTESIAN_POINT('',(0.00708495175576022,-0.011793734663524,0.00077659972609268));
#22978=CARTESIAN_POINT('',(0.00691574863000882,-0.0118780762591769,0.00172396909278938));
#22979=CARTESIAN_POINT('',(0.00622133060999841,-0.0120396909193479,0.00347774265687652));
#22980=CARTESIAN_POINT('',(0.00569611571573941,-0.0121169639838661,0.00428414685426696));
#22981=CARTESIAN_POINT('',(0.00437282010607869,-0.0122644415817676,0.00562832950136433));
#22982=CARTESIAN_POINT('',(0.00357473939067698,-0.012334646115151,0.00616610795107126));
#22983=CARTESIAN_POINT('',(0.0018320551686576,-0.0124679866507829,0.006887904025252));
#22984=CARTESIAN_POINT('',(0.000887451662039948,-0.0125311226530315,0.00707192164972581));
#22985=CARTESIAN_POINT('',(-0.000998739750123815,-0.0126503261263939,0.00705706525826911));
#22986=CARTESIAN_POINT('',(-0.00194032765566992,-0.0127063935975077,0.00685819124233861));
#22987=CARTESIAN_POINT('',(-0.00367142523266258,-0.0128114600086006,0.00610903226946734));
#22988=CARTESIAN_POINT('',(-0.00446093490410914,-0.0128604589485796,0.00555874731252656));
#22989=CARTESIAN_POINT('',(-0.00576289475965981,-0.0129513882974029,0.00419389146326531));
#22990=CARTESIAN_POINT('',(-0.00627534494376392,-0.0129933187062471,0.00337932057094484));
#22991=CARTESIAN_POINT('',(-0.00694204264370749,-0.0130701109928008,0.00161480812657567));
#22992=CARTESIAN_POINT('',(-0.00709629015954695,-0.0131049728705102,0.00066486657452696));
#22993=CARTESIAN_POINT('',(-0.0070222309192393,-0.0131676280947944,-0.00121986083819952));
#22994=CARTESIAN_POINT('',(-0.00679392416309219,-0.013195421441369,-0.00215464669887731));
#22995=CARTESIAN_POINT('',(-0.00639228653582991,-0.0132196805223763,-0.00300812846551772));
#22996=CARTESIAN_POINT('',(-0.00642231404177568,-0.00934092867827176,-0.00208695248649585));
#22997=CARTESIAN_POINT('',(-0.00614366947772652,-0.00947828425743542,-0.00294444344900556));
#22998=CARTESIAN_POINT('',(-0.00569105205835654,-0.0096121055710317,-0.00374516199307731));
#22999=CARTESIAN_POINT('',(-0.00450935098575736,-0.00987267966708951,-0.00510682823883964));
#23000=CARTESIAN_POINT('',(-0.00378026733252819,-0.00999943244955104,-0.00566777594053021));
#23001=CARTESIAN_POINT('',(-0.00216110045279195,-0.0102458694833393,-0.00646095450283777));
#23002=CARTESIAN_POINT('',(-0.0012710172262849,-0.0103655537346661,-0.00669318536345474));
#23003=CARTESIAN_POINT('',(0.000529253555245836,-0.0105978537061848,-0.00679220450798197));
#23004=CARTESIAN_POINT('',(0.00143944111026952,-0.0107104694263769,-0.00665899279189221));
#23005=CARTESIAN_POINT('',(0.00313582680629751,-0.0109286323356261,-0.0060482050431914));
#23006=CARTESIAN_POINT('',(0.00392202494730184,-0.0110341795246833,-0.00557062901058033));
#23007=CARTESIAN_POINT('',(0.00524597088416309,-0.011238205371663,-0.00434671971589707));
#23008=CARTESIAN_POINT('',(0.00578371868002002,-0.0113366840295855,-0.00360038645382486));
#23009=CARTESIAN_POINT('',(0.00652563365526577,-0.0115265728142956,-0.00195711284119222));
#23010=CARTESIAN_POINT('',(0.0067298008346546,-0.0116179829410833,-0.00106017249063177));
#23011=CARTESIAN_POINT('',(0.00677223324534879,-0.011793734663524,0.00074232184843004));
#23012=CARTESIAN_POINT('',(0.00661049847665415,-0.0118780762591769,0.0016478758369314));
#23013=CARTESIAN_POINT('',(0.00594673096441099,-0.0120396909193479,0.00332424062316563));
#23014=CARTESIAN_POINT('',(0.00544469822086248,-0.0121169639838661,0.00409505142089849));
#23015=CARTESIAN_POINT('',(0.00417981077630333,-0.0122644415817676,0.00537990398225753));
#23016=CARTESIAN_POINT('',(0.00341695607529269,-0.012334646115151,0.00589394574588371));
#23017=CARTESIAN_POINT('',(0.00175119116519162,-0.0124679866507829,0.00658388288849796));
#23018=CARTESIAN_POINT('',(0.000848280956101175,-0.0125311226530315,0.00675977826748603));
#23019=CARTESIAN_POINT('',(-0.000954656964846769,-0.0126503261263939,0.00674557761353704));
#23020=CARTESIAN_POINT('',(-0.00185468467670427,-0.0127063935975077,0.00655548158059996));
#23021=CARTESIAN_POINT('',(-0.0035093743578755,-0.0128114600086006,0.00583938929415562));
#23022=CARTESIAN_POINT('',(-0.00426403632718924,-0.0128604589485796,0.00531339304064834));
#23023=CARTESIAN_POINT('',(-0.00550852974391592,-0.0129513882974029,0.0040087797594131));
#23024=CARTESIAN_POINT('',(-0.00599836119132888,-0.0129933187062471,0.00323016273168512));
#23025=CARTESIAN_POINT('',(-0.00663563191437715,-0.0130701109928008,0.00154353306227724));
#23026=CARTESIAN_POINT('',(-0.00678307119001246,-0.0131049728705102,0.000635520420597347));
#23027=CARTESIAN_POINT('',(-0.00671228080686991,-0.0131676280947944,-0.00116601811952175));
#23028=CARTESIAN_POINT('',(-0.00649405114809204,-0.013195421441369,-0.00205954401796095));
#23029=CARTESIAN_POINT('',(-0.00611014116737591,-0.0132196805223763,-0.0028753544558573));
#23030=CARTESIAN_POINT('',(-0.00627403382107316,-0.00940550978882296,-0.00203876833148874));
#23031=CARTESIAN_POINT('',(-0.00600182268229503,-0.00954286536798665,-0.00287646129777088));
#23032=CARTESIAN_POINT('',(-0.00555965542316345,-0.00967668668158289,-0.0036586926234252));
#23033=CARTESIAN_POINT('',(-0.00440523780240261,-0.00993726077764048,-0.00498892033003616));
#23034=CARTESIAN_POINT('',(-0.00369298744077334,-0.0100640135601018,-0.00553691671099277));
#23035=CARTESIAN_POINT('',(-0.00211120434836358,-0.0103104505938897,-0.00631178214013517));
#23036=CARTESIAN_POINT('',(-0.00124167161758307,-0.0104301348452162,-0.00653865118832096));
#23037=CARTESIAN_POINT('',(0.000517033998016309,-0.0106624348167344,-0.00663538415056111));
#23038=CARTESIAN_POINT('',(0.00140620688283518,-0.010775050536926,-0.00650524806461549));
#23039=CARTESIAN_POINT('',(0.00306342594145377,-0.0109932134461746,-0.00590856235788749));
#23040=CARTESIAN_POINT('',(0.00383147211525347,-0.0110987606352314,-0.00544201273710513));
#23041=CARTESIAN_POINT('',(0.00512485041022755,-0.0113027864822104,-0.00424636140974563));
#23042=CARTESIAN_POINT('',(0.00565018253140191,-0.0114012651401325,-0.00351725970316852));
#23043=CARTESIAN_POINT('',(0.00637496796182063,-0.0115911539248419,-0.00191192646099593));
#23044=CARTESIAN_POINT('',(0.00657442127106498,-0.0116825640516293,-0.00103569492540045));
#23045=CARTESIAN_POINT('',(0.00661587399014308,-0.0118583157740692,0.000725182909598717));
#23046=CARTESIAN_POINT('',(0.00645787339997682,-0.0119426573697218,0.00160982920900241));
#23047=CARTESIAN_POINT('',(0.00580943114161729,-0.0121042720298923,0.00324748960631018));
#23048=CARTESIAN_POINT('',(0.00531898947342402,-0.0121815450944102,0.00400050370421425));
#23049=CARTESIAN_POINT('',(0.00408330611141565,-0.0123290226923114,0.00525569122270413));
#23050=CARTESIAN_POINT('',(0.00333806441760056,-0.0123992272256946,0.00575786464328994));
#23051=CARTESIAN_POINT('',(0.00171075916345863,-0.0125325677613264,0.00643187232012095));
#23052=CARTESIAN_POINT('',(0.000828695603131796,-0.012595703763575,0.00660370657636615));
#23053=CARTESIAN_POINT('',(-0.000932615572208239,-0.0127149072369375,0.006589833791171));
#23054=CARTESIAN_POINT('',(-0.00181186318722145,-0.0127709747080514,0.00640412674973064));
#23055=CARTESIAN_POINT('',(-0.00342834892048197,-0.0128760411191447,0.00570456780649976));
#23056=CARTESIAN_POINT('',(-0.00416558703872928,-0.012925040059124,0.00519071590470924));
#23057=CARTESIAN_POINT('',(-0.00538134723604398,-0.0130159694079481,0.00391622390748699));
#23058=CARTESIAN_POINT('',(-0.00585986931511135,-0.0130578998167929,0.00315558381205526));
#23059=CARTESIAN_POINT('',(-0.00648242654971197,-0.0131346921033478,0.00150789553012803));
#23060=CARTESIAN_POINT('',(-0.00662646170524521,-0.0131695539810581,0.000620847343632542));
#23061=CARTESIAN_POINT('',(-0.00655730575068521,-0.0132322092053439,-0.00113909676018287));
#23062=CARTESIAN_POINT('',(-0.00634411464059197,-0.0132600025519196,-0.00201199267750278));
#23063=CARTESIAN_POINT('',(-0.00596906848314891,-0.013284261632928,-0.00280896745102709));
#23064=CARTESIAN_POINT('',(-0.00606433392192398,-0.00962600349234004,-0.0019706256459862));
#23065=CARTESIAN_POINT('',(-0.00580122102041663,-0.00976335907150372,-0.00278032001749548));
#23066=CARTESIAN_POINT('',(-0.0053738325196232,-0.00989718038509996,-0.00353640646813335));
#23067=CARTESIAN_POINT('',(-0.00425799952648047,-0.0101577544811575,-0.00482217336629522));
#23068=CARTESIAN_POINT('',(-0.00356955503413119,-0.0102845072636188,-0.00535185381381923));
#23069=CARTESIAN_POINT('',(-0.00204064060077137,-0.0105309442974066,-0.00610082056166993));
#23070=CARTESIAN_POINT('',(-0.00120017065976085,-0.0106506285487331,-0.00632010686199662));
#23071=CARTESIAN_POINT('',(0.000499752934456116,-0.0108829285202512,-0.00641360667424036));
#23072=CARTESIAN_POINT('',(0.00135920658766256,-0.0109955442404428,-0.0062878201861574));
#23073=CARTESIAN_POINT('',(0.0029610356564642,-0.0112137071496912,-0.00571107777844453));
#23074=CARTESIAN_POINT('',(0.00370341107205939,-0.011319254338748,-0.0052601218588146));
#23075=CARTESIAN_POINT('',(0.00495356019330686,-0.0115232801857269,-0.00410443333208948));
#23076=CARTESIAN_POINT('',(0.00546133389895913,-0.0116217588436489,-0.00339970072499429));
#23077=CARTESIAN_POINT('',(0.00616189449476617,-0.0118116476283582,-0.00184802326928778));
#23078=CARTESIAN_POINT('',(0.00635468138492093,-0.0119030577551455,-0.00100107842067645));
#23079=CARTESIAN_POINT('',(0.0063947486108286,-0.0120788094775854,0.000700944789858772));
#23080=CARTESIAN_POINT('',(0.0062420289465815,-0.0121631510732379,0.00155602315178267));
#23081=CARTESIAN_POINT('',(0.005615259870111,-0.0123247657334084,0.00313894727734728));
#23082=CARTESIAN_POINT('',(0.00514121045788761,-0.0124020387979262,0.00386679304098799));
#23083=CARTESIAN_POINT('',(0.00394682790549922,-0.0125495163958273,0.00508002785352392));
#23084=CARTESIAN_POINT('',(0.00322649476533423,-0.0126197209292105,0.00556541690241914));
#23085=CARTESIAN_POINT('',(0.00165357967825393,-0.0127530614648423,0.00621689691269813));
#23086=CARTESIAN_POINT('',(0.000800997731338632,-0.0128161974670908,0.00638298787408191));
#23087=CARTESIAN_POINT('',(-0.000901444335805244,-0.0129354009404534,0.00636957876532512));
#23088=CARTESIAN_POINT('',(-0.00175130445603382,-0.0129914684115673,0.00619007869518455));
#23089=CARTESIAN_POINT('',(-0.00331376164802281,-0.0130965348226607,0.00551390143015753));
#23090=CARTESIAN_POINT('',(-0.00402635871978323,-0.0131455337626401,0.00501722423527107));
#23091=CARTESIAN_POINT('',(-0.00520148400851484,-0.0132364631114643,0.00378533016641609));
#23092=CARTESIAN_POINT('',(-0.00566401222548603,-0.0132783935203091,0.00305011329244757));
#23093=CARTESIAN_POINT('',(-0.00626576144517416,-0.0133551858068643,0.00145749644883311));
#23094=CARTESIAN_POINT('',(-0.00640498244789111,-0.0133900476845746,0.000600096479187167));
#23095=CARTESIAN_POINT('',(-0.00633813792439929,-0.0134527029088608,-0.00110102420868829));
#23096=CARTESIAN_POINT('',(-0.00613207239819051,-0.0134804962554366,-0.0019447449269178));
#23097=CARTESIAN_POINT('',(-0.00576956157983471,-0.0135047553364452,-0.00271508204843087));
#23098=CARTESIAN_POINT('',(-0.00600291424347732,-0.00978191608530591,-0.00195066711549076));
#23099=CARTESIAN_POINT('',(-0.00574246615396974,-0.00991927166446956,-0.00275216088845478));
#23100=CARTESIAN_POINT('',(-0.00531940625127603,-0.0100530929780658,-0.00350058968249359));
#23101=CARTESIAN_POINT('',(-0.0042148744339131,-0.0103136670741236,-0.00477333431135776));
#23102=CARTESIAN_POINT('',(-0.00353340251924386,-0.010440419856585,-0.00529765014618313));
#23103=CARTESIAN_POINT('',(-0.00201997295760755,-0.0106868568903732,-0.00603903134590728));
#23104=CARTESIAN_POINT('',(-0.00118801531064046,-0.0108065411416999,-0.00625609671080607));
#23105=CARTESIAN_POINT('',(0.00049469142812545,-0.0110388411132185,-0.00634864955534044));
#23106=CARTESIAN_POINT('',(0.00134544051992427,-0.0111514568334104,-0.00622413703497603));
#23107=CARTESIAN_POINT('',(0.00293104623631838,-0.0113696197426594,-0.00565323588430546));
#23108=CARTESIAN_POINT('',(0.00366590286091366,-0.0114751669317165,-0.00520684725399929));
#23109=CARTESIAN_POINT('',(0.0049033904503217,-0.011679192778696,-0.00406286356058477));
#23110=CARTESIAN_POINT('',(0.00540602141513444,-0.0117776714366183,-0.00336526849747642));
#23111=CARTESIAN_POINT('',(0.00609948672115684,-0.0119675602213283,-0.00182930645777592));
#23112=CARTESIAN_POINT('',(0.0062903210623665,-0.0120589703481159,-0.000990939481183775));
#23113=CARTESIAN_POINT('',(0.00632998248671984,-0.0122347220705563,0.00069384560895015));
#23114=CARTESIAN_POINT('',(0.00617880956986351,-0.0123190636662091,0.00154026372249193));
#23115=CARTESIAN_POINT('',(0.00555838842139843,-0.01248067832638,0.00310715596523984));
#23116=CARTESIAN_POINT('',(0.00508914018978966,-0.0125579513908981,0.00382763009444596));
#23117=CARTESIAN_POINT('',(0.00390685436447047,-0.0127054289887995,0.0050285772438971));
#23118=CARTESIAN_POINT('',(0.00319381677076005,-0.0127756335221828,0.00550905026414211));
#23119=CARTESIAN_POINT('',(0.00163683219478224,-0.0129089740578147,0.00615393207365234));
#23120=CARTESIAN_POINT('',(0.000792885212514846,-0.0129721100600633,0.00631834086291755));
#23121=CARTESIAN_POINT('',(-0.000892314492040779,-0.0130913135334257,0.00630506756184527));
#23122=CARTESIAN_POINT('',(-0.00173356721432901,-0.0131473810045395,0.00612738547150779));
#23123=CARTESIAN_POINT('',(-0.00328019981295719,-0.0132524474156325,0.00545805654147115));
#23124=CARTESIAN_POINT('',(-0.00398557968929714,-0.0133014463556116,0.004966409701772));
#23125=CARTESIAN_POINT('',(-0.00514880328885766,-0.0133923757044352,0.0037469922772713));
#23126=CARTESIAN_POINT('',(-0.00560664701207822,-0.0134343061132796,0.00301922169246975));
#23127=CARTESIAN_POINT('',(-0.00620230170530152,-0.0135110983998336,0.0014427348996874));
#23128=CARTESIAN_POINT('',(-0.00634011267530426,-0.0135459602775433,0.000594018691706598));
#23129=CARTESIAN_POINT('',(-0.00627394515429806,-0.013608615501828,-0.0010898730165326));
#23130=CARTESIAN_POINT('',(-0.00606996666328912,-0.013636408848403,-0.00192504851679101));
#23131=CARTESIAN_POINT('',(-0.00571112736074751,-0.0136606679294106,-0.00268758365066487));
#23132=CARTESIAN_POINT('',(-0.00600291424347732,-0.0099532476683191,-0.00195066711549076));
#23133=CARTESIAN_POINT('',(-0.00574246615396974,-0.0100906032474828,-0.00275216088845478));
#23134=CARTESIAN_POINT('',(-0.00531940625127604,-0.010224424561079,-0.0035005896824936));
#23135=CARTESIAN_POINT('',(-0.0042148744339131,-0.0104849986571369,-0.00477333431135777));
#23136=CARTESIAN_POINT('',(-0.00353340251924388,-0.0106117514395984,-0.00529765014618313));
#23137=CARTESIAN_POINT('',(-0.00201997295760755,-0.0108581884733867,-0.00603903134590727));
#23138=CARTESIAN_POINT('',(-0.00118801531064046,-0.0109778727247135,-0.00625609671080606));
#23139=CARTESIAN_POINT('',(0.000494691428125452,-0.0112101726962322,-0.00634864955534044));
#23140=CARTESIAN_POINT('',(0.00134544051992427,-0.0113227884164243,-0.00622413703497603));
#23141=CARTESIAN_POINT('',(0.00293104623631838,-0.0115409513256735,-0.00565323588430545));
#23142=CARTESIAN_POINT('',(0.00366590286091367,-0.0116464985147308,-0.00520684725399928));
#23143=CARTESIAN_POINT('',(0.0049033904503217,-0.0118505243617105,-0.00406286356058477));
#23144=CARTESIAN_POINT('',(0.00540602141513444,-0.011949003019633,-0.00336526849747643));
#23145=CARTESIAN_POINT('',(0.00609948672115684,-0.0121388918043431,-0.00182930645777592));
#23146=CARTESIAN_POINT('',(0.0062903210623665,-0.0122303019311308,-0.000990939481183762));
#23147=CARTESIAN_POINT('',(0.00632998248671984,-0.0124060536535715,0.000693845608950163));
#23148=CARTESIAN_POINT('',(0.00617880956986351,-0.0124903952492244,0.00154026372249193));
#23149=CARTESIAN_POINT('',(0.00555838842139842,-0.0126520099093955,0.00310715596523983));
#23150=CARTESIAN_POINT('',(0.00508914018978966,-0.0127292829739137,0.00382763009444597));
#23151=CARTESIAN_POINT('',(0.00390685436447048,-0.0128767605718152,0.00502857724389711));
#23152=CARTESIAN_POINT('',(0.00319381677076006,-0.0129469651051986,0.00550905026414211));
#23153=CARTESIAN_POINT('',(0.00163683219478224,-0.0130803056408305,0.00615393207365233));
#23154=CARTESIAN_POINT('',(0.000792885212514845,-0.0131434416430791,0.00631834086291754));
#23155=CARTESIAN_POINT('',(-0.000892314492040781,-0.0132626451164415,0.00630506756184527));
#23156=CARTESIAN_POINT('',(-0.00173356721432902,-0.0133187125875553,0.00612738547150779));
#23157=CARTESIAN_POINT('',(-0.00328019981295719,-0.0134237789986481,0.00545805654147115));
#23158=CARTESIAN_POINT('',(-0.00398557968929714,-0.0134727779386271,0.004966409701772));
#23159=CARTESIAN_POINT('',(-0.00514880328885766,-0.0135637072874504,0.0037469922772713));
#23160=CARTESIAN_POINT('',(-0.00560664701207823,-0.0136056376962946,0.00301922169246975));
#23161=CARTESIAN_POINT('',(-0.00620230170530153,-0.0136824299828483,0.0014427348996874));
#23162=CARTESIAN_POINT('',(-0.00634011267530426,-0.0137172918605577,0.000594018691706601));
#23163=CARTESIAN_POINT('',(-0.00627394515429805,-0.0137799470848417,-0.0010898730165326));
#23164=CARTESIAN_POINT('',(-0.00606996666328913,-0.0138077404314164,-0.00192504851679101));
#23165=CARTESIAN_POINT('',(-0.00571112736074751,-0.0138319995124236,-0.00268758365066487));
#23166=CARTESIAN_POINT('',(-0.00600351494261159,-0.00996866665836644,-0.00195086231468902));
#23167=CARTESIAN_POINT('',(-0.00574304079060577,-0.0101060222375301,-0.00275243629146672));
#23168=CARTESIAN_POINT('',(-0.00531993855318813,-0.0102398435511264,-0.00350093997921721));
#23169=CARTESIAN_POINT('',(-0.00421529620762514,-0.0105004176471842,-0.00477381196898739));
#23170=CARTESIAN_POINT('',(-0.00353375609947977,-0.0106271704296457,-0.00529818027100706));
#23171=CARTESIAN_POINT('',(-0.00202017509209718,-0.0108736074634341,-0.0060396356592048));
#23172=CARTESIAN_POINT('',(-0.00118813419285994,-0.0109932917147608,-0.00625672274538287));
#23173=CARTESIAN_POINT('',(0.000494740930867045,-0.0112255916862796,-0.00634928485148777));
#23174=CARTESIAN_POINT('',(0.00134557515535679,-0.0113382074064716,-0.0062247598714146));
#23175=CARTESIAN_POINT('',(0.00293133954001475,-0.0115563703157209,-0.00565380159185411));
#23176=CARTESIAN_POINT('',(0.00366626970018299,-0.0116619175047782,-0.00520736829236679));
#23177=CARTESIAN_POINT('',(0.00490388112239846,-0.0118659433517579,-0.0040632701228851));
#23178=CARTESIAN_POINT('',(0.00540656238444571,-0.0119644220096804,-0.00336560525289072));
#23179=CARTESIAN_POINT('',(0.00610009708409794,-0.0121543107943906,-0.00182948951266575));
#23180=CARTESIAN_POINT('',(0.00629095052170294,-0.0122457209211783,-0.000991038642435164));
#23181=CARTESIAN_POINT('',(0.00633061591489246,-0.012421472643619,0.000693915040636126));
#23182=CARTESIAN_POINT('',(0.00617942787047698,-0.0125058142392719,0.00154041785347683));
#23183=CARTESIAN_POINT('',(0.00555894463775888,-0.012667428899443,0.00310746689187023));
#23184=CARTESIAN_POINT('',(0.00508964944945624,-0.0127447019639612,0.00382801311742293));
#23185=CARTESIAN_POINT('',(0.00390724531525525,-0.0128921795618627,0.00502908044315575));
#23186=CARTESIAN_POINT('',(0.0031941363693569,-0.0129623840952461,0.00550960154333586));
#23187=CARTESIAN_POINT('',(0.00163699598917317,-0.0130957246308781,0.00615454788482654));
#23188=CARTESIAN_POINT('',(0.000792964554887801,-0.0131588606331266,0.0063189731261371));
#23189=CARTESIAN_POINT('',(-0.000892403784094793,-0.013278064106489,0.00630569849683322));
#23190=CARTESIAN_POINT('',(-0.00173374068879202,-0.0133341315776028,0.00612799862621877));
#23191=CARTESIAN_POINT('',(-0.00328052805572528,-0.0134391979886957,0.0054586027178292));
#23192=CARTESIAN_POINT('',(-0.00398597851796132,-0.0134881969286747,0.00496690668005408));
#23193=CARTESIAN_POINT('',(-0.00514931851888639,-0.0135791262774979,0.00374736723098973));
#23194=CARTESIAN_POINT('',(-0.00560720805757541,-0.0136210566863421,0.0030195238197005));
#23195=CARTESIAN_POINT('',(-0.0062029223567241,-0.0136978489728957,0.001442879271166));
#23196=CARTESIAN_POINT('',(-0.00634074711718376,-0.0137327108506051,0.000594078133920727));
#23197=CARTESIAN_POINT('',(-0.00627457297493145,-0.0137953660748891,-0.00108998207785698));
#23198=CARTESIAN_POINT('',(-0.00607057407221948,-0.0138231594214637,-0.00192524115238941));
#23199=CARTESIAN_POINT('',(-0.00571169886137572,-0.0138474185024709,-0.00268785259156703));
#23200=CARTESIAN_POINT('',(-0.0060046989412083,-0.00998404147970407,-0.00195124705900381));
#23201=CARTESIAN_POINT('',(-0.00574417341912455,-0.0101213970588677,-0.00275297912024915));
#23202=CARTESIAN_POINT('',(-0.00532098773851402,-0.010255218372464,-0.00350163042607414));
#23203=CARTESIAN_POINT('',(-0.00421612753807775,-0.0105157924685218,-0.00477475344855832));
#23204=CARTESIAN_POINT('',(-0.00353445301825201,-0.0106425452509834,-0.00529922516521753));
#23205=CARTESIAN_POINT('',(-0.00202057350610914,-0.0108889822847717,-0.00604082678144128));
#23206=CARTESIAN_POINT('',(-0.00118836851379201,-0.0110086665360985,-0.00625795668100581));
#23207=CARTESIAN_POINT('',(0.000494838502468596,-0.0112409665076173,-0.00635053704198386));
#23208=CARTESIAN_POINT('',(0.00134584052641207,-0.0113535822278093,-0.00622598750339738));
#23209=CARTESIAN_POINT('',(0.00293191765166019,-0.0115717451370586,-0.00565491662083544));
#23210=CARTESIAN_POINT('',(0.00366699275296484,-0.0116772923261159,-0.00520839527685999));
#23211=CARTESIAN_POINT('',(0.00490484825389107,-0.0118813181730956,-0.00406407147112351));
#23212=CARTESIAN_POINT('',(0.00540762865351265,-0.0119797968310181,-0.00336626900936249));
#23213=CARTESIAN_POINT('',(0.0061013001303894,-0.0121696856157283,-0.00182985032013211));
#23214=CARTESIAN_POINT('',(0.00629219120764457,-0.0122610957425161,-0.000991234092662764));
#23215=CARTESIAN_POINT('',(0.00633186442354634,-0.0124368474649567,0.00069405189287056));
#23216=CARTESIAN_POINT('',(0.00618064656219293,-0.0125211890606097,0.00154072165093453));
#23217=CARTESIAN_POINT('',(0.00556004095928272,-0.0126828037207808,0.00310807973892308));
#23218=CARTESIAN_POINT('',(0.00509065321772592,-0.0127600767852989,0.00382876806884765));
#23219=CARTESIAN_POINT('',(0.00390801589266107,-0.0129075543832005,0.00503007226615351));
#23220=CARTESIAN_POINT('',(0.00319476630915303,-0.0129777589165839,0.00551068813353479));
#23221=CARTESIAN_POINT('',(0.0016373188335356,-0.0131110994522158,0.00615576166977231));
#23222=CARTESIAN_POINT('',(0.000793120941426221,-0.0131742354544644,0.00632021933862854));
#23223=CARTESIAN_POINT('',(-0.000892579781795835,-0.0132934389278268,0.0063069420913346));
#23224=CARTESIAN_POINT('',(-0.00173408261290851,-0.0133495063989406,0.00612920717518442));
#23225=CARTESIAN_POINT('',(-0.00328117503347941,-0.0134545728100334,0.00545967925016396));
#23226=CARTESIAN_POINT('',(-0.00398676462293764,-0.0135035717500124,0.00496788624129369));
#23227=CARTESIAN_POINT('',(-0.00515033405494463,-0.0135945010988356,0.00374810627762912));
#23228=CARTESIAN_POINT('',(-0.00560831389749338,-0.0136364315076798,0.00302011932283482));
#23229=CARTESIAN_POINT('',(-0.00620414568196542,-0.0137132237942334,0.00144316383230204));
#23230=CARTESIAN_POINT('',(-0.00634199762388869,-0.0137480856719428,0.00059419529656355));
#23231=CARTESIAN_POINT('',(-0.0062758104309332,-0.0138107408962268,-0.00109019704146795));
#23232=CARTESIAN_POINT('',(-0.00607177129605443,-0.0138385342428014,-0.00192562084376098));
#23233=CARTESIAN_POINT('',(-0.00571282530871555,-0.0138627933238085,-0.00268838268330946));
#23234=CARTESIAN_POINT('',(-0.00697848962230257,-0.0100021880761874,-0.00276298368595472));
#23235=CARTESIAN_POINT('',(-0.0069784927334439,-0.00984627346412808,-0.00276298497368024));
#23236=CARTESIAN_POINT('',(-0.00685840540887306,-0.00953444168472413,-0.0027154390780474));
#23237=CARTESIAN_POINT('',(-0.00642351660340855,-0.00934069305043517,-0.00254325430359987));
#23238=CARTESIAN_POINT('',(-0.00598862778407599,-0.00953444167233752,-0.0023710695004056));
#23239=CARTESIAN_POINT('',(-0.0058685404369188,-0.0098462734648897,-0.00232352356685033));
#23240=CARTESIAN_POINT('',(-0.00586854353315033,-0.0100021880910911,-0.00232352483977624));
#23241=CARTESIAN_POINT('',(-0.00595196988716087,0.0137864962072417,0.00210067694133285));
#23242=CARTESIAN_POINT('',(-0.00572722627692746,0.0138067909284317,0.00273633130246211));
#23243=CARTESIAN_POINT('',(-0.00540062531389276,0.0138270856496218,0.00333605153597525));
#23244=CARTESIAN_POINT('',(-0.00446089318476394,0.0138732460374782,0.00454750491924395));
#23245=CARTESIAN_POINT('',(-0.00379371870698236,0.0138991117041446,0.00511734584923682));
#23246=CARTESIAN_POINT('',(-0.00228794870083571,0.0139508430374775,0.00594516609786777));
#23247=CARTESIAN_POINT('',(-0.00144935317247064,0.013976708704144,0.00620314541650586));
#23248=CARTESIAN_POINT('',(0.000261328061997682,0.0140284400374772,0.00636484747719175));
#23249=CARTESIAN_POINT('',(0.00113341376810093,0.0140543057041439,0.00626857021923956));
#23250=CARTESIAN_POINT('',(0.00276762255858251,0.0141060370374773,0.00573758506115909));
#23251=CARTESIAN_POINT('',(0.00352974564296082,0.0141319027041441,0.00530287716103082));
#23252=CARTESIAN_POINT('',(0.00481866773505796,0.0141836340374777,0.00416653903580334));
#23253=CARTESIAN_POINT('',(0.00534546674277679,0.0142094997041445,0.00346490881070412));
#23254=CARTESIAN_POINT('',(0.00607708692013597,0.0142612310374782,0.00191013694324312));
#23255=CARTESIAN_POINT('',(0.00628190808977635,0.0142870967041451,0.00105699530088134));
#23256=CARTESIAN_POINT('',(0.00633588145473074,0.0143388280374788,-0.000660465289815461));
#23257=CARTESIAN_POINT('',(0.00618503365004477,0.0143646937041458,-0.00152478423815047));
#23258=CARTESIAN_POINT('',(0.00555248212780469,0.0144164250374796,-0.00312242701203853));
#23259=CARTESIAN_POINT('',(0.00507077841025057,0.0144422907041465,-0.00385575083759157));
#23260=CARTESIAN_POINT('',(0.00385575084356898,0.0144940220374802,-0.00507077841625911));
#23261=CARTESIAN_POINT('',(0.00312242699444151,0.0145198877041471,-0.00555248216937361));
#23262=CARTESIAN_POINT('',(0.00152478425570669,0.0145716190374808,-0.00618503360849201));
#23263=CARTESIAN_POINT('',(0.000660465366099334,0.0145974847041477,-0.00633588129449591));
#23264=CARTESIAN_POINT('',(-0.00105699537720861,0.0146492160374812,-0.0062819082500098));
#23265=CARTESIAN_POINT('',(-0.0019101372309092,0.014675081704148,-0.00607708751951978));
#23266=CARTESIAN_POINT('',(-0.00346490852307661,0.0147268130374814,-0.00534546614337484));
#23267=CARTESIAN_POINT('',(-0.00416653796154343,0.0147526787041481,-0.00481866549771993));
#23268=CARTESIAN_POINT('',(-0.00530287823531816,0.0148044100374813,-0.00352974788026773));
#23269=CARTESIAN_POINT('',(-0.00573758907062607,0.0148302757041478,-0.00276763090847045));
#23270=CARTESIAN_POINT('',(-0.00626856620978494,0.0148820070374808,-0.00113340541817491));
#23271=CARTESIAN_POINT('',(-0.00636483251363591,0.0149078727041471,-0.000261296899676647));
#23272=CARTESIAN_POINT('',(-0.0062205710326375,0.0149540330324328,0.00126510354979954));
#23273=CARTESIAN_POINT('',(-0.00604811696439261,0.014974327694052,0.00192585262016124));
#23274=CARTESIAN_POINT('',(-0.00577681402884133,0.0149946223556712,0.00254307073910409));
#23275=CARTESIAN_POINT('',(-0.00595190119996603,0.013790242654245,0.00210065269900483));
#23276=CARTESIAN_POINT('',(-0.0057271601833291,0.013810537375435,0.00273629972452659));
#23277=CARTESIAN_POINT('',(-0.00540056298934976,0.0138308320966251,0.00333601303712089));
#23278=CARTESIAN_POINT('',(-0.00446084170496059,0.0138769924844815,0.00454745243991991));
#23279=CARTESIAN_POINT('',(-0.0037936749265364,0.0139028581511479,0.00511728679380844));
#23280=CARTESIAN_POINT('',(-0.00228792229734557,0.0139545894844808,0.00594509748919034));
#23281=CARTESIAN_POINT('',(-0.00144933644657894,0.0139804551511473,0.00620307383068371));
#23282=CARTESIAN_POINT('',(0.000261325046207641,0.0140321864844806,0.00636477402528809));
#23283=CARTESIAN_POINT('',(0.00113340068822758,0.0140580521511472,0.00626849787839911));
#23284=CARTESIAN_POINT('',(0.0027675906195382,0.0141097834844806,0.00573751884801782));
#23285=CARTESIAN_POINT('',(0.00352970490882888,0.0141356491511474,0.00530281596452552));
#23286=CARTESIAN_POINT('',(0.0048186121264484,0.014187380484481,0.00416649095291919));
#23287=CARTESIAN_POINT('',(0.00534540505477725,0.0142132461511478,0.00346486882480515));
#23288=CARTESIAN_POINT('',(0.00607701678905984,0.0142649774844815,0.00191011489979349));
#23289=CARTESIAN_POINT('',(0.00628183559501359,0.0142908431511484,0.00105698310289587));
#23290=CARTESIAN_POINT('',(0.00633580833710209,0.0143425744844822,-0.000660457667883747));
#23291=CARTESIAN_POINT('',(0.00618496227323685,0.0143684401511491,-0.00152476664176574));
#23292=CARTESIAN_POINT('',(0.00555241805079674,0.0144201714844829,-0.00312239097846366));
#23293=CARTESIAN_POINT('',(0.00507071989222187,0.0144460371511498,-0.00385570634127959));
#23294=CARTESIAN_POINT('',(0.00385570634725693,0.0144977684844836,-0.00507071989823035));
#23295=CARTESIAN_POINT('',(0.00312239096086684,0.0145236341511504,-0.00555241809236518));
#23296=CARTESIAN_POINT('',(0.00152476665932175,0.0145753654844841,-0.00618496223168457));
#23297=CARTESIAN_POINT('',(0.00066045774416674,0.014601231151151,-0.00633580817686911));
#23298=CARTESIAN_POINT('',(-0.00105698317922226,0.0146529624844846,-0.0062818357552452));
#23299=CARTESIAN_POINT('',(-0.00191011518745625,0.0146788281511513,-0.00607701738843673));
#23300=CARTESIAN_POINT('',(-0.00346486853718096,0.0147305594844847,-0.00534540445538222));
#23301=CARTESIAN_POINT('',(-0.00416648987867168,0.0147564251511514,-0.00481860988913619));
#23302=CARTESIAN_POINT('',(-0.00530281703880047,0.0148081564844846,-0.00352970714610997));
#23303=CARTESIAN_POINT('',(-0.00573752285743853,0.0148340221511511,-0.00276759896932979));
#23304=CARTESIAN_POINT('',(-0.00626849386899076,0.0148857534844841,-0.00113339233839792));
#23305=CARTESIAN_POINT('',(-0.00636475906190493,0.0149116191511505,-0.000261293884246227));
#23306=CARTESIAN_POINT('',(-0.00622049924571945,0.0149577794794361,0.00126508895019375));
#23307=CARTESIAN_POINT('',(-0.00604804716763688,0.0149780741410553,0.00192583039534884));
#23308=CARTESIAN_POINT('',(-0.00577674736298813,0.0149983688026745,0.00254304139144295));
#23309=CARTESIAN_POINT('',(-0.00595186675769869,0.0137939897453371,0.00210064054301644));
#23310=CARTESIAN_POINT('',(-0.00572712704158573,0.0138142844665271,0.00273628389019677));
#23311=CARTESIAN_POINT('',(-0.00540053173754835,0.0138345791877171,0.00333599373238967));
#23312=CARTESIAN_POINT('',(-0.0044608158911076,0.0138807395755735,0.00454742612487075));
#23313=CARTESIAN_POINT('',(-0.00379365297342232,0.0139066052422399,0.00511725718126046));
#23314=CARTESIAN_POINT('',(-0.0022879090576716,0.0139583365755728,0.00594506308629448));
#23315=CARTESIAN_POINT('',(-0.00144932805960615,0.0139842022422394,0.00620303793493879));
#23316=CARTESIAN_POINT('',(0.000261323533980404,0.0140359335755726,0.00636473719382177));
#23317=CARTESIAN_POINT('',(0.00113339412950152,0.0140617992422392,0.00626846160406045));
#23318=CARTESIAN_POINT('',(0.00276757460413526,0.0141135305755727,0.00573748564633126));
#23319=CARTESIAN_POINT('',(0.00352968448324787,0.0141393962422394,0.0053027852783634));
#23320=CARTESIAN_POINT('',(0.00481858424226123,0.014191127575573,0.00416646684240551));
#23321=CARTESIAN_POINT('',(0.00534537412216198,0.0142169932422398,0.00346484877441548));
#23322=CARTESIAN_POINT('',(0.00607698162277769,0.0142687245755735,0.00191010384640302));
#23323=CARTESIAN_POINT('',(0.00628179924349267,0.0142945902422404,0.00105697698638059));
#23324=CARTESIAN_POINT('',(0.00633577167325347,0.0143463215755742,-0.000660453845968899));
#23325=CARTESIAN_POINT('',(0.0061849264822993,0.0143721872422411,-0.00152475781829597));
#23326=CARTESIAN_POINT('',(0.00555238592024543,0.0144239185755749,-0.00312237290991359));
#23327=CARTESIAN_POINT('',(0.00507069054914572,0.0144497842422418,-0.00385568402920415));
#23328=CARTESIAN_POINT('',(0.00385568403518144,0.0145015155755756,-0.00507069055515416));
#23329=CARTESIAN_POINT('',(0.00312237289231688,0.0145273812422425,-0.00555238596181363));
#23330=CARTESIAN_POINT('',(0.00152475783585188,0.0145791125755762,-0.00618492644074726));
#23331=CARTESIAN_POINT('',(0.000660453922251451,0.014604978242243,-0.00633577151302142));
#23332=CARTESIAN_POINT('',(-0.00105697706270654,0.0146567095755766,-0.00628179940372335));
#23333=CARTESIAN_POINT('',(-0.00191010413406411,0.0146825752422434,-0.00607698222215111));
#23334=CARTESIAN_POINT('',(-0.00346484848679295,0.0147343065755768,-0.00534537352277041));
#23335=CARTESIAN_POINT('',(-0.00416646576816422,0.0147601722422434,-0.00481858200496196));
#23336=CARTESIAN_POINT('',(-0.00530278635263213,0.0148119035755766,-0.00352968672051601));
#23337=CARTESIAN_POINT('',(-0.00573748965572877,0.0148377692422432,-0.00276758295387852));
#23338=CARTESIAN_POINT('',(-0.0062684575946753,0.0148895005755761,-0.00113338577972018));
#23339=CARTESIAN_POINT('',(-0.0063647222305252,0.0149153662422425,-0.000261292372199317));
#23340=CARTESIAN_POINT('',(-0.00622046324913771,0.0149615265705281,0.00126508162941836));
#23341=CARTESIAN_POINT('',(-0.00604801216899519,0.0149818212321474,0.00192581925101645));
#23342=CARTESIAN_POINT('',(-0.00577671393429529,0.0150021158937665,0.00254302667545414));
#23343=CARTESIAN_POINT('',(-0.00595186675769868,0.0139226378312596,0.00210064054301645));
#23344=CARTESIAN_POINT('',(-0.00572712704158573,0.0139429325524496,0.00273628389019677));
#23345=CARTESIAN_POINT('',(-0.00540053173754835,0.0139632272736397,0.00333599373238967));
#23346=CARTESIAN_POINT('',(-0.00446081589110761,0.0140093876614961,0.00454742612487074));
#23347=CARTESIAN_POINT('',(-0.00379365297342231,0.0140352533281625,0.00511725718126046));
#23348=CARTESIAN_POINT('',(-0.0022879090576716,0.0140869846614954,0.00594506308629448));
#23349=CARTESIAN_POINT('',(-0.00144932805960616,0.0141128503281619,0.00620303793493879));
#23350=CARTESIAN_POINT('',(0.000261323533980407,0.0141645816614952,0.00636473719382179));
#23351=CARTESIAN_POINT('',(0.00113339412950153,0.0141904473281618,0.00626846160406046));
#23352=CARTESIAN_POINT('',(0.00276757460413526,0.0142421786614953,0.00573748564633127));
#23353=CARTESIAN_POINT('',(0.00352968448324788,0.014268044328162,0.00530278527836341));
#23354=CARTESIAN_POINT('',(0.00481858424226124,0.0143197756614956,0.00416646684240551));
#23355=CARTESIAN_POINT('',(0.00534537412216198,0.0143456413281624,0.00346484877441548));
#23356=CARTESIAN_POINT('',(0.00607698162277769,0.0143973726614961,0.00191010384640303));
#23357=CARTESIAN_POINT('',(0.00628179924349266,0.014423238328163,0.0010569769863806));
#23358=CARTESIAN_POINT('',(0.00633577167325347,0.0144749696614968,-0.000660453845968898));
#23359=CARTESIAN_POINT('',(0.00618492648229931,0.0145008353281637,-0.00152475781829598));
#23360=CARTESIAN_POINT('',(0.00555238592024543,0.0145525666614975,-0.00312237290991359));
#23361=CARTESIAN_POINT('',(0.00507069054914572,0.0145784323281644,-0.00385568402920415));
#23362=CARTESIAN_POINT('',(0.00385568403518144,0.0146301636614982,-0.00507069055515416));
#23363=CARTESIAN_POINT('',(0.00312237289231687,0.014656029328165,-0.00555238596181364));
#23364=CARTESIAN_POINT('',(0.00152475783585188,0.0147077606614987,-0.00618492644074726));
#23365=CARTESIAN_POINT('',(0.000660453922251451,0.0147336263281656,-0.00633577151302143));
#23366=CARTESIAN_POINT('',(-0.00105697706270654,0.0147853576614992,-0.00628179940372336));
#23367=CARTESIAN_POINT('',(-0.00191010413406411,0.0148112233281659,-0.00607698222215111));
#23368=CARTESIAN_POINT('',(-0.00346484848679296,0.0148629546614993,-0.00534537352277042));
#23369=CARTESIAN_POINT('',(-0.00416646576816423,0.014888820328166,-0.00481858200496196));
#23370=CARTESIAN_POINT('',(-0.00530278635263215,0.0149405516614992,-0.003529686720516));
#23371=CARTESIAN_POINT('',(-0.00573748965572878,0.0149664173281658,-0.00276758295387851));
#23372=CARTESIAN_POINT('',(-0.00626845759467531,0.0150181486614987,-0.00113338577972016));
#23373=CARTESIAN_POINT('',(-0.0063647222305252,0.0150440143281651,-0.000261292372199312));
#23374=CARTESIAN_POINT('',(-0.00622046324913772,0.0150901746564507,0.00126508162941836));
#23375=CARTESIAN_POINT('',(-0.0060480121689952,0.0151104693180699,0.00192581925101644));
#23376=CARTESIAN_POINT('',(-0.00577671393429529,0.0151307639796891,0.00254302667545414));
#23377=CARTESIAN_POINT('',(-0.00599013469261116,0.0140475388260902,0.00211414675524317));
#23378=CARTESIAN_POINT('',(-0.0057639499971029,0.0140678335472802,0.00275387701485411));
#23379=CARTESIAN_POINT('',(-0.00543525482619242,0.0140881282684702,0.00335744273254653));
#23380=CARTESIAN_POINT('',(-0.00448949701236366,0.0141342886563267,0.004576664112556));
#23381=CARTESIAN_POINT('',(-0.00381804452501068,0.014160154322993,0.00515015893674575));
#23382=CARTESIAN_POINT('',(-0.00230261932563776,0.014211885656326,0.00598328727653573));
#23383=CARTESIAN_POINT('',(-0.00145864661361782,0.0142377513229925,0.00624292079213596));
#23384=CARTESIAN_POINT('',(0.000263003731538004,0.0142894826563257,0.00640565970747737));
#23385=CARTESIAN_POINT('',(0.00114068136467389,0.0143153483229924,0.00630876510721855));
#23386=CARTESIAN_POINT('',(0.00278536891458071,0.0143670796563258,0.00577437520320702));
#23387=CARTESIAN_POINT('',(0.00355237883135164,0.0143929453229926,0.0053368798994543));
#23388=CARTESIAN_POINT('',(0.00484956565963161,0.0144446766563261,0.00419325542629542));
#23389=CARTESIAN_POINT('',(0.00537974257114063,0.014470542322993,0.00348712625688925));
#23390=CARTESIAN_POINT('',(0.00611605399228327,0.0145222736563267,0.0019223849898906));
#23391=CARTESIAN_POINT('',(0.00632218850191688,0.0145481393229936,0.0010637728922981));
#23392=CARTESIAN_POINT('',(0.00637650795111096,0.0145998706563273,-0.000664700279200542));
#23393=CARTESIAN_POINT('',(0.00622469289067142,0.0146257363229942,-0.00153456135310668));
#23394=CARTESIAN_POINT('',(0.00558808536575638,0.014677467656328,-0.00314244842036324));
#23395=CARTESIAN_POINT('',(0.00510329290128087,0.014703333322995,-0.00388047441371365));
#23396=CARTESIAN_POINT('',(0.00388047441972938,0.0147550646563287,-0.00510329290732795));
#23397=CARTESIAN_POINT('',(0.00314244840265338,0.0147809303229956,-0.00558808540759184));
#23398=CARTESIAN_POINT('',(0.00153456137077547,0.0148326616563293,-0.00622469284885221));
#23399=CARTESIAN_POINT('',(0.000664700355973563,0.0148585273229961,-0.00637650778984869));
#23400=CARTESIAN_POINT('',(-0.00106377296911478,0.0149102586563297,-0.00632218866317778));
#23401=CARTESIAN_POINT('',(-0.00192238527940122,0.0149361243229965,-0.0061160545955104));
#23402=CARTESIAN_POINT('',(-0.00348712596741744,0.0149878556563299,-0.00537974196789524));
#23403=CARTESIAN_POINT('',(-0.00419325434514722,0.0150137213229966,-0.00484956340794746));
#23404=CARTESIAN_POINT('',(-0.00533688098063012,0.0150654526563297,-0.00355238108300445));
#23405=CARTESIAN_POINT('',(-0.00577437923838323,0.0150913183229963,-0.00278537731800922));
#23406=CARTESIAN_POINT('',(-0.0063087610720548,0.0151430496563293,-0.00114067296120705));
#23407=CARTESIAN_POINT('',(-0.00640564464797325,0.0151689153229957,-0.000262972369400112));
#23408=CARTESIAN_POINT('',(-0.00626045814358583,0.0152150756512812,0.00127321555838962));
#23409=CARTESIAN_POINT('',(-0.0060868982774138,0.0152353703129005,0.0019382014377742));
#23410=CARTESIAN_POINT('',(-0.00581385571213493,0.0152556649745197,0.00255937723961472));
#23411=CARTESIAN_POINT('',(-0.00612858938180376,0.0142496328809547,0.00216301269013872));
#23412=CARTESIAN_POINT('',(-0.00589717670173025,0.0142699276021447,0.0028175295378327));
#23413=CARTESIAN_POINT('',(-0.00556088414110103,0.0142902223233348,0.00343504594413876));
#23414=CARTESIAN_POINT('',(-0.00459326628390352,0.0143363827111912,0.00468244814576388));
#23415=CARTESIAN_POINT('',(-0.0039062939876957,0.0143622483778576,0.0052691986063811));
#23416=CARTESIAN_POINT('',(-0.00235584157512295,0.0144139797111905,0.00612158369602103));
#23417=CARTESIAN_POINT('',(-0.00149236145875801,0.014439845377857,0.00638721832504375));
#23418=CARTESIAN_POINT('',(0.000269082743409222,0.0144915767111902,0.00655371875278837));
#23419=CARTESIAN_POINT('',(0.00116704682921152,0.0145174423778569,0.00645458455151026));
#23420=CARTESIAN_POINT('',(0.00284974933457872,0.0145691737111903,0.00590784287381343));
#23421=CARTESIAN_POINT('',(0.00363448775414362,0.0145950393778571,0.00546023539739471));
#23422=CARTESIAN_POINT('',(0.00496165748069727,0.0146467707111907,0.00429017743331958));
#23423=CARTESIAN_POINT('',(0.00550408878768602,0.0146726363778575,0.00356772694566317));
#23424=CARTESIAN_POINT('',(0.00625741915317544,0.0147243677111912,0.00196681858444935));
#23425=CARTESIAN_POINT('',(0.00646831821167611,0.0147502333778581,0.00108836071089195));
#23426=CARTESIAN_POINT('',(0.00652389318897451,0.0148019647111919,-0.000680064018963598));
#23427=CARTESIAN_POINT('',(0.00636856910777225,0.0148278303778588,-0.00157003087526174));
#23428=CARTESIAN_POINT('',(0.00571724717299452,0.0148795617111926,-0.00321508229951153));
#23429=CARTESIAN_POINT('',(0.00522124931941905,0.0149054273778595,-0.00397016686746319));
#23430=CARTESIAN_POINT('',(0.00397016687361797,0.0149571587111933,-0.0052212493256059));
#23431=CARTESIAN_POINT('',(0.00321508228139234,0.0149830243778601,-0.00571724721579696));
#23432=CARTESIAN_POINT('',(0.00157003089333893,0.0150347557111939,-0.00636856906498643));
#23433=CARTESIAN_POINT('',(0.000680064097511137,0.0150606213778607,-0.00652389302398486));
#23434=CARTESIAN_POINT('',(-0.00108836078948416,0.0151123527111943,-0.00646831837666436));
#23435=CARTESIAN_POINT('',(-0.00196681888065166,0.015138218377861,-0.00625741977034543));
#23436=CARTESIAN_POINT('',(-0.00356772664950055,0.0151899497111945,-0.00550408817049734));
#23437=CARTESIAN_POINT('',(-0.00429017632718195,0.0152158153778611,-0.00496165517696819));
#23438=CARTESIAN_POINT('',(-0.00546023650356059,0.0152675467111943,-0.00363449005784066));
#23439=CARTESIAN_POINT('',(-0.00590784700225784,0.0152934123778609,-0.00284975793224229));
#23440=CARTESIAN_POINT('',(-0.00645458042307859,0.0153451437111938,-0.00116703823150876));
#23441=CARTESIAN_POINT('',(-0.0065537033452021,0.0153710093778602,-0.000269050656373603));
#23442=CARTESIAN_POINT('',(-0.00640516103107559,0.0154171697061458,0.00130264438986973));
#23443=CARTESIAN_POINT('',(-0.00622758953936252,0.015437464367765,0.0019830006103188));
#23444=CARTESIAN_POINT('',(-0.00594823592676135,0.0154577590293842,0.00261853413648293));
#23445=CARTESIAN_POINT('',(-0.00622877613608389,0.0143268259409887,0.00219837241280755));
#23446=CARTESIAN_POINT('',(-0.00599358045084044,0.0143471206621787,0.00286358893615395));
#23447=CARTESIAN_POINT('',(-0.00565179036736558,0.0143674153833687,0.00349120015557414));
#23448=CARTESIAN_POINT('',(-0.00466835443418733,0.0144135757712251,0.00475899419128652));
#23449=CARTESIAN_POINT('',(-0.00397015189879237,0.0144394414378915,0.00535533652053114));
#23450=CARTESIAN_POINT('',(-0.00239435355664198,0.0144911727712245,0.00622165592526508));
#23451=CARTESIAN_POINT('',(-0.00151675774988655,0.014517038437891,0.00649163300075439));
#23452=CARTESIAN_POINT('',(0.000273481557722839,0.0145687697712242,0.00666085528444379));
#23453=CARTESIAN_POINT('',(0.00118612505857679,0.0145946354378909,0.00656010049264387));
#23454=CARTESIAN_POINT('',(0.00289633544413129,0.0146463667712243,0.00600442098754409));
#23455=CARTESIAN_POINT('',(0.00369390232883182,0.014672232437891,0.00554949627424423));
#23456=CARTESIAN_POINT('',(0.00504276788439256,0.0147239637712246,0.00436031085645383));
#23457=CARTESIAN_POINT('',(0.00559406655525276,0.0147498294378914,0.0036260501519633));
#23458=CARTESIAN_POINT('',(0.00635971194456203,0.0148015607712252,0.00199897103552053));
#23459=CARTESIAN_POINT('',(0.00657405866301112,0.014827426437892,0.0011061526235683));
#23460=CARTESIAN_POINT('',(0.00663054214898058,0.0148791577712258,-0.000691181325495012));
#23461=CARTESIAN_POINT('',(0.00647267891650096,0.0149050234378927,-0.00159569686260609));
#23462=CARTESIAN_POINT('',(0.0058107095347217,0.0149567547712265,-0.0032676406682102));
#23463=CARTESIAN_POINT('',(0.00530660338542208,0.0149826204378934,-0.00403506893670324));
#23464=CARTESIAN_POINT('',(0.00403506894295862,0.0150343517712272,-0.00530660339171006));
#23465=CARTESIAN_POINT('',(0.0032676406497948,0.0150602174378941,-0.00581070957822385));
#23466=CARTESIAN_POINT('',(0.00159569688097878,0.0151119487712278,-0.00647267887301571));
#23467=CARTESIAN_POINT('',(0.000691181405326598,0.0151378144378947,-0.00663054198129377));
#23468=CARTESIAN_POINT('',(-0.00110615270344529,0.0151895457712282,-0.0065740588306965));
#23469=CARTESIAN_POINT('',(-0.001998971336565,0.015215411437895,-0.00635971257182118));
#23470=CARTESIAN_POINT('',(-0.00362604985095919,0.0152671427712284,-0.00559406592797463));
#23471=CARTESIAN_POINT('',(-0.00436030973223368,0.015293008437895,-0.0050427655430034));
#23472=CARTESIAN_POINT('',(-0.00554949739849309,0.0153447397712283,-0.00369390467018841));
#23473=CARTESIAN_POINT('',(-0.006004425183478,0.0153706054378948,-0.00289634418234465));
#23474=CARTESIAN_POINT('',(-0.00656009629672291,0.0154223367712278,-0.00118611632032359));
#23475=CARTESIAN_POINT('',(-0.00666083962498291,0.0154482024378941,-0.000273448946146293));
#23476=CARTESIAN_POINT('',(-0.00650986902411724,0.0154943627661797,0.00132393929237858));
#23477=CARTESIAN_POINT('',(-0.00632939469289264,0.015514657427799,0.00201541759610565));
#23478=CARTESIAN_POINT('',(-0.00604547436354813,0.0155349520894182,0.00266134046919056));
#23479=CARTESIAN_POINT('',(-0.00645280052909932,0.0144040190010226,0.0022774391563606));
#23480=CARTESIAN_POINT('',(-0.00620914578713664,0.0144243137222126,0.00296658088180299));
#23481=CARTESIAN_POINT('',(-0.00585506286887108,0.0144446084434027,0.00361676478956652));
#23482=CARTESIAN_POINT('',(-0.00483625664252665,0.0144907688312591,0.00493015635248392));
#23483=CARTESIAN_POINT('',(-0.00411294252890566,0.0145166344979255,0.00554794675201068));
#23484=CARTESIAN_POINT('',(-0.00248046896526675,0.0145683658312584,0.00644542423251471));
#23485=CARTESIAN_POINT('',(-0.00157130951524883,0.014594231497925,0.00672511131349197));
#23486=CARTESIAN_POINT('',(0.000283317605548484,0.0146459628312582,0.00690041985209886));
#23487=CARTESIAN_POINT('',(0.00122878527632787,0.0146718284979248,0.00679604130972849));
#23488=CARTESIAN_POINT('',(0.00300050515189807,0.0147235598312582,0.00622037621498455));
#23489=CARTESIAN_POINT('',(0.00382675735668889,0.014749425497925,0.00574908966261098));
#23490=CARTESIAN_POINT('',(0.00522413626073768,0.0148011568312586,0.00451713395807678));
#23491=CARTESIAN_POINT('',(0.00579526295999565,0.0148270224979254,0.00375646480591615));
#23492=CARTESIAN_POINT('',(0.00658844557971067,0.0148787538312591,0.00207086610175894));
#23493=CARTESIAN_POINT('',(0.0068105015001677,0.014904619497926,0.00114593654976237));
#23494=CARTESIAN_POINT('',(0.0068690164732838,0.0149563508312598,-0.000716040378625947));
#23495=CARTESIAN_POINT('',(0.00670547552594285,0.0149822164979267,-0.00165308775501769));
#23496=CARTESIAN_POINT('',(0.00601969772888137,0.0150339478312605,-0.00338516475340689));
#23497=CARTESIAN_POINT('',(0.00549746087916084,0.0150598134979274,-0.00418019437540437));
#23498=CARTESIAN_POINT('',(0.00418019438188475,0.0151115448312611,-0.00549746088567498));
#23499=CARTESIAN_POINT('',(0.00338516473432918,0.015137410497928,-0.00601969777394812));
#23500=CARTESIAN_POINT('',(0.00165308777405119,0.0151891418312618,-0.00670547548089361));
#23501=CARTESIAN_POINT('',(0.000716040461328761,0.0152150074979286,-0.00686901629956595));
#23502=CARTESIAN_POINT('',(-0.00114593663251221,0.0152667388312622,-0.00681050167388406));
#23503=CARTESIAN_POINT('',(-0.00207086641363077,0.0152926044979289,-0.00658844622952983));
#23504=CARTESIAN_POINT('',(-0.00375646449408611,0.0153443358312623,-0.00579526231015681));
#23505=CARTESIAN_POINT('',(-0.00451713279342289,0.015370201497929,-0.00522413383513803));
#23506=CARTESIAN_POINT('',(-0.00574909082729462,0.0154219328312622,-0.00382675978225479));
#23507=CARTESIAN_POINT('',(-0.00622038056182957,0.0154477984979287,-0.00300051420439034));
#23508=CARTESIAN_POINT('',(-0.00679603696289688,0.0154995298312617,-0.00122877622379433));
#23509=CARTESIAN_POINT('',(-0.00690040362942923,0.0155253954979281,-0.000283283821062771));
#23510=CARTESIAN_POINT('',(-0.00674400321434594,0.0155715558262137,0.00137155614196259));
#23511=CARTESIAN_POINT('',(-0.0065570379366458,0.0155918504878329,0.00208790417995068));
#23512=CARTESIAN_POINT('',(-0.00626290611822919,0.0156121451494521,0.00275705833899229));
#23513=CARTESIAN_POINT('',(-0.00657663816783462,0.0144040190010226,0.00232114617724482));
#23514=CARTESIAN_POINT('',(-0.00632830737432266,0.0144243137222126,0.00302351342913078));
#23515=CARTESIAN_POINT('',(-0.00596742914411203,0.0144446084434027,0.00368617521212354));
#23516=CARTESIAN_POINT('',(-0.00492907070058215,0.0144907688312591,0.00502477246815869));
#23517=CARTESIAN_POINT('',(-0.00419187524792228,0.0145166344979255,0.00565441906934018));
#23518=CARTESIAN_POINT('',(-0.00252807239237249,0.0145683658312584,0.00656912031052029));
#23519=CARTESIAN_POINT('',(-0.00160146498948257,0.014594231497925,0.00685417495051891));
#23520=CARTESIAN_POINT('',(0.000288754839060511,0.0146459628312582,0.00703284788809851));
#23521=CARTESIAN_POINT('',(0.00125236726471367,0.0146718284979248,0.00692646618567949));
#23522=CARTESIAN_POINT('',(0.00305808875011229,0.0147235598312582,0.00633975332869435));
#23523=CARTESIAN_POINT('',(0.00390019780985774,0.014749425497925,0.00585942217412823));
#23524=CARTESIAN_POINT('',(0.0053243942333875,0.0148011568312586,0.00460382363656548));
#23525=CARTESIAN_POINT('',(0.00590648159717181,0.0148270224979254,0.00382855625356886));
#23526=CARTESIAN_POINT('',(0.0067148864234727,0.0148787538312591,0.00211060871692616));
#23527=CARTESIAN_POINT('',(0.00694120388598928,0.014904619497926,0.00116792856328008));
#23528=CARTESIAN_POINT('',(0.00700084183758095,0.0149563508312598,-0.000729782125225469));
#23529=CARTESIAN_POINT('',(0.00683416232665603,0.0149822164979267,-0.00168481266008494));
#23530=CARTESIAN_POINT('',(0.00613522356131385,0.0150339478312605,-0.00345013046990494));
#23531=CARTESIAN_POINT('',(0.00560296430689659,0.0150598134979274,-0.00426041774486547));
#23532=CARTESIAN_POINT('',(0.00426041775147021,0.0151115448312612,-0.00560296431353574));
#23533=CARTESIAN_POINT('',(0.0034501304504611,0.015137410497928,-0.00613522360724549));
#23534=CARTESIAN_POINT('',(0.00168481267948373,0.0151891418312618,-0.00683416228074224));
#23535=CARTESIAN_POINT('',(0.000729782209515462,0.0152150074979286,-0.00700084166052923));
#23536=CARTESIAN_POINT('',(-0.00116792864761801,0.0152667388312622,-0.00694120406303948));
#23537=CARTESIAN_POINT('',(-0.00211060903478322,0.0152926044979289,-0.00671488708576274));
#23538=CARTESIAN_POINT('',(-0.00382855593575439,0.0153443358312623,-0.00590648093486172));
#23539=CARTESIAN_POINT('',(-0.00460382244956036,0.015370201497929,-0.00532439176123744));
#23540=CARTESIAN_POINT('',(-0.00585942336116365,0.0154219328312622,-0.00390020028197342));
#23541=CARTESIAN_POINT('',(-0.00633975775896098,0.0154477984979287,-0.00305809797633367));
#23542=CARTESIAN_POINT('',(-0.00692646175542653,0.0154995298312617,-0.00125235803845024));
#23543=CARTESIAN_POINT('',(-0.00703283135409475,0.0155253954979281,-0.000288720406206559));
#23544=CARTESIAN_POINT('',(-0.00687342941153299,0.0155715558262137,0.00139787808903776));
#23545=CARTESIAN_POINT('',(-0.00668287602686883,0.0155918504878329,0.00212797377800887));
#23546=CARTESIAN_POINT('',(-0.00638309943612347,0.0156121451494521,0.00280996987608639));
#23547=CARTESIAN_POINT('',(-0.00680066256085005,0.0143268259409887,0.00240021292079786));
#23548=CARTESIAN_POINT('',(-0.00654387271061886,0.0143471206621787,0.00312650537477982));
#23549=CARTESIAN_POINT('',(-0.00617070164561753,0.0143674153833687,0.00381173984611592));
#23550=CARTESIAN_POINT('',(-0.00509697290892147,0.0144135757712251,0.00519593462935609));
#23551=CARTESIAN_POINT('',(-0.00433466587803557,0.0144394414378915,0.00584702930081972));
#23552=CARTESIAN_POINT('',(-0.00261418780099725,0.0144911727712245,0.00679288861776992));
#23553=CARTESIAN_POINT('',(-0.00165601675484485,0.014517038437891,0.00708765326325648));
#23554=CARTESIAN_POINT('',(0.000298590886886155,0.0145687697712242,0.00727241245575358));
#23555=CARTESIAN_POINT('',(0.00129502748246475,0.0145946354378909,0.00716240700276411));
#23556=CARTESIAN_POINT('',(0.00316225845787908,0.0146463667712243,0.00655570855613481));
#23557=CARTESIAN_POINT('',(0.00403305283771481,0.014672232437891,0.00605901556249498));
#23558=CARTESIAN_POINT('',(0.00550576260973262,0.0147239637712246,0.00476064673818843));
#23559=CARTESIAN_POINT('',(0.00610767800191471,0.0147498294378915,0.0039589709075217));
#23560=CARTESIAN_POINT('',(0.00694362005862133,0.0148015607712252,0.00218250378316456));
#23561=CARTESIAN_POINT('',(0.00717764672314587,0.014827426437892,0.00120771248947415));
#23562=CARTESIAN_POINT('',(0.00723931616188416,0.0148791577712258,-0.000754641178356403));
#23563=CARTESIAN_POINT('',(0.00706695893609793,0.0149050234378927,-0.00174220355249655));
#23564=CARTESIAN_POINT('',(0.00634421175547352,0.0149567547712265,-0.00356765455510164));
#23565=CARTESIAN_POINT('',(0.00579382180063536,0.0149826204378934,-0.00440554318356661));
#23566=CARTESIAN_POINT('',(0.00440554319039633,0.0150343517712272,-0.00579382180750066));
#23567=CARTESIAN_POINT('',(0.00356765453499547,0.0150602174378941,-0.00634421180296976));
#23568=CARTESIAN_POINT('',(0.00174220357255612,0.0151119487712278,-0.00706695888862014));
#23569=CARTESIAN_POINT('',(0.000754641265517627,0.0151378144378947,-0.00723931597880142));
#23570=CARTESIAN_POINT('',(-0.00120771257668493,0.0151895457712282,-0.00717764690622705));
#23571=CARTESIAN_POINT('',(-0.00218250411184899,0.015215411437895,-0.00694362074347139));
#23572=CARTESIAN_POINT('',(-0.00395897057888131,0.0152671427712284,-0.00610767731704391));
#23573=CARTESIAN_POINT('',(-0.00476064551074956,0.015293008437895,-0.00550576005337207));
#23574=CARTESIAN_POINT('',(-0.00605901678996518,0.0153447397712283,-0.0040330553940398));
#23575=CARTESIAN_POINT('',(-0.00655571313731255,0.0153706054378948,-0.00316226799837936));
#23576=CARTESIAN_POINT('',(-0.00716240242160049,0.0154223367712278,-0.00129501794192098));
#23577=CARTESIAN_POINT('',(-0.00727239535854106,0.0154482024378941,-0.000298555281123038));
#23578=CARTESIAN_POINT('',(-0.00710756360176169,0.0154943627661797,0.00144549493862177));
#23579=CARTESIAN_POINT('',(-0.00691051927062198,0.015514657427799,0.0022004603618539));
#23580=CARTESIAN_POINT('',(-0.00660053119080453,0.0155349520894182,0.00290568774588812));
#23581=CARTESIAN_POINT('',(-0.00690084931513019,0.0142496328809547,0.00243557264346669));
#23582=CARTESIAN_POINT('',(-0.00664027645972905,0.0142699276021447,0.00317256477310107));
#23583=CARTESIAN_POINT('',(-0.00626160787188208,0.0142902223233348,0.00386789405755129));
#23584=CARTESIAN_POINT('',(-0.00517206105920528,0.0143363827111912,0.00527248067487872));
#23585=CARTESIAN_POINT('',(-0.00439852378913223,0.0143622483778576,0.00593316721496976));
#23586=CARTESIAN_POINT('',(-0.00265269978251628,0.0144139797111905,0.00689296084701396));
#23587=CARTESIAN_POINT('',(-0.00168041304597338,0.014439845377857,0.00719206793896712));
#23588=CARTESIAN_POINT('',(0.000302989701199774,0.0144915767111902,0.007379548987409));
#23589=CARTESIAN_POINT('',(0.00131410571183002,0.0145174423778569,0.00726792294389772));
#23590=CARTESIAN_POINT('',(0.00320884456743164,0.0145691737111903,0.00665228666986547));
#23591=CARTESIAN_POINT('',(0.00409246741240301,0.0145950393778571,0.0061482764393445));
#23592=CARTESIAN_POINT('',(0.00558687301342791,0.0146467707111907,0.00483078016132268));
#23593=CARTESIAN_POINT('',(0.00619765576948144,0.0146726363778575,0.00401729411382184));
#23594=CARTESIAN_POINT('',(0.00704591285000792,0.0147243677111912,0.00221465623423575));
#23595=CARTESIAN_POINT('',(0.00728338717448087,0.0147502333778581,0.0012255044021505));
#23596=CARTESIAN_POINT('',(0.00734596512189023,0.0148019647111919,-0.000765758484887816));
#23597=CARTESIAN_POINT('',(0.00717106874482664,0.0148278303778588,-0.00176786953984089));
#23598=CARTESIAN_POINT('',(0.00643767411720071,0.0148795617111926,-0.00362021292380031));
#23599=CARTESIAN_POINT('',(0.00587917586663838,0.0149054273778595,-0.00447044525280665));
#23600=CARTESIAN_POINT('',(0.00447044525973699,0.0149571587111933,-0.00587917587360483));
#23601=CARTESIAN_POINT('',(0.00362021290339794,0.0149830243778601,-0.00643767416539666));
#23602=CARTESIAN_POINT('',(0.00176786956019598,0.0150347557111939,-0.00717106869664941));
#23603=CARTESIAN_POINT('',(0.000765758573333092,0.0150606213778607,-0.00734596493611033));
#23604=CARTESIAN_POINT('',(-0.00122550449064606,0.0151123527111943,-0.0072833873602592));
#23605=CARTESIAN_POINT('',(-0.00221465656776232,0.015138218377861,-0.00704591354494714));
#23606=CARTESIAN_POINT('',(-0.00401729378033993,0.0151899497111945,-0.00619765507452119));
#23607=CARTESIAN_POINT('',(-0.00483077891580129,0.0152158153778611,-0.00558687041940729));
#23608=CARTESIAN_POINT('',(-0.00614827768489768,0.0152675467111943,-0.00409247000638756));
#23609=CARTESIAN_POINT('',(-0.00665229131853271,0.0152934123778609,-0.00320885424848173));
#23610=CARTESIAN_POINT('',(-0.00726791829524481,0.0153451437111938,-0.00131409603073581));
#23611=CARTESIAN_POINT('',(-0.00737953163832187,0.0153710093778602,-0.00030295357089573));
#23612=CARTESIAN_POINT('',(-0.00721227159480333,0.0154171697061458,0.00146678984113062));
#23613=CARTESIAN_POINT('',(-0.0070123244241521,0.015437464367765,0.00223287734764075));
#23614=CARTESIAN_POINT('',(-0.00669776962759131,0.0154577590293842,0.00294849407859576));
#23615=CARTESIAN_POINT('',(-0.00703930400432278,0.0140475388260902,0.00248443857836225));
#23616=CARTESIAN_POINT('',(-0.0067735031643564,0.0140678335472802,0.00323621729607965));
#23617=CARTESIAN_POINT('',(-0.0063872371867907,0.0140881282684702,0.00394549726914353));
#23618=CARTESIAN_POINT('',(-0.00527583033074515,0.0141342886563267,0.00537826470808661));
#23619=CARTESIAN_POINT('',(-0.00448677325181727,0.014160154322993,0.0060522068846051));
#23620=CARTESIAN_POINT('',(-0.00270592203200148,0.014211885656326,0.00703125726649926));
#23621=CARTESIAN_POINT('',(-0.00171412789111358,0.0142377513229925,0.00733636547187492));
#23622=CARTESIAN_POINT('',(0.000309068713070991,0.0142894826563257,0.00752760803272));
#23623=CARTESIAN_POINT('',(0.00134047117636765,0.0143153483229924,0.00741374238818943));
#23624=CARTESIAN_POINT('',(0.00327322498742965,0.0143670796563258,0.00678575434047188));
#23625=CARTESIAN_POINT('',(0.00417457633519498,0.0143929453229926,0.00627163193728491));
#23626=CARTESIAN_POINT('',(0.00569896483449358,0.0144446766563261,0.00492770216834684));
#23627=CARTESIAN_POINT('',(0.00632200198602683,0.014470542322993,0.00409789480259574));
#23628=CARTESIAN_POINT('',(0.00718727801090009,0.0145222736563267,0.0022590898287945));
#23629=CARTESIAN_POINT('',(0.00742951688424009,0.0145481393229936,0.00125009222074435));
#23630=CARTESIAN_POINT('',(0.00749335035975378,0.0145998706563273,-0.000781122224650873));
#23631=CARTESIAN_POINT('',(0.00731494496192747,0.0146257363229942,-0.00180333906199595));
#23632=CARTESIAN_POINT('',(0.00656683592443885,0.014677467656328,-0.0036928468029486));
#23633=CARTESIAN_POINT('',(0.00599713228477656,0.014703333322995,-0.00456013770655619));
#23634=CARTESIAN_POINT('',(0.00456013771362558,0.0147550646563287,-0.00599713229188277));
#23635=CARTESIAN_POINT('',(0.00369284678213689,0.0147809303229956,-0.00656683597360177));
#23636=CARTESIAN_POINT('',(0.00180333908275944,0.0148326616563293,-0.00731494491278363));
#23637=CARTESIAN_POINT('',(0.000781122314870668,0.0148585273229961,-0.0074933501702465));
#23638=CARTESIAN_POINT('',(-0.00125009231101543,0.0149102586563297,-0.00742951707374577));
#23639=CARTESIAN_POINT('',(-0.00225909016901275,0.0149361243229965,-0.00718727871978218));
#23640=CARTESIAN_POINT('',(-0.00409789446242306,0.0149878556563299,-0.0063220012771233));
#23641=CARTESIAN_POINT('',(-0.00492770089783603,0.0150137213229966,-0.005698962188428));
#23642=CARTESIAN_POINT('',(-0.00627163320782816,0.0150654526563298,-0.00417457898122375));
#23643=CARTESIAN_POINT('',(-0.00678575908240733,0.0150913183229963,-0.00327323486271478));
#23644=CARTESIAN_POINT('',(-0.00741373764626861,0.0151430496563293,-0.00134046130103752));
#23645=CARTESIAN_POINT('',(-0.00752759033555073,0.0151689153229957,-0.000309031857869217));
#23646=CARTESIAN_POINT('',(-0.0073569744822931,0.0152150756512812,0.00149621867261073));
#23647=CARTESIAN_POINT('',(-0.00715301568610083,0.0152353703129005,0.00227767652018535));
#23648=CARTESIAN_POINT('',(-0.00683214984221773,0.0152556649745197,0.00300765097546396));
#23649=CARTESIAN_POINT('',(-0.00707757193923525,0.0139226378312596,0.00249794479058897));
#23650=CARTESIAN_POINT('',(-0.00681032611987357,0.0139429325524497,0.003253810420737));
#23651=CARTESIAN_POINT('',(-0.00642196027543476,0.0139632272736397,0.00396694626930039));
#23652=CARTESIAN_POINT('',(-0.0053045114520012,0.0140093876614961,0.00540750269577186));
#23653=CARTESIAN_POINT('',(-0.00451116480340562,0.0140352533281625,0.0060851086400904));
#23654=CARTESIAN_POINT('',(-0.00272063229996764,0.0140869846614954,0.00706948145674052));
#23655=CARTESIAN_POINT('',(-0.00172344644512523,0.014112850328162,0.00737624832907208));
#23656=CARTESIAN_POINT('',(0.000310748910628593,0.0141645816614952,0.00756853054637559));
#23657=CARTESIAN_POINT('',(0.00134775841154002,0.0141904473281618,0.00745404589134753));
#23658=CARTESIAN_POINT('',(0.0032910192978751,0.0142421786614952,0.00682264389734763));
#23659=CARTESIAN_POINT('',(0.00419727068329876,0.014268044328162,0.0063057265583758));
#23660=CARTESIAN_POINT('',(0.00572994625186395,0.0143197756614956,0.00495449075223675));
#23661=CARTESIAN_POINT('',(0.00635637043500549,0.0143456413281624,0.00412017228506952));
#23662=CARTESIAN_POINT('',(0.00722635038040567,0.0143973726614961,0.00227137097228208));
#23663=CARTESIAN_POINT('',(0.00746990614266432,0.014423238328163,0.00125688812666185));
#23664=CARTESIAN_POINT('',(0.00753408663761127,0.0144749696614968,-0.000785368657882517));
#23665=CARTESIAN_POINT('',(0.00735471137029958,0.0145008353281637,-0.00181314259680666));
#23666=CARTESIAN_POINT('',(0.00660253536994981,0.0145525666614975,-0.00371292231339824));
#23667=CARTESIAN_POINT('',(0.00602973463691172,0.0145784323281644,-0.00458492809106568));
#23668=CARTESIAN_POINT('',(0.00458492809817352,0.0146301636614982,-0.00602973464405655));
#23669=CARTESIAN_POINT('',(0.0037129222924734,0.014656029328165,-0.00660253541937998));
#23670=CARTESIAN_POINT('',(0.00181314261768302,0.0147077606614987,-0.00735471132088858));
#23671=CARTESIAN_POINT('',(0.000785368748592778,0.0147336263281656,-0.00753408644707376));
#23672=CARTESIAN_POINT('',(-0.00125688821742367,0.0147853576614992,-0.0074699063332002));
#23673=CARTESIAN_POINT('',(-0.00227137131434987,0.0148112233281659,-0.00722635109314147));
#23674=CARTESIAN_POINT('',(-0.00412017194304755,0.0148629546614994,-0.00635636972224812));
#23675=CARTESIAN_POINT('',(-0.00495448947481904,0.014888820328166,-0.0057299435914135));
#23676=CARTESIAN_POINT('',(-0.00630572783582616,0.0149405516614992,-0.00419727334371219));
#23677=CARTESIAN_POINT('',(-0.00682264866506178,0.0149664173281658,-0.00329102922684548));
#23678=CARTESIAN_POINT('',(-0.0074540411236481,0.0150181486614987,-0.0013477484825244));
#23679=CARTESIAN_POINT('',(-0.00756851275299878,0.0150440143281651,-0.000310711855070012));
#23680=CARTESIAN_POINT('',(-0.00739696937674122,0.0150901746564507,0.00150435260158199));
#23681=CARTESIAN_POINT('',(-0.00719190179451943,0.01511046931807,0.0022900587069431));
#23682=CARTESIAN_POINT('',(-0.00686929162005737,0.0151307639796891,0.00302400153962454));
#23683=CARTESIAN_POINT('',(-0.00707757193923526,0.0137939897455748,0.00249794479058897));
#23684=CARTESIAN_POINT('',(-0.00681032611987357,0.0138142844667648,0.003253810420737));
#23685=CARTESIAN_POINT('',(-0.00642196027543476,0.0138345791879549,0.00396694626930039));
#23686=CARTESIAN_POINT('',(-0.0053045114520012,0.0138807395758113,0.00540750269577185));
#23687=CARTESIAN_POINT('',(-0.00451116480340562,0.0139066052424777,0.0060851086400904));
#23688=CARTESIAN_POINT('',(-0.00272063229996764,0.0139583365758106,0.00706948145674052));
#23689=CARTESIAN_POINT('',(-0.00172344644512524,0.0139842022424771,0.00737624832907208));
#23690=CARTESIAN_POINT('',(0.000310748910628593,0.0140359335758103,0.00756853054637559));
#23691=CARTESIAN_POINT('',(0.00134775841154002,0.014061799242477,0.00745404589134753));
#23692=CARTESIAN_POINT('',(0.0032910192978751,0.0141135305758104,0.00682264389734764));
#23693=CARTESIAN_POINT('',(0.00419727068329876,0.0141393962424772,0.00630572655837581));
#23694=CARTESIAN_POINT('',(0.00572994625186395,0.0141911275758108,0.00495449075223675));
#23695=CARTESIAN_POINT('',(0.00635637043500548,0.0142169932424776,0.00412017228506952));
#23696=CARTESIAN_POINT('',(0.00722635038040566,0.0142687245758113,0.00227137097228208));
#23697=CARTESIAN_POINT('',(0.00746990614266432,0.0142945902424782,0.00125688812666185));
#23698=CARTESIAN_POINT('',(0.00753408663761127,0.014346321575812,-0.000785368657882514));
#23699=CARTESIAN_POINT('',(0.00735471137029958,0.0143721872424789,-0.00181314259680666));
#23700=CARTESIAN_POINT('',(0.00660253536994981,0.0144239185758127,-0.00371292231339824));
#23701=CARTESIAN_POINT('',(0.00602973463691172,0.0144497842424796,-0.00458492809106569));
#23702=CARTESIAN_POINT('',(0.00458492809817352,0.0145015155758134,-0.00602973464405656));
#23703=CARTESIAN_POINT('',(0.0037129222924734,0.0145273812424802,-0.00660253541937998));
#23704=CARTESIAN_POINT('',(0.00181314261768302,0.0145791125758139,-0.00735471132088859));
#23705=CARTESIAN_POINT('',(0.000785368748592778,0.0146049782424808,-0.00753408644707376));
#23706=CARTESIAN_POINT('',(-0.00125688821742367,0.0146567095758144,-0.0074699063332002));
#23707=CARTESIAN_POINT('',(-0.00227137131434987,0.0146825752424811,-0.00722635109314146));
#23708=CARTESIAN_POINT('',(-0.00412017194304755,0.0147343065758145,-0.00635636972224813));
#23709=CARTESIAN_POINT('',(-0.00495448947481902,0.0147601722424812,-0.00572994359141352));
#23710=CARTESIAN_POINT('',(-0.00630572783582614,0.0148119035758144,-0.0041972733437122));
#23711=CARTESIAN_POINT('',(-0.00682264866506178,0.0148377692424809,-0.00329102922684549));
#23712=CARTESIAN_POINT('',(-0.0074540411236481,0.0148895005758139,-0.0013477484825244));
#23713=CARTESIAN_POINT('',(-0.00756851275299878,0.0149153662424803,-0.000310711855070013));
#23714=CARTESIAN_POINT('',(-0.00739696937674121,0.0149615265707659,0.00150435260158199));
#23715=CARTESIAN_POINT('',(-0.00719190179451944,0.0149818212323851,0.0022900587069431));
#23716=CARTESIAN_POINT('',(-0.00686929162005737,0.0150021158940043,0.00302400153962454));
#23717=CARTESIAN_POINT('',(-0.00707753749697229,0.0137902426547206,0.00249793263460213));
#23718=CARTESIAN_POINT('',(-0.0068102929781344,0.0138105373759106,0.00325379458640919));
#23719=CARTESIAN_POINT('',(-0.00642192902363732,0.0138308320971006,0.00396692696457162));
#23720=CARTESIAN_POINT('',(-0.00530448563815149,0.013876992484957,0.00540747638072603));
#23721=CARTESIAN_POINT('',(-0.00451114285029432,0.0139028581516234,0.00608507902754618));
#23722=CARTESIAN_POINT('',(-0.00272061906029534,0.0139545894849563,0.00706944705384903));
#23723=CARTESIAN_POINT('',(-0.00172343805815352,0.0139804551516229,0.00737621243333172));
#23724=CARTESIAN_POINT('',(0.000310747398401548,0.0140321864849561,0.00756849371491394));
#23725=CARTESIAN_POINT('',(0.00134775185281479,0.0140580521516227,0.00745400961701348));
#23726=CARTESIAN_POINT('',(0.00329100328247419,0.0141097834849562,0.00682261069566529));
#23727=CARTESIAN_POINT('',(0.00419725025772034,0.0141356491516229,0.00630569587221758));
#23728=CARTESIAN_POINT('',(0.00572991836768031,0.0141873804849565,0.00495446664172613));
#23729=CARTESIAN_POINT('',(0.00635633950239413,0.0142132461516233,0.00412015223468239));
#23730=CARTESIAN_POINT('',(0.00722631521412797,0.0142649774849571,0.00227135991889301));
#23731=CARTESIAN_POINT('',(0.00746986979114801,0.0142908431516239,0.00125688201014735));
#23732=CARTESIAN_POINT('',(0.0075340499737673,0.0143425744849577,-0.000785364835968151));
#23733=CARTESIAN_POINT('',(0.00735467557936657,0.0143684401516246,-0.00181313377333801));
#23734=CARTESIAN_POINT('',(0.00660250323940257,0.0144201714849584,-0.00371290424485047));
#23735=CARTESIAN_POINT('',(0.00602970529383929,0.0144460371516253,-0.00458490577899308));
#23736=CARTESIAN_POINT('',(0.00458490578610087,0.0144977684849591,-0.0060297053009841));
#23737=CARTESIAN_POINT('',(0.00371290422392572,0.014523634151626,-0.0066025032888325));
#23738=CARTESIAN_POINT('',(0.00181313379421427,0.0145753654849597,-0.00735467552995582));
#23739=CARTESIAN_POINT('',(0.000785364926677974,0.0146012311516265,-0.00753404978323072));
#23740=CARTESIAN_POINT('',(-0.00125688210090873,0.0146529624849601,-0.00746986998168296));
#23741=CARTESIAN_POINT('',(-0.00227136026095913,0.0146788281516269,-0.00722631592686031));
#23742=CARTESIAN_POINT('',(-0.00412015189266208,0.0147305594849603,-0.00635633878964025));
#23743=CARTESIAN_POINT('',(-0.00495446536431462,0.0147564251516269,-0.00572991570724283));
#23744=CARTESIAN_POINT('',(-0.0063056971496617,0.0148081564849601,-0.00419725291812084));
#23745=CARTESIAN_POINT('',(-0.00682261546335623,0.0148340221516267,-0.00329101321139626));
#23746=CARTESIAN_POINT('',(-0.00745400484933725,0.0148857534849596,-0.00134774192384749));
#23747=CARTESIAN_POINT('',(-0.00756847592162372,0.014911619151626,-0.000310710343023295));
#23748=CARTESIAN_POINT('',(-0.00739693338016404,0.0149577794799116,0.00150434528080753));
#23749=CARTESIAN_POINT('',(-0.00719186679588219,0.0149780741415309,0.00229004756261212));
#23750=CARTESIAN_POINT('',(-0.00686925819136877,0.0149983688031501,0.0030239868236376));
#23751=CARTESIAN_POINT('',(-0.00707746880978615,0.0137864962079549,0.00249790839227718));
#23752=CARTESIAN_POINT('',(-0.00681022688454442,0.0138067909291449,0.00325376300847767));
#23753=CARTESIAN_POINT('',(-0.00642186669910222,0.013827085650335,0.00396688846572214));
#23754=CARTESIAN_POINT('',(-0.00530443415835466,0.0138732460381914,0.00540742390140863));
#23755=CARTESIAN_POINT('',(-0.00451109906985392,0.0138991117048577,0.00608501997212528));
#23756=CARTESIAN_POINT('',(-0.00272059265680856,0.0139508430381907,0.00706937844518029));
#23757=CARTESIAN_POINT('',(-0.00172342133226394,0.0139767087048572,0.00737614084751863));
#23758=CARTESIAN_POINT('',(0.000310744382611889,0.0140284400381904,0.00756842026301959));
#23759=CARTESIAN_POINT('',(0.0013477387729431,0.0140543057048571,0.00745393727618219));
#23760=CARTESIAN_POINT('',(0.00329097134343394,0.0141060370381905,0.00682254448253241));
#23761=CARTESIAN_POINT('',(0.00419720952359356,0.0141319027048573,0.00630563467572004));
#23762=CARTESIAN_POINT('',(0.0057298627590778,0.0141836340381909,0.00495441855884807));
#23763=CARTESIAN_POINT('',(0.00635627781440241,0.0142094997048577,0.00412011224878849));
#23764=CARTESIAN_POINT('',(0.00722624508306073,0.0142612310381914,0.00227133787544617));
#23765=CARTESIAN_POINT('',(0.00746979729639444,0.0142870967048583,0.00125686981216344));
#23766=CARTESIAN_POINT('',(0.00753397685614792,0.014338828038192,-0.000785357214037403));
#23767=CARTESIAN_POINT('',(0.0073546042025677,0.0143646937048589,-0.00181311617695551));
#23768=CARTESIAN_POINT('',(0.00660243916240275,0.0144164250381928,-0.00371286821128017));
#23769=CARTESIAN_POINT('',(0.00602964677581802,0.0144422907048597,-0.00458486128268673));
#23770=CARTESIAN_POINT('',(0.00458486128979446,0.0144940220381934,-0.00602964678296275));
#23771=CARTESIAN_POINT('',(0.00371286819035562,0.0145198877048603,-0.0066024392118322));
#23772=CARTESIAN_POINT('',(0.00181311619783157,0.014571619038194,-0.00735460415315743));
#23773=CARTESIAN_POINT('',(0.000785357304746346,0.0145974847048609,-0.00753397666561319));
#23774=CARTESIAN_POINT('',(-0.00125686990292393,0.0146492160381944,-0.00746979748692755));
#23775=CARTESIAN_POINT('',(-0.00227133821750898,0.0146750817048612,-0.00722624579578614));
#23776=CARTESIAN_POINT('',(-0.00412011190677149,0.0147268130381946,-0.00635627710165544));
#23777=CARTESIAN_POINT('',(-0.00495441728144896,0.0147526787048613,-0.00572986009866614));
#23778=CARTESIAN_POINT('',(-0.00630563595315176,0.0148044100381945,-0.00419721218396824));
#23779=CARTESIAN_POINT('',(-0.00682254925017708,0.014830275704861,-0.00329098127225964));
#23780=CARTESIAN_POINT('',(-0.00745393250855223,0.0148820070381939,-0.00134772884407215));
#23781=CARTESIAN_POINT('',(-0.00756840246990205,0.0149078727048603,-0.000310707327593257));
#23782=CARTESIAN_POINT('',(-0.00739686159325509,0.0149540330331459,0.00150433068120359));
#23783=CARTESIAN_POINT('',(-0.0071917969991353,0.0149743276947652,0.00229002533780254));
#23784=CARTESIAN_POINT('',(-0.00686919152552402,0.0149946223563844,0.00302395747598018));
#23785=CARTESIAN_POINT('',(-0.00586834142534816,0.0138049000898792,0.002323445101092));
#23786=CARTESIAN_POINT('',(-0.00586834150722695,0.0139610262791494,0.00232344513351016));
#23787=CARTESIAN_POINT('',(-0.00598853868710003,0.0142723828532714,0.00237103465301815));
#23788=CARTESIAN_POINT('',(-0.00642329524186585,0.0144661077682987,0.00254316727348483));
#23789=CARTESIAN_POINT('',(-0.00685805179684844,0.014272382853826,0.00271529989403731));
#23790=CARTESIAN_POINT('',(-0.00697824897705869,0.0139610262798587,0.00276288941367881));
#23791=CARTESIAN_POINT('',(-0.00697824905911604,0.0138049000905885,0.00276288944616767));
#23792=CARTESIAN_POINT('',(-0.00713652355335438,0.00998404077070117,0.0023190372625396));
#23793=CARTESIAN_POINT('',(-0.00682689162296045,0.0101213963498648,0.00327188765430387));
#23794=CARTESIAN_POINT('',(-0.00632393975032057,0.0102552176634611,0.00416165210870539));
#23795=CARTESIAN_POINT('',(-0.00501082465149917,0.0105157917595189,0.00567474585832276));
#23796=CARTESIAN_POINT('',(-0.00420066142531763,0.0106425445419805,0.00629807515353861));
#23797=CARTESIAN_POINT('',(-0.0024014310390604,0.0108889815757688,0.00717946112362713));
#23798=CARTESIAN_POINT('',(-0.00141236387898469,0.0110086658270955,0.0074375177984998));
#23799=CARTESIAN_POINT('',(0.000588110521868161,0.0112409657986143,0.00754754861489316));
#23800=CARTESIAN_POINT('',(0.00159951776264531,0.0113535815188063,0.00739952275641386));
#23801=CARTESIAN_POINT('',(0.00348455427698092,0.0115717444280555,0.00672081082698304));
#23802=CARTESIAN_POINT('',(0.00435818355053937,0.0116772916171128,0.00619012475603152));
#23803=CARTESIAN_POINT('',(0.0058293622098697,0.0118813174640925,0.00483010756411885));
#23804=CARTESIAN_POINT('',(0.00642691159564158,0.0119797961220149,0.00400077644315771));
#23805=CARTESIAN_POINT('',(0.00725133308312823,0.0121696849067251,0.00217475847441996));
#23806=CARTESIAN_POINT('',(0.00747820518484301,0.0122610950335128,0.00117807162664336));
#23807=CARTESIAN_POINT('',(0.00752535639799984,0.0124368467559534,-0.000824873608022594));
#23808=CARTESIAN_POINT('',(0.0073456355094419,0.0125211883516063,-0.00183113199491196));
#23809=CARTESIAN_POINT('',(0.00660805206922664,0.0126828030117774,-0.00369392112405686));
#23810=CARTESIAN_POINT('',(0.00605018951756932,0.0127600760762956,-0.00455045186631239));
#23811=CARTESIAN_POINT('',(0.00464463709803305,0.0129075536741971,-0.00597818967344566));
#23812=CARTESIAN_POINT('',(0.0037969472301541,0.0129777582075804,-0.00654939673832338));
#23813=CARTESIAN_POINT('',(0.00194593676290491,0.0131110987432124,-0.00731606006817175));
#23814=CARTESIAN_POINT('',(0.000942616163534665,0.013174234745461,-0.00751151633314239));
#23815=CARTESIAN_POINT('',(-0.00106082198265159,0.0132934382188234,-0.00749573645991879));
#23816=CARTESIAN_POINT('',(-0.0020609395294676,0.0133495056899372,-0.00728450032172455));
#23817=CARTESIAN_POINT('',(-0.0038996431192263,0.01345457210103,-0.00648877319979548));
#23818=CARTESIAN_POINT('',(-0.00473822916216899,0.0135035710410091,-0.00590428221606065));
#23819=CARTESIAN_POINT('',(-0.00612111958495,0.0135945003898323,-0.0044545861487252));
#23820=CARTESIAN_POINT('',(-0.00666542396478831,0.0136364307986766,-0.00358938106512457));
#23821=CARTESIAN_POINT('',(-0.00737356397402995,0.0137132230852302,-0.00171518552077393));
#23822=CARTESIAN_POINT('',(-0.00753739960343328,0.0137480849629397,-0.000706195060023929));
#23823=CARTESIAN_POINT('',(-0.00745873679850607,0.0138107401872238,0.00129568808368499));
#23824=CARTESIAN_POINT('',(-0.00721623836417553,0.0138385335337985,0.0022885807666439));
#23825=CARTESIAN_POINT('',(-0.00678963471291716,0.0138627926148057,0.00319511544670599));
#23826=CARTESIAN_POINT('',(-0.00713768608282461,0.00996866665836644,0.00231941503038975));
#23827=CARTESIAN_POINT('',(-0.0068280037138325,0.0101060222375301,0.00327242064011874));
#23828=CARTESIAN_POINT('',(-0.00632496991105259,0.0102398435511264,0.00416233003587611));
#23829=CARTESIAN_POINT('',(-0.00501164090766143,0.0105004176471842,0.00567567026629915));
#23830=CARTESIAN_POINT('',(-0.00420134570705017,0.0106271704296457,0.00629910110096484));
#23831=CARTESIAN_POINT('',(-0.00240182222873878,0.010873607463434,0.00718063064756609));
#23832=CARTESIAN_POINT('',(-0.00141259395103865,0.0109932917147608,0.00743872935950167));
#23833=CARTESIAN_POINT('',(0.000588206324230238,0.0112255916862796,0.00754877809975751));
#23834=CARTESIAN_POINT('',(0.00159977832179899,0.0113382074064716,0.00740072812807777));
#23835=CARTESIAN_POINT('',(0.00348512190588417,0.0115563703157208,0.00672190563744528));
#23836=CARTESIAN_POINT('',(0.0043588934924006,0.011661917504778,0.00619113311849253));
#23837=CARTESIAN_POINT('',(0.00583031180462841,0.0118659433517577,0.00483089438172629));
#23838=CARTESIAN_POINT('',(0.00642795853033978,0.0119644220096802,0.0040014281639128));
#23839=CARTESIAN_POINT('',(0.00725251431490651,0.0121543107943904,0.00217511273946207));
#23840=CARTESIAN_POINT('',(0.00747942337376187,0.0122457209211781,0.00117826353282482));
#23841=CARTESIAN_POINT('',(0.00752658226778383,0.0124214726436187,-0.000825007978752457));
#23842=CARTESIAN_POINT('',(0.00734683210295042,0.0125058142392716,-0.00183143028369249));
#23843=CARTESIAN_POINT('',(0.00660912851144867,0.0126674288994427,-0.00369452285851977));
#23844=CARTESIAN_POINT('',(0.00605117508478032,0.0127447019639608,-0.00455119312840702));
#23845=CARTESIAN_POINT('',(0.00464539370276709,0.0128921795618623,-0.00597916351198512));
#23846=CARTESIAN_POINT('',(0.00379756574742221,0.0129623840952457,-0.00655046362567598));
#23847=CARTESIAN_POINT('',(0.00194625375321779,0.0130957246308777,-0.00731725184388323));
#23848=CARTESIAN_POINT('',(0.000942769714358262,0.0131588606331263,-0.00751273994839962));
#23849=CARTESIAN_POINT('',(-0.0010609947890339,0.0132780641064887,-0.00749695750465726));
#23850=CARTESIAN_POINT('',(-0.00206127525356652,0.0133341315776025,-0.00728568695639851));
#23851=CARTESIAN_POINT('',(-0.00390027836550772,0.0134391979886953,-0.00648983021166044));
#23852=CARTESIAN_POINT('',(-0.00473900101291629,0.0134881969286743,-0.00590524401518111));
#23853=CARTESIAN_POINT('',(-0.00612211670656743,0.0135791262774976,-0.00445531179443167));
#23854=CARTESIAN_POINT('',(-0.00666650975281,0.0136210566863418,-0.00358996577016154));
#23855=CARTESIAN_POINT('',(-0.00737476511704538,0.0136978489728955,-0.00171546492203982));
#23856=CARTESIAN_POINT('',(-0.00753862743503819,0.013732710850605,-0.000706310098188223));
#23857=CARTESIAN_POINT('',(-0.00745995181605267,0.0137953660748891,0.00129589914941892));
#23858=CARTESIAN_POINT('',(-0.00721741387907434,0.0138231594214637,0.00228895357317447));
#23859=CARTESIAN_POINT('',(-0.0067907407346919,0.013847418502471,0.00319563592643815));
#23860=CARTESIAN_POINT('',(-0.00713827428147907,0.0099532476683191,0.00231960616751517));
#23861=CARTESIAN_POINT('',(-0.00682856639234631,0.0100906032474828,0.00327269031202572));
#23862=CARTESIAN_POINT('',(-0.00632549113582319,0.010224424561079,0.00416267304296526));
#23863=CARTESIAN_POINT('',(-0.00501205390431109,0.0104849986571369,0.00567613798392852));
#23864=CARTESIAN_POINT('',(-0.00420169192932209,0.0106117514395984,0.00629962019395224));
#23865=CARTESIAN_POINT('',(-0.00240202015683297,0.0108581884733867,0.0071812223851735));
#23866=CARTESIAN_POINT('',(-0.00141271035933283,0.0109778727247134,0.00743934236637103));
#23867=CARTESIAN_POINT('',(0.00058825479682548,0.0112101726962322,0.00754940017546518));
#23868=CARTESIAN_POINT('',(0.00159991015548366,0.0113227884164242,0.00740133800336178));
#23869=CARTESIAN_POINT('',(0.00348540910596441,0.0115409513256735,0.00672245957268501));
#23870=CARTESIAN_POINT('',(0.00435925269778697,0.0116464985147307,0.00619164331411162));
#23871=CARTESIAN_POINT('',(0.00583079226587576,0.0118505243617104,0.00483129248351197));
#23872=CARTESIAN_POINT('',(0.00642848824214198,0.0119490030196329,0.0040017579114857));
#23873=CARTESIAN_POINT('',(0.00725311197626511,0.012138891804343,0.00217529198500073));
#23874=CARTESIAN_POINT('',(0.00748003973412201,0.0122303019311307,0.00117836063054201));
#23875=CARTESIAN_POINT('',(0.00752720251438913,0.0124060536535713,-0.000825075965573031));
#23876=CARTESIAN_POINT('',(0.00734743753679934,0.0124903952492243,-0.00183158120722935));
#23877=CARTESIAN_POINT('',(0.00660967315301072,0.0126520099093953,-0.0036948273148028));
#23878=CARTESIAN_POINT('',(0.00605167374681189,0.0127292829739135,-0.00455156818071995));
#23879=CARTESIAN_POINT('',(0.00464577651791106,0.012876760571815,-0.00597965623972514));
#23880=CARTESIAN_POINT('',(0.00379787869520906,0.0129469651051984,-0.0065510034328132));
#23881=CARTESIAN_POINT('',(0.00194641413906631,0.0130803056408303,-0.00731785484009783));
#23882=CARTESIAN_POINT('',(0.000942847405625574,0.0131434416430789,-0.0075133590542944));
#23883=CARTESIAN_POINT('',(-0.00106108222293055,0.0132626451164413,-0.00749757530996077));
#23884=CARTESIAN_POINT('',(-0.00206144511804593,0.0133187125875551,-0.00728628735143058));
#23885=CARTESIAN_POINT('',(-0.00390059977758161,0.013423778998648,-0.00649036502215139));
#23886=CARTESIAN_POINT('',(-0.0047393915420019,0.013472777938627,-0.00590573065140239));
#23887=CARTESIAN_POINT('',(-0.0061226212147186,0.0135637072874502,-0.0044556789454064));
#23888=CARTESIAN_POINT('',(-0.006667059123015,0.0136056376962945,-0.00359026161015942));
#23889=CARTESIAN_POINT('',(-0.00737537285278333,0.0136824299828482,-0.00171560628916457));
#23890=CARTESIAN_POINT('',(-0.00753924867425526,0.0137172918605576,-0.000706368303416719));
#23891=CARTESIAN_POINT('',(-0.00746056657181099,0.0137799470848417,0.00129600594118969));
#23892=CARTESIAN_POINT('',(-0.0072180086478948,0.0138077404314164,0.00228914220004825));
#23893=CARTESIAN_POINT('',(-0.00679130034245786,0.0138319995124236,0.0031958992707111));
#23894=CARTESIAN_POINT('',(-0.00713827428147907,0.00981292768344121,0.00231960616751517));
#23895=CARTESIAN_POINT('',(-0.0068285663923463,0.00995028326260487,0.00327269031202572));
#23896=CARTESIAN_POINT('',(-0.00632549113582319,0.0100841045762011,0.00416267304296526));
#23897=CARTESIAN_POINT('',(-0.00501205390431109,0.0103446786722589,0.00567613798392853));
#23898=CARTESIAN_POINT('',(-0.0042016919293221,0.0104714314547205,0.00629962019395224));
#23899=CARTESIAN_POINT('',(-0.00240202015683296,0.0107178684885088,0.0071812223851735));
#23900=CARTESIAN_POINT('',(-0.00141271035933283,0.0108375527398355,0.00743934236637104));
#23901=CARTESIAN_POINT('',(0.000588254796825484,0.0110698527113543,0.00754940017546518));
#23902=CARTESIAN_POINT('',(0.00159991015548366,0.0111824684315463,0.00740133800336179));
#23903=CARTESIAN_POINT('',(0.00348540910596441,0.0114006313407956,0.00672245957268501));
#23904=CARTESIAN_POINT('',(0.00435925269778698,0.0115061785298528,0.00619164331411163));
#23905=CARTESIAN_POINT('',(0.00583079226587577,0.0117102043768325,0.00483129248351197));
#23906=CARTESIAN_POINT('',(0.00642848824214199,0.011808683034755,0.00400175791148571));
#23907=CARTESIAN_POINT('',(0.00725311197626511,0.0119985718194651,0.00217529198500072));
#23908=CARTESIAN_POINT('',(0.00748003973412199,0.0120899819462528,0.001178360630542));
#23909=CARTESIAN_POINT('',(0.00752720251438914,0.0122657336686934,-0.000825075965573036));
#23910=CARTESIAN_POINT('',(0.00734743753679934,0.0123500752643464,-0.00183158120722935));
#23911=CARTESIAN_POINT('',(0.00660967315301072,0.0125116899245174,-0.0036948273148028));
#23912=CARTESIAN_POINT('',(0.00605167374681189,0.0125889629890356,-0.00455156818071994));
#23913=CARTESIAN_POINT('',(0.00464577651791106,0.0127364405869371,-0.00597965623972514));
#23914=CARTESIAN_POINT('',(0.00379787869520905,0.0128066451203205,-0.00655100343281321));
#23915=CARTESIAN_POINT('',(0.00194641413906632,0.0129399856559524,-0.00731785484009784));
#23916=CARTESIAN_POINT('',(0.000942847405625574,0.013003121658201,-0.00751335905429439));
#23917=CARTESIAN_POINT('',(-0.00106108222293055,0.0131223251315634,-0.00749757530996077));
#23918=CARTESIAN_POINT('',(-0.00206144511804593,0.0131783926026772,-0.00728628735143058));
#23919=CARTESIAN_POINT('',(-0.0039005997775816,0.01328345901377,-0.00649036502215138));
#23920=CARTESIAN_POINT('',(-0.0047393915420019,0.0133324579537491,-0.00590573065140239));
#23921=CARTESIAN_POINT('',(-0.00612262121471859,0.0134233873025723,-0.00445567894540641));
#23922=CARTESIAN_POINT('',(-0.006667059123015,0.0134653177114166,-0.00359026161015941));
#23923=CARTESIAN_POINT('',(-0.00737537285278332,0.0135421099979703,-0.00171560628916458));
#23924=CARTESIAN_POINT('',(-0.00753924867425525,0.0135769718756797,-0.000706368303416716));
#23925=CARTESIAN_POINT('',(-0.007460566571811,0.0136396270999638,0.0012960059411897));
#23926=CARTESIAN_POINT('',(-0.0072180086478948,0.0136674204465385,0.00228914220004825));
#23927=CARTESIAN_POINT('',(-0.00679130034245786,0.0136916795275457,0.0031958992707111));
#23928=CARTESIAN_POINT('',(-0.00709967813326097,0.00968802668861064,0.00230706421971116));
#23929=CARTESIAN_POINT('',(-0.00679164481295561,0.00982538226777431,0.00325499510512079));
#23930=CARTESIAN_POINT('',(-0.00629128964904872,0.0099592035813706,0.00414016576187539));
#23931=CARTESIAN_POINT('',(-0.00498495408049655,0.0102197776774284,0.00564544750408768));
#23932=CARTESIAN_POINT('',(-0.00417897367585126,0.0103465304598899,0.00626555858954536));
#23933=CARTESIAN_POINT('',(-0.00238903260237088,0.0105929674936782,0.00714239401957196));
#23934=CARTESIAN_POINT('',(-0.00140507193353578,0.010712651745005,0.00739911836414088));
#23935=CARTESIAN_POINT('',(0.00058507414441105,0.0109449517165238,0.00750858109838291));
#23936=CARTESIAN_POINT('',(0.00159125955352277,0.0110575674367158,0.00736131948805603));
#23937=CARTESIAN_POINT('',(0.00346656374346502,0.011275730345965,0.00668611170542376));
#23938=CARTESIAN_POINT('',(0.00433568252429554,0.0113812775350222,0.00615816553311837));
#23939=CARTESIAN_POINT('',(0.00579926558118299,0.0115853033820019,0.00480517002401746));
#23940=CARTESIAN_POINT('',(0.00639372985723993,0.0116837820399244,0.00398012068722193));
#23941=CARTESIAN_POINT('',(0.00721389490868832,0.0118736708246346,0.00216353033385647));
#23942=CARTESIAN_POINT('',(0.00743959568407976,0.0119650809514223,0.00117198931728653));
#23943=CARTESIAN_POINT('',(0.00748650345850291,0.0121408326738629,-0.00082061483771457));
#23944=CARTESIAN_POINT('',(0.00730771045753463,0.0122251742695158,-0.00182167797614574));
#23945=CARTESIAN_POINT('',(0.00657393511400755,0.0123867889296869,-0.00367484964274103));
#23946=CARTESIAN_POINT('',(0.00601895277144875,0.012464061994205,-0.00452695817090515));
#23947=CARTESIAN_POINT('',(0.00462065713022673,0.0126115395921065,-0.00594732465797007));
#23948=CARTESIAN_POINT('',(0.00377734383156351,0.0126817441254899,-0.00651558261687086));
#23949=CARTESIAN_POINT('',(0.00193589001437694,0.0128150846611219,-0.00727828771239866));
#23950=CARTESIAN_POINT('',(0.0009377494958536,0.0128782206633705,-0.00747273484902566));
#23951=CARTESIAN_POINT('',(-0.00105534502579677,0.0129974241367329,-0.00745703644629026));
#23952=CARTESIAN_POINT('',(-0.0020502990289238,0.0130534916078467,-0.00724689090692786));
#23953=CARTESIAN_POINT('',(-0.00387950950825059,0.0131585580189395,-0.0064552720738411));
#23954=CARTESIAN_POINT('',(-0.00471376598445036,0.0132075569589185,-0.00587379878011675));
#23955=CARTESIAN_POINT('',(-0.00608951663137417,0.0132984863077418,-0.00443158740195935));
#23956=CARTESIAN_POINT('',(-0.00663101080209822,0.013340416716586,-0.0035708493175263));
#23957=CARTESIAN_POINT('',(-0.00733549472922503,0.0134172090031397,-0.00170633012632612));
#23958=CARTESIAN_POINT('',(-0.0074984844856278,0.0134520708808492,-0.000702549019558996));
#23959=CARTESIAN_POINT('',(-0.00742022781179112,0.0135147261051333,0.00128899852799355));
#23960=CARTESIAN_POINT('',(-0.00717898138155166,0.0135425194517079,0.00227676496877898));
#23961=CARTESIAN_POINT('',(-0.00675458025798432,0.0135667785327152,0.00317861926757889));
#23962=CARTESIAN_POINT('',(-0.00696003595717303,0.00948593263374612,0.00226168702627111));
#23963=CARTESIAN_POINT('',(-0.00665806128380176,0.00962328821290979,0.00319097324510079));
#23964=CARTESIAN_POINT('',(-0.00616754750743291,0.00975710952650608,0.00405873365389791));
#23965=CARTESIAN_POINT('',(-0.00488690599684642,0.0100176836225639,0.00553440830489247));
#23966=CARTESIAN_POINT('',(-0.00409677826262877,0.0101444364050254,0.00614232254708991));
#23967=CARTESIAN_POINT('',(-0.00234204318889632,0.0103908734388137,0.00700191167309798));
#23968=CARTESIAN_POINT('',(-0.00137743584938151,0.0105105576901405,0.00725358655690861));
#23969=CARTESIAN_POINT('',(0.000573566435869221,0.0107428576616592,0.00736089629010987));
#23970=CARTESIAN_POINT('',(0.00155996138160514,0.0108554733818512,0.0072165311395005));
#23971=CARTESIAN_POINT('',(0.00339838058141192,0.0110736362911005,0.006554603886254));
#23972=CARTESIAN_POINT('',(0.00425040483548277,0.0111791834801577,0.00603704178361687));
#23973=CARTESIAN_POINT('',(0.00568520096441194,0.0113832093271374,0.00471065807769657));
#23974=CARTESIAN_POINT('',(0.00626797283927026,0.0114816879850599,0.0039018364744134));
#23975=CARTESIAN_POINT('',(0.00707200622525638,0.01167157676977,0.00212097628025275));
#23976=CARTESIAN_POINT('',(0.00729326773638417,0.0117629868965577,0.00114893768937527));
#23977=CARTESIAN_POINT('',(0.00733925289099655,0.0119387386189984,-0.000804474325494489));
#23978=CARTESIAN_POINT('',(0.00716397653448113,0.0120230802146513,-0.00178584774948676));
#23979=CARTESIAN_POINT('',(0.0064446336742028,0.0121846948748224,-0.00360256974620541));
#23980=CARTESIAN_POINT('',(0.00590056717043989,0.0122619679393405,-0.00443791831893177));
#23981=CARTESIAN_POINT('',(0.00452977433180828,0.012409445537242,-0.00583034789627018));
#23982=CARTESIAN_POINT('',(0.00370304799693959,0.0124796500706254,-0.00638742890088223));
#23983=CARTESIAN_POINT('',(0.00189781337354895,0.0126129906062573,-0.00713513249954584));
#23984=CARTESIAN_POINT('',(0.000919305085027019,0.0126761266085059,-0.00732575509359739));
#23985=CARTESIAN_POINT('',(-0.0010345876515666,0.0127953300818683,-0.00731036545966501));
#23986=CARTESIAN_POINT('',(-0.00200997209963829,0.0128513975529821,-0.00710435323168109));
#23987=CARTESIAN_POINT('',(-0.00380320419697909,0.012956463964075,-0.00632830459408905));
#23988=CARTESIAN_POINT('',(-0.00462105184624821,0.013005462904054,-0.00575826818448094));
#23989=CARTESIAN_POINT('',(-0.00596974312365063,0.0130963922528773,-0.00434442337892649));
#23990=CARTESIAN_POINT('',(-0.00650058675178394,0.0131383226617215,-0.00350061498298014));
#23991=CARTESIAN_POINT('',(-0.00719121432278355,0.0132151149482752,-0.00167276865389143));
#23992=CARTESIAN_POINT('',(-0.00735099826564986,0.0132499768259846,-0.000688730720749077));
#23993=CARTESIAN_POINT('',(-0.00727428080697516,0.0133126320502687,0.0012636454688767));
#23994=CARTESIAN_POINT('',(-0.00703777940543416,0.0133404253968434,0.00223198372536013));
#23995=CARTESIAN_POINT('',(-0.00662172574428931,0.0133646844778507,0.00311609962892087));
#23996=CARTESIAN_POINT('',(-0.0068589899293032,0.00940873957371216,0.00222885178063507));
#23997=CARTESIAN_POINT('',(-0.00656139933403859,0.00954609515287583,0.00314464659198573));
#23998=CARTESIAN_POINT('',(-0.00607800685259157,0.00967991646647212,0.0039998088270103));
#23999=CARTESIAN_POINT('',(-0.00481595773701083,0.00994049056252993,0.0054540595855381));
#24000=CARTESIAN_POINT('',(-0.00403730110287711,0.0100672433449915,0.00605314810904134));
#24001=CARTESIAN_POINT('',(-0.00230804132988384,0.0103136803787797,0.00690025769222555));
#24002=CARTESIAN_POINT('',(-0.00135743819102429,0.0104333646301065,0.00714827875190651));
#24003=CARTESIAN_POINT('',(0.000565239379741828,0.0106656646016253,0.0072540305589191));
#24004=CARTESIAN_POINT('',(0.00153731381164839,0.0107782803218173,0.00711176130625072));
#24005=CARTESIAN_POINT('',(0.00334904278185819,0.0109964432310665,0.00645944393434548));
#24006=CARTESIAN_POINT('',(0.00418869732016143,0.0111019904201238,0.00594939581510862));
#24007=CARTESIAN_POINT('',(0.00560266303233365,0.0113060162671035,0.0046422685908702));
#24008=CARTESIAN_POINT('',(0.00617697420620263,0.0114044949250259,0.00384518948586864));
#24009=CARTESIAN_POINT('',(0.00696933460940123,0.0115943837097361,0.00209018387779328));
#24010=CARTESIAN_POINT('',(0.00718738383873084,0.0116857938365238,0.00113225737471947));
#24011=CARTESIAN_POINT('',(0.0072327013793764,0.0118615455589644,-0.000792794941132875));
#24012=CARTESIAN_POINT('',(0.00705996969069235,0.0119458871546173,-0.00175992075391141));
#24013=CARTESIAN_POINT('',(0.00635107027340123,0.0121075018147884,-0.00355026752173156));
#24014=CARTESIAN_POINT('',(0.00581490254479415,0.0121847748793065,-0.00437348847677317));
#24015=CARTESIAN_POINT('',(0.00446401092107414,0.0123322524772081,-0.00574570271632536));
#24016=CARTESIAN_POINT('',(0.00364928702596121,0.0124024570105914,-0.00629469600083595));
#24017=CARTESIAN_POINT('',(0.00187026085741034,0.0125357975462234,-0.0070315444143922));
#24018=CARTESIAN_POINT('',(0.000905958583972412,0.012598933548472,-0.00721939954343787));
#24019=CARTESIAN_POINT('',(-0.00101956747447022,0.0127181370218344,-0.00720423333671029));
#24020=CARTESIAN_POINT('',(-0.00198079125947491,0.0127742044929482,-0.00700121200093706));
#24021=CARTESIAN_POINT('',(-0.0037479891550386,0.012879270904041,-0.00623643006264729));
#24022=CARTESIAN_POINT('',(-0.0045539632655976,0.01292826984402,-0.00567466946013077));
#24023=CARTESIAN_POINT('',(-0.00588307419927152,0.0130191991928433,-0.00428135089934067));
#24024=CARTESIAN_POINT('',(-0.00640621102238644,0.0130611296016875,-0.0034497929410671));
#24025=CARTESIAN_POINT('',(-0.00708681203990037,0.0131379218882412,-0.0016484833442952));
#24026=CARTESIAN_POINT('',(-0.00724427623429937,0.0131727837659507,-0.000678731705796877));
#24027=CARTESIAN_POINT('',(-0.00716867256217909,0.0132354389902348,0.00124529982295599));
#24028=CARTESIAN_POINT('',(-0.0069356046956598,0.0132632323368094,0.00219957971321054));
#24029=CARTESIAN_POINT('',(-0.00652559131506782,0.0132874914178167,0.00307085999339506));
#24030=CARTESIAN_POINT('',(-0.00663304414212992,0.0093315465136782,0.00215542993933499));
#24031=CARTESIAN_POINT('',(-0.00634525664353049,0.00946890209284187,0.00304105704645039));
#24032=CARTESIAN_POINT('',(-0.00587778786161648,0.00960272340643816,0.00386804890852719));
#24033=CARTESIAN_POINT('',(-0.00465731260513313,0.00986329750249597,0.00527439438715669));
#24034=CARTESIAN_POINT('',(-0.00390430613056378,0.0099900502849575,0.0058537480037094));
#24035=CARTESIAN_POINT('',(-0.00223201086177059,0.0102364873187458,0.00667295248081131));
#24036=CARTESIAN_POINT('',(-0.00131272206754674,0.0103561715700725,0.00691280334136051));
#24037=CARTESIAN_POINT('',(0.000546619516188517,0.0105884715415913,0.00701507151951131));
#24038=CARTESIAN_POINT('',(0.00148667230569993,0.0107010872617833,0.00687748883711291));
#24039=CARTESIAN_POINT('',(0.00323872010819583,0.0109192501710326,0.00624665981314244));
#24040=CARTESIAN_POINT('',(0.00405071512118033,0.0110247973600898,0.00575341347157038));
#24041=CARTESIAN_POINT('',(0.00541810260548434,0.0112288232070695,0.00448934504938012));
#24042=CARTESIAN_POINT('',(0.00597349507680387,0.011327301864992,0.00371852296876192));
#24043=CARTESIAN_POINT('',(0.00673975389698938,0.0115171906497021,0.00202132997270337));
#24044=CARTESIAN_POINT('',(0.00695062024585536,0.0116086007764898,0.00109495905726303));
#24045=CARTESIAN_POINT('',(0.0069944449562884,0.0117843524989304,-0.000766679043764952));
#24046=CARTESIAN_POINT('',(0.00682740331785544,0.0118686940945834,-0.00170194622935258));
#24047=CARTESIAN_POINT('',(0.00614185614900286,0.0120303087547544,-0.00343331619243359));
#24048=CARTESIAN_POINT('',(0.00562335061858323,0.0121075818192726,-0.00422941896992696));
#24049=CARTESIAN_POINT('',(0.00431695946424038,0.0122550594171741,-0.00555643034000104));
#24050=CARTESIAN_POINT('',(0.00352907384031716,0.0123252639505575,-0.00608733893258175));
#24051=CARTESIAN_POINT('',(0.00180865155837324,0.0124586044861894,-0.00679991441432962));
#24052=CARTESIAN_POINT('',(0.000876114900352539,0.012521740488438,-0.00698158130349679));
#24053=CARTESIAN_POINT('',(-0.0009859813374486,0.0126409439618004,-0.00696691469518718));
#24054=CARTESIAN_POINT('',(-0.00191554091722904,0.0126970114329142,-0.0067705811977104));
#24055=CARTESIAN_POINT('',(-0.00362452456787917,0.0128020778440071,-0.00603099236494257));
#24056=CARTESIAN_POINT('',(-0.00440394863874887,0.0128510767839861,-0.00548773702965151));
#24057=CARTESIAN_POINT('',(-0.00568927659282304,0.0129420061328093,-0.00414031654747732));
#24058=CARTESIAN_POINT('',(-0.00619518047602752,0.0129839365416536,-0.00333615140059418));
#24059=CARTESIAN_POINT('',(-0.00685336143836741,0.0130607288282073,-0.00159417974118338));
#24060=CARTESIAN_POINT('',(-0.00700563851750282,0.0130955907059167,-0.000656373228655722));
#24061=CARTESIAN_POINT('',(-0.00693252534783064,0.0131582459302008,0.00120427771158615));
#24062=CARTESIAN_POINT('',(-0.00670713509902304,0.0131860392767755,0.00212712213930035));
#24063=CARTESIAN_POINT('',(-0.00631062819635045,0.0132102983577827,0.00296970109308201));
#24064=CARTESIAN_POINT('',(-0.00650814438282647,0.0093315465136782,0.00211484334367094));
#24065=CARTESIAN_POINT('',(-0.00622577590278555,0.00946890209284187,0.00298379415403012));
#24066=CARTESIAN_POINT('',(-0.00576710952548273,0.00960272340643816,0.00379521381693169));
#24067=CARTESIAN_POINT('',(-0.00456961573309102,0.00986329750249597,0.00517507790812964));
#24068=CARTESIAN_POINT('',(-0.00383078831800211,0.0099900502849575,0.00574352233642602));
#24069=CARTESIAN_POINT('',(-0.0021899822526698,0.0102364873187458,0.00654730125026951));
#24070=CARTESIAN_POINT('',(-0.00128800360242641,0.0103561715700726,0.00678263573581662));
#24071=CARTESIAN_POINT('',(0.000536326708762601,0.0105884715415913,0.0068829782112943));
#24072=CARTESIAN_POINT('',(0.0014586783697082,0.0107010872617833,0.00674798620122487));
#24073=CARTESIAN_POINT('',(0.00317773523408718,0.0109192501710326,0.00612903564384791));
#24074=CARTESIAN_POINT('',(0.00397444043752055,0.0110247973600898,0.00564507709654038));
#24075=CARTESIAN_POINT('',(0.00531608011071332,0.0112288232070695,0.00440481099471639));
#24076=CARTESIAN_POINT('',(0.00586101458047273,0.011327301864992,0.00364850344019995));
#24077=CARTESIAN_POINT('',(0.00661284480043267,0.0115171906497021,0.00198326847007294));
#24078=CARTESIAN_POINT('',(0.00681974055063321,0.0116086007764898,0.00107434105446238));
#24079=CARTESIAN_POINT('',(0.00686274004482053,0.0117843524989304,-0.000752242530758643));
#24080=CARTESIAN_POINT('',(0.00669884378880731,0.0118686940945834,-0.00166989870036911));
#24081=CARTESIAN_POINT('',(0.00602620542540606,0.0120303087547544,-0.00336866708760947));
#24082=CARTESIAN_POINT('',(0.00551746331801803,0.0121075818192726,-0.00414977930523935));
#24083=CARTESIAN_POINT('',(0.00423567141814074,0.0122550594171741,-0.00545180314362154));
#24084=CARTESIAN_POINT('',(0.00346262162565148,0.0123252639505575,-0.00597271476437384));
#24085=CARTESIAN_POINT('',(0.00177459477547475,0.0124586044861894,-0.00667187249942069));
#24086=CARTESIAN_POINT('',(0.000859617717787273,0.012521740488438,-0.00685011861371523));
#24087=CARTESIAN_POINT('',(-0.000967415377523374,0.0126409439618004,-0.00683572817661878));
#24088=CARTESIAN_POINT('',(-0.00187947141514655,0.0126970114329142,-0.00664309162522779));
#24089=CARTESIAN_POINT('',(-0.00355627502266023,0.0128020778440071,-0.00591742919867961));
#24090=CARTESIAN_POINT('',(-0.00432102259255074,0.0128510767839861,-0.00538440332352243));
#24091=CARTESIAN_POINT('',(-0.00558214791075367,0.0129420061328093,-0.00406235467519978));
#24092=CARTESIAN_POINT('',(-0.00607852565906608,0.0129839365416536,-0.00327333190203431));
#24093=CARTESIAN_POINT('',(-0.00672431311971763,0.0130607288282073,-0.00156416144766781));
#24094=CARTESIAN_POINT('',(-0.00687372283205676,0.0130955907059167,-0.000644013766466766));
#24095=CARTESIAN_POINT('',(-0.00680198637827826,0.0131582459302008,0.00118160124613701));
#24096=CARTESIAN_POINT('',(-0.00658084021216063,0.0131860392767755,0.00208706857753974));
#24097=CARTESIAN_POINT('',(-0.00619179950685455,0.0132102983577827,0.00291378182829478));
#24098=CARTESIAN_POINT('',(-0.0062821985956532,0.00940873957371216,0.00204142150237086));
#24099=CARTESIAN_POINT('',(-0.00600963321227745,0.00954609515287583,0.00288020460849478));
#24100=CARTESIAN_POINT('',(-0.00556689053450765,0.00967991646647212,0.00366345389844858));
#24101=CARTESIAN_POINT('',(-0.00441097060121332,0.00994049056252993,0.00499541270974823));
#24102=CARTESIAN_POINT('',(-0.00369779334568878,0.0100672433449915,0.00554412223109408));
#24103=CARTESIAN_POINT('',(-0.00211395178455655,0.0103136803787797,0.00631999603885527));
#24104=CARTESIAN_POINT('',(-0.00124328747894885,0.0104333646301065,0.00654716032527062));
#24105=CARTESIAN_POINT('',(0.000517706845209291,0.0106656646016253,0.00664401917188651));
#24106=CARTESIAN_POINT('',(0.00140803686375974,0.0107782803218173,0.00651371373208705));
#24107=CARTESIAN_POINT('',(0.00306741256042481,0.0109964432310665,0.00591625152264486));
#24108=CARTESIAN_POINT('',(0.00383645823853945,0.0111019904201238,0.00544909475300212));
#24109=CARTESIAN_POINT('',(0.00513151968386402,0.0113060162671035,0.0042518874532263));
#24110=CARTESIAN_POINT('',(0.00565753545107397,0.0114044949250259,0.00352183692309322));
#24111=CARTESIAN_POINT('',(0.00638326408802082,0.0115943837097361,0.00191441456498304));
#24112=CARTESIAN_POINT('',(0.00658297695775774,0.0116857938365238,0.00103704273700594));
#24113=CARTESIAN_POINT('',(0.00662448362173252,0.0118615455589644,-0.000726126633390719));
#24114=CARTESIAN_POINT('',(0.00646627741597039,0.0119458871546173,-0.00161192417581028));
#24115=CARTESIAN_POINT('',(0.00581699130100768,0.0121075018147884,-0.0032517157583115));
#24116=CARTESIAN_POINT('',(0.0053259113918071,0.0121847748793065,-0.00400570979839314));
#24117=CARTESIAN_POINT('',(0.00408861996130697,0.0123322524772081,-0.00526253076729722));
#24118=CARTESIAN_POINT('',(0.00334240844000743,0.0124024570105914,-0.00576535769611964));
#24119=CARTESIAN_POINT('',(0.00171298547643764,0.0125357975462234,-0.00644024249935811));
#24120=CARTESIAN_POINT('',(0.000829774034167402,0.012598933548472,-0.00661230037377415));
#24121=CARTESIAN_POINT('',(-0.000933829240501756,0.0127181370218344,-0.00659840953509566));
#24122=CARTESIAN_POINT('',(-0.00181422107290067,0.0127742044929482,-0.00641246082200114));
#24123=CARTESIAN_POINT('',(-0.0034328104355008,0.012879270904041,-0.00571199150097489));
#24124=CARTESIAN_POINT('',(-0.004171007965702,0.01292826984402,-0.00519747089304317));
#24125=CARTESIAN_POINT('',(-0.00538835030430518,0.0130191991928433,-0.00392132032333643));
#24126=CARTESIAN_POINT('',(-0.00586749511270716,0.0130611296016875,-0.0031596903615614));
#24127=CARTESIAN_POINT('',(-0.00649086251818467,0.0131379218882412,-0.00150985784455599));
#24128=CARTESIAN_POINT('',(-0.00663508511526021,0.0131727837659507,-0.000621655289325611));
#24129=CARTESIAN_POINT('',(-0.00656583916392981,0.0132354389902348,0.00114057913476716));
#24130=CARTESIAN_POINT('',(-0.00635237061552386,0.0132632323368094,0.00201461100362955));
#24131=CARTESIAN_POINT('',(-0.00597683638813717,0.0132874914178167,0.00281262292798174));
#24132=CARTESIAN_POINT('',(-0.00618115256778337,0.00948593263374612,0.00200858625673482));
#24133=CARTESIAN_POINT('',(-0.00591297126251429,0.00962328821290979,0.00283387795537971));
#24134=CARTESIAN_POINT('',(-0.0054773498796663,0.00975710952650608,0.00360452907156096));
#24135=CARTESIAN_POINT('',(-0.00434002234137772,0.0100176836225639,0.00491506399039386));
#24136=CARTESIAN_POINT('',(-0.00363831618593712,0.0101444364050254,0.00545494779304551));
#24137=CARTESIAN_POINT('',(-0.00207994992554408,0.0103908734388137,0.00621834205798284));
#24138=CARTESIAN_POINT('',(-0.00122328982059163,0.0105105576901405,0.00644185252026851));
#24139=CARTESIAN_POINT('',(0.000509379789081899,0.0107428576616592,0.00653715344069573));
#24140=CARTESIAN_POINT('',(0.00138538929380299,0.0108554733818512,0.00640894389883727));
#24141=CARTESIAN_POINT('',(0.0030180747608711,0.0110736362911005,0.00582109157073635));
#24142=CARTESIAN_POINT('',(0.00377475072321812,0.0111791834801577,0.00536144878449388));
#24143=CARTESIAN_POINT('',(0.00504898175178574,0.0113832093271374,0.00418349796639994));
#24144=CARTESIAN_POINT('',(0.00556653681800634,0.0114816879850599,0.00346518993454846));
#24145=CARTESIAN_POINT('',(0.00628059247216568,0.01167157676977,0.00188362216252356));
#24146=CARTESIAN_POINT('',(0.00647709306010441,0.0117629868965577,0.00102036242235014));
#24147=CARTESIAN_POINT('',(0.00651793211011238,0.0119387386189984,-0.000714447249029104));
#24148=CARTESIAN_POINT('',(0.00636227057218162,0.0120230802146513,-0.00158599718023493));
#24149=CARTESIAN_POINT('',(0.00572342790020611,0.0121846948748224,-0.00319941353383765));
#24150=CARTESIAN_POINT('',(0.00524024676616137,0.0122619679393405,-0.00394127995623455));
#24151=CARTESIAN_POINT('',(0.00402285655057284,0.012409445537242,-0.0051778855873524));
#24152=CARTESIAN_POINT('',(0.00328864746902905,0.0124796500706254,-0.00567262479607335));
#24153=CARTESIAN_POINT('',(0.00168543296029903,0.0126129906062574,-0.00633665441420447));
#24154=CARTESIAN_POINT('',(0.000816427533112798,0.0126761266085059,-0.00650594482361463));
#24155=CARTESIAN_POINT('',(-0.000918809063405365,0.0127953300818683,-0.00649227741214095));
#24156=CARTESIAN_POINT('',(-0.0017850402327373,0.0128513975529821,-0.0063093195912571));
#24157=CARTESIAN_POINT('',(-0.00337759539356031,0.012956463964075,-0.00562011696953312));
#24158=CARTESIAN_POINT('',(-0.0041039193850514,0.013005462904054,-0.005113872168693));
#24159=CARTESIAN_POINT('',(-0.00530168137992607,0.0130963922528773,-0.00385824784375061));
#24160=CARTESIAN_POINT('',(-0.00577311938330966,0.0131383226617215,-0.00310886831964835));
#24161=CARTESIAN_POINT('',(-0.00638646023530149,0.0132151149482752,-0.00148557253495975));
#24162=CARTESIAN_POINT('',(-0.00652836308390973,0.0132499768259846,-0.000611656274373411));
#24163=CARTESIAN_POINT('',(-0.00646023091913374,0.0133126320502687,0.00112223348884645));
#24164=CARTESIAN_POINT('',(-0.00625019590574951,0.0133404253968434,0.00198220699147998));
#24165=CARTESIAN_POINT('',(-0.00588070195891569,0.0133646844778507,0.00276738329245591));
#24166=CARTESIAN_POINT('',(-0.00604151039169543,0.00968802668861064,0.00196320906329477));
#24167=CARTESIAN_POINT('',(-0.00577938773336043,0.00982538226777431,0.00276985609535972));
#24168=CARTESIAN_POINT('',(-0.00535360773805049,0.0099592035813706,0.00352309696358349));
#24169=CARTESIAN_POINT('',(-0.00424197425772759,0.0102197776774284,0.00480402479119866));
#24170=CARTESIAN_POINT('',(-0.00355612077271463,0.0103465304598899,0.00533171175059006));
#24171=CARTESIAN_POINT('',(-0.00203296051206952,0.0105929674936782,0.00607785971150886));
#24172=CARTESIAN_POINT('',(-0.00119565373643737,0.010712651745005,0.00629632071303625));
#24173=CARTESIAN_POINT('',(0.000497872080540071,0.0109449517165238,0.0063894686324227));
#24174=CARTESIAN_POINT('',(0.00135409112188536,0.0110575674367158,0.00626415555028175));
#24175=CARTESIAN_POINT('',(0.00294989159881799,0.011275730345965,0.00568958375156659));
#24176=CARTESIAN_POINT('',(0.00368947303440534,0.0113812775350222,0.00524032503499238));
#24177=CARTESIAN_POINT('',(0.00493491713501468,0.0115853033820019,0.00408898602007905));
#24178=CARTESIAN_POINT('',(0.00544077980003666,0.0116837820399244,0.00338690572173993));
#24179=CARTESIAN_POINT('',(0.00613870378873374,0.0118736708246346,0.00184106810891984));
#24180=CARTESIAN_POINT('',(0.00633076511240882,0.0119650809514223,0.000997310794438875));
#24181=CARTESIAN_POINT('',(0.00637068154260601,0.0121408326738629,-0.000698306736809027));
#24182=CARTESIAN_POINT('',(0.00621853664912812,0.0122251742695158,-0.00155016695357596));
#24183=CARTESIAN_POINT('',(0.00559412646040137,0.0123867889296869,-0.00312713363730202));
#24184=CARTESIAN_POINT('',(0.0051218611651525,0.012464061994205,-0.00385224010426115));
#24185=CARTESIAN_POINT('',(0.00393197375215438,0.0126115395921065,-0.00506090882565251));
#24186=CARTESIAN_POINT('',(0.00321435163440513,0.0126817441254899,-0.00554447108008473));
#24187=CARTESIAN_POINT('',(0.00164735631947105,0.0128150846611219,-0.00619349920135166));
#24188=CARTESIAN_POINT('',(0.000797983122286219,0.0128782206633705,-0.00635896506818636));
#24189=CARTESIAN_POINT('',(-0.000898051689175195,0.0129974241367329,-0.0063456064255157));
#24190=CARTESIAN_POINT('',(-0.00174471330345178,0.0130534916078467,-0.00616678191601033));
#24191=CARTESIAN_POINT('',(-0.0033012900822888,0.0131585580189395,-0.00549314948978108));
#24192=CARTESIAN_POINT('',(-0.00401120524684925,0.0132075569589185,-0.00499834157305719));
#24193=CARTESIAN_POINT('',(-0.00518190787220253,0.0132984863077418,-0.00377108382071775));
#24194=CARTESIAN_POINT('',(-0.00564269533299538,0.013340416716586,-0.0030386339851022));
#24195=CARTESIAN_POINT('',(-0.00624217982886001,0.0134172090031397,-0.00145201106252507));
#24196=CARTESIAN_POINT('',(-0.00638087686393179,0.0134520708808492,-0.000597837975563491));
#24197=CARTESIAN_POINT('',(-0.00631428391431779,0.0135147261051333,0.0010968804297296));
#24198=CARTESIAN_POINT('',(-0.00610899392963201,0.0135425194517079,0.00193742574806112));
#24199=CARTESIAN_POINT('',(-0.00574784744522067,0.0135667785327152,0.00270486365379789));
#24200=CARTESIAN_POINT('',(-0.00600291424347733,0.0098129276834412,0.00195066711549076));
#24201=CARTESIAN_POINT('',(-0.00574246615396974,0.00995028326260487,0.00275216088845479));
#24202=CARTESIAN_POINT('',(-0.00531940625127602,0.0100841045762011,0.00350058968249363));
#24203=CARTESIAN_POINT('',(-0.00421487443391305,0.010344678672259,0.00477333431135782));
#24204=CARTESIAN_POINT('',(-0.0035334025192438,0.0104714314547205,0.00529765014618318));
#24205=CARTESIAN_POINT('',(-0.00201997295760744,0.0107178684885088,0.00603903134590732));
#24206=CARTESIAN_POINT('',(-0.00118801531064032,0.0108375527398356,0.0062560967108061));
#24207=CARTESIAN_POINT('',(0.000494691428125636,0.0110698527113543,0.00634864955534044));
#24208=CARTESIAN_POINT('',(0.00134544051992447,0.0111824684315463,0.006224137034976));
#24209=CARTESIAN_POINT('',(0.00293104623631861,0.0114006313407956,0.00565323588430534));
#24210=CARTESIAN_POINT('',(0.0036659028609139,0.0115061785298528,0.00520684725399912));
#24211=CARTESIAN_POINT('',(0.0049033904503219,0.0117102043768325,0.00406286356058453));
#24212=CARTESIAN_POINT('',(0.00540602141513461,0.011808683034755,0.00336526849747616));
#24213=CARTESIAN_POINT('',(0.00609948672115694,0.0119985718194651,0.0018293064577756));
#24214=CARTESIAN_POINT('',(0.00629032106236656,0.0120899819462528,0.000990939481183402));
#24215=CARTESIAN_POINT('',(0.0063299824867198,0.0122657336686934,-0.000693845608950565));
#24216=CARTESIAN_POINT('',(0.00617880956986341,0.0123500752643464,-0.00154026372249235));
#24217=CARTESIAN_POINT('',(0.0055583884213982,0.0125116899245174,-0.00310715596524024));
#24218=CARTESIAN_POINT('',(0.00508914018978937,0.0125889629890356,-0.00382763009444636));
#24219=CARTESIAN_POINT('',(0.00390685436447006,0.0127364405869371,-0.00502857724389744));
#24220=CARTESIAN_POINT('',(0.00319381677075958,0.0128066451203205,-0.0055090502641424));
#24221=CARTESIAN_POINT('',(0.00163683219478167,0.0129399856559524,-0.00615393207365249));
#24222=CARTESIAN_POINT('',(0.000792885212514245,0.013003121658201,-0.00631834086291762));
#24223=CARTESIAN_POINT('',(-0.000892314492041416,0.0131223251315634,-0.00630506756184518));
#24224=CARTESIAN_POINT('',(-0.00173356721432965,0.0131783926026772,-0.00612738547150761));
#24225=CARTESIAN_POINT('',(-0.00328019981295779,0.0132834590137701,-0.0054580565414708));
#24226=CARTESIAN_POINT('',(-0.00398557968929771,0.0133324579537491,-0.00496640970177156));
#24227=CARTESIAN_POINT('',(-0.00514880328885811,0.0134233873025723,-0.0037469922772707));
#24228=CARTESIAN_POINT('',(-0.0056066470120786,0.0134653177114166,-0.00301922169246908));
#24229=CARTESIAN_POINT('',(-0.00620230170530171,0.0135421099979703,-0.00144273489968662));
#24230=CARTESIAN_POINT('',(-0.00634011267530433,0.0135769718756797,-0.000594018691705771));
#24231=CARTESIAN_POINT('',(-0.00627394515429791,0.0136396270999638,0.00108987301653346));
#24232=CARTESIAN_POINT('',(-0.00606996666328886,0.0136674204465385,0.00192504851679185));
#24233=CARTESIAN_POINT('',(-0.00571112736074713,0.0136916795275457,0.00268758365066568));
#24234=CARTESIAN_POINT('',(-0.00600291424347733,0.0099532476683191,0.00195066711549077));
#24235=CARTESIAN_POINT('',(-0.00574246615396974,0.0100906032474828,0.00275216088845479));
#24236=CARTESIAN_POINT('',(-0.00531940625127602,0.010224424561079,0.00350058968249362));
#24237=CARTESIAN_POINT('',(-0.00421487443391306,0.0104849986571369,0.00477333431135782));
#24238=CARTESIAN_POINT('',(-0.0035334025192438,0.0106117514395984,0.00529765014618318));
#24239=CARTESIAN_POINT('',(-0.00201997295760744,0.0108581884733867,0.00603903134590732));
#24240=CARTESIAN_POINT('',(-0.00118801531064032,0.0109778727247135,0.00625609671080609));
#24241=CARTESIAN_POINT('',(0.000494691428125636,0.0112101726962322,0.00634864955534043));
#24242=CARTESIAN_POINT('',(0.00134544051992447,0.0113227884164242,0.00622413703497599));
#24243=CARTESIAN_POINT('',(0.0029310462363186,0.0115409513256735,0.00565323588430534));
#24244=CARTESIAN_POINT('',(0.0036659028609139,0.0116464985147307,0.00520684725399913));
#24245=CARTESIAN_POINT('',(0.0049033904503219,0.0118505243617104,0.00406286356058454));
#24246=CARTESIAN_POINT('',(0.00540602141513462,0.0119490030196329,0.00336526849747616));
#24247=CARTESIAN_POINT('',(0.00609948672115694,0.012138891804343,0.00182930645777559));
#24248=CARTESIAN_POINT('',(0.00629032106236656,0.0122303019311307,0.000990939481183403));
#24249=CARTESIAN_POINT('',(0.0063299824867198,0.0124060536535713,-0.000693845608950565));
#24250=CARTESIAN_POINT('',(0.00617880956986341,0.0124903952492243,-0.00154026372249235));
#24251=CARTESIAN_POINT('',(0.0055583884213982,0.0126520099093953,-0.00310715596524024));
#24252=CARTESIAN_POINT('',(0.00508914018978937,0.0127292829739135,-0.00382763009444637));
#24253=CARTESIAN_POINT('',(0.00390685436447006,0.012876760571815,-0.00502857724389744));
#24254=CARTESIAN_POINT('',(0.00319381677075958,0.0129469651051984,-0.00550905026414239));
#24255=CARTESIAN_POINT('',(0.00163683219478167,0.0130803056408303,-0.00615393207365248));
#24256=CARTESIAN_POINT('',(0.000792885212514244,0.0131434416430789,-0.00631834086291762));
#24257=CARTESIAN_POINT('',(-0.000892314492041418,0.0132626451164413,-0.00630506756184519));
#24258=CARTESIAN_POINT('',(-0.00173356721432965,0.0133187125875551,-0.00612738547150761));
#24259=CARTESIAN_POINT('',(-0.00328019981295779,0.013423778998648,-0.0054580565414708));
#24260=CARTESIAN_POINT('',(-0.0039855796892977,0.013472777938627,-0.00496640970177156));
#24261=CARTESIAN_POINT('',(-0.00514880328885811,0.0135637072874503,-0.0037469922772707));
#24262=CARTESIAN_POINT('',(-0.0056066470120786,0.0136056376962945,-0.00301922169246908));
#24263=CARTESIAN_POINT('',(-0.00620230170530171,0.0136824299828482,-0.00144273489968662));
#24264=CARTESIAN_POINT('',(-0.00634011267530433,0.0137172918605576,-0.000594018691705768));
#24265=CARTESIAN_POINT('',(-0.00627394515429791,0.0137799470848417,0.00108987301653346));
#24266=CARTESIAN_POINT('',(-0.00606996666328886,0.0138077404314164,0.00192504851679185));
#24267=CARTESIAN_POINT('',(-0.00571112736074713,0.0138319995124236,0.00268758365066568));
#24268=CARTESIAN_POINT('',(-0.00600350244213179,0.00996866665836644,0.00195085825261618));
#24269=CARTESIAN_POINT('',(-0.00574302883248355,0.0101060222375301,0.00275243056036177));
#24270=CARTESIAN_POINT('',(-0.00531992747604663,0.0102398435511264,0.00350093268958277));
#24271=CARTESIAN_POINT('',(-0.00421528743056271,0.0105004176471842,0.00477380202898718));
#24272=CARTESIAN_POINT('',(-0.00353374874151571,0.0106271704296457,0.00529816923917059));
#24273=CARTESIAN_POINT('',(-0.00202017088570161,0.010873607463434,0.00603962308351473));
#24274=CARTESIAN_POINT('',(-0.0011881317189345,0.0109932917147608,0.00625670971767546));
#24275=CARTESIAN_POINT('',(0.000494739900720878,0.0112255916862796,0.0063492716310481));
#24276=CARTESIAN_POINT('',(0.00134557235360914,0.0113382074064716,0.00622474691026));
#24277=CARTESIAN_POINT('',(0.00293133343639884,0.0115563703157208,0.00565378981954506));
#24278=CARTESIAN_POINT('',(0.00366626206630027,0.011661917504778,0.00520735744961822));
#24279=CARTESIAN_POINT('',(0.00490387091156926,0.0118659433517577,0.00406326166237022));
#24280=CARTESIAN_POINT('',(0.00540655112693682,0.0119644220096802,0.00336559824504906));
#24281=CARTESIAN_POINT('',(0.00610008438251554,0.0121543107943904,0.00182948570331425));
#24282=CARTESIAN_POINT('',(0.00629093742272671,0.0122457209211781,0.000991036578900586));
#24283=CARTESIAN_POINT('',(0.0063306027333251,0.0124214726436187,-0.000693913595771138));
#24284=CARTESIAN_POINT('',(0.00617941500371233,0.0125058142392716,-0.0015404146460292));
#24285=CARTESIAN_POINT('',(0.00555893306296025,0.0126674288994427,-0.00310746042152328));
#24286=CARTESIAN_POINT('',(0.00508963885182094,0.0127447019639608,-0.0038280051467593));
#24287=CARTESIAN_POINT('',(0.00390723717961403,0.0128921795618623,-0.00502906997163746));
#24288=CARTESIAN_POINT('',(0.00319412971854643,0.0129623840952457,-0.00550959007127961));
#24289=CARTESIAN_POINT('',(0.00163699258063019,0.0130957246308777,-0.00615453506986708));
#24290=CARTESIAN_POINT('',(0.000792962903781556,0.0131588606331263,-0.0063189599688124));
#24291=CARTESIAN_POINT('',(-0.00089240192593807,0.0132780641064887,-0.0063056853671487));
#24292=CARTESIAN_POINT('',(-0.00173373707880906,0.0133341315776025,-0.00612798586653968));
#24293=CARTESIAN_POINT('',(-0.00328052122503168,0.0134391979886953,-0.00545859135196174));
#24294=CARTESIAN_POINT('',(-0.00398597021838331,0.0134881969286743,-0.00496689633799283));
#24295=CARTESIAN_POINT('',(-0.00514930779700927,0.0135791262774976,-0.00374735942824544));
#24296=CARTESIAN_POINT('',(-0.0056071963822836,0.0136210566863418,-0.00301951753246696));
#24297=CARTESIAN_POINT('',(-0.00620290944103967,0.0136978489728955,-0.00144287626681137));
#24298=CARTESIAN_POINT('',(-0.0063407339145214,0.013732710850605,-0.000594076896934264));
#24299=CARTESIAN_POINT('',(-0.00627455991005623,0.0137953660748891,0.00108997980830424));
#24300=CARTESIAN_POINT('',(-0.00607056143210933,0.0138231594214637,0.00192523714366563));
#24301=CARTESIAN_POINT('',(-0.00571168696851309,0.013847418502471,0.00268784699493864));
#24302=CARTESIAN_POINT('',(-0.00600466497160202,0.00998404077070117,0.00195123602046633));
#24303=CARTESIAN_POINT('',(-0.00574414092335559,0.0101213963498648,0.00275296354617664));
#24304=CARTESIAN_POINT('',(-0.00532095763677864,0.0102552176634611,0.00350161061675348));
#24305=CARTESIAN_POINT('',(-0.00421610368672497,0.0105157917595189,0.00477472643696357));
#24306=CARTESIAN_POINT('',(-0.00353443302324826,0.0106425445419805,0.00529919518659681));
#24307=CARTESIAN_POINT('',(-0.00202056207538,0.0108889815757688,0.00604079260745369));
#24308=CARTESIAN_POINT('',(-0.00118836179098845,0.0110086658270955,0.00625792127867733));
#24309=CARTESIAN_POINT('',(0.000494835703082955,0.0112409657986143,0.00635050111591244));
#24310=CARTESIAN_POINT('',(0.00134583291276282,0.0113535815188063,0.00622595228192391));
#24311=CARTESIAN_POINT('',(0.0029319010653021,0.0115717444280555,0.00565488463000731));
#24312=CARTESIAN_POINT('',(0.00366697200816151,0.0116772916171128,0.00520836581207923));
#24313=CARTESIAN_POINT('',(0.00490482050632797,0.0118813174640925,0.00406404847997765));
#24314=CARTESIAN_POINT('',(0.00540759806163502,0.0119797961220149,0.00336624996580416));
#24315=CARTESIAN_POINT('',(0.00610126561429382,0.0121696849067251,0.00182983996835635));
#24316=CARTESIAN_POINT('',(0.00629215561164556,0.0122610950335128,0.000991228485082046));
#24317=CARTESIAN_POINT('',(0.00633182860310908,0.0124368467559534,-0.000694047966501001));
#24318=CARTESIAN_POINT('',(0.00618061159722085,0.0125211883516063,-0.00154071293480974));
#24319=CARTESIAN_POINT('',(0.00556000950518228,0.0126828030117774,-0.00310806215598619));
#24320=CARTESIAN_POINT('',(0.00509062441903194,0.0127600760762956,-0.00382874640885392));
#24321=CARTESIAN_POINT('',(0.00390799378434807,0.0129075536741971,-0.00503004381017692));
#24322=CARTESIAN_POINT('',(0.00319474823581454,0.0129777582075804,-0.0055106569586322));
#24323=CARTESIAN_POINT('',(0.00163730957094308,0.0131110987432124,-0.00615572684557856));
#24324=CARTESIAN_POINT('',(0.000793116454605152,0.013174234745461,-0.00632018358406963));
#24325=CARTESIAN_POINT('',(-0.000892574732320377,0.0132934382188234,-0.00630690641188717));
#24326=CARTESIAN_POINT('',(-0.00173407280290798,0.0133495056899372,-0.00612917250121364));
#24327=CARTESIAN_POINT('',(-0.0032811564713131,0.01345457210103,-0.0054596483638267));
#24328=CARTESIAN_POINT('',(-0.00398674206913061,0.0135035710410091,-0.00496785813711329));
#24329=CARTESIAN_POINT('',(-0.0051503049186267,0.0135945003898323,-0.00374808507395191));
#24330=CARTESIAN_POINT('',(-0.00560828217030528,0.0136364307986766,-0.00302010223750393));
#24331=CARTESIAN_POINT('',(-0.00620411058405509,0.0137132230852302,-0.00144315566807726));
#24332=CARTESIAN_POINT('',(-0.00634196174612631,0.0137480849629397,-0.000594191935098558));
#24333=CARTESIAN_POINT('',(-0.00627577492760283,0.0138107401872238,0.00109019087403817));
#24334=CARTESIAN_POINT('',(-0.00607173694700813,0.0138385335337985,0.0019256099501962));
#24335=CARTESIAN_POINT('',(-0.00571279299028783,0.0138627926148057,0.0026883674746708));
#24336=CARTESIAN_POINT('',(-0.00697849090552825,0.0138048999657612,0.00276297995550743));
#24337=CARTESIAN_POINT('',(-0.00770093960806379,0.0137551587719337,0.000935651043377239));
#24338=CARTESIAN_POINT('',(-0.00763327349501092,0.0136285000940253,-0.00330117175933696));
#24339=CARTESIAN_POINT('',(-0.00306209458664848,0.0133569832064022,-0.00773417999788023));
#24340=CARTESIAN_POINT('',(0.00330337857838533,0.0130039374480187,-0.00763353819154981));
#24341=CARTESIAN_POINT('',(0.00773369503189247,0.0125693628188748,-0.00306198864781927));
#24342=CARTESIAN_POINT('',(0.00763357751275619,0.0120532593189706,0.00330328794520609));
#24343=CARTESIAN_POINT('',(0.00306224339866001,0.0114556269483061,0.00773412121643255));
#24344=CARTESIAN_POINT('',(-0.00330460558482244,0.0107764657068814,0.0076317876877591));
#24345=CARTESIAN_POINT('',(-0.00625423884549511,0.0102693389654248,0.00458959876393758));
#24346=CARTESIAN_POINT('',(-0.00697848972311123,0.0100021874495699,0.00276298343174812));
#24347=CARTESIAN_POINT('',(-0.00697764147125442,0.0100021874312087,0.00276264710354824));
#24348=CARTESIAN_POINT('',(-0.00697848972311123,0.0100021874495699,0.00276298343174812));
#24349=CARTESIAN_POINT('',(-0.00697849262258089,0.00984605923679087,0.00276298464249866));
#24350=CARTESIAN_POINT('',(-0.00685829363455566,0.00953469610649544,0.00271539455481491));
#24351=CARTESIAN_POINT('',(-0.00642351637787649,0.00934096612656149,0.00254325398177964));
#24352=CARTESIAN_POINT('',(-0.00598873928938105,0.00953469656153736,0.00237111344924713));
#24353=CARTESIAN_POINT('',(-0.00586854056022389,0.00984605983716938,0.00232352343153022));
#24354=CARTESIAN_POINT('',(-0.00586854359428379,0.0100021880658147,0.00232352468558586));
#24355=CARTESIAN_POINT('',(-0.00586720616262124,0.0100021880960647,0.00232299439006458));
#24356=CARTESIAN_POINT('',(-0.00586854359418786,0.0100021812334169,0.00232352468554787));
#24357=CARTESIAN_POINT('',(-0.00525948646019975,0.0102693332225451,0.00385961228953058));
#24358=CARTESIAN_POINT('',(-0.00277899942182948,0.0107764609112978,0.00641793334267154));
#24359=CARTESIAN_POINT('',(0.00257518653164471,0.0114556235759148,0.00650399005855098));
#24360=CARTESIAN_POINT('',(0.00641943843133522,0.0120532573720201,0.00277789149481545));
#24361=CARTESIAN_POINT('',(0.00650363171566794,0.0125693622996134,-0.00257497215866852));
#24362=CARTESIAN_POINT('',(0.00277796785160325,0.0130039383586948,-0.00641940530424472));
#24363=CARTESIAN_POINT('',(-0.00257506110685358,0.0133569855492641,-0.00650403960238204));
#24364=CARTESIAN_POINT('',(-0.00641918264818325,0.0136285038713214,-0.00277611217167013));
#24365=CARTESIAN_POINT('',(-0.00647608625583389,0.0137551635070182,0.000786833513742433));
#24366=CARTESIAN_POINT('',(-0.00586854479004135,0.0138049051801146,0.00232352125385291));
#24367=CARTESIAN_POINT('',(0.00629981614599573,7.12593715023016E-5,-0.000371046098527164));
#24368=CARTESIAN_POINT('',(0.00635939064243718,-9.87832735314357E-5,0.000679057046437751));
#24369=CARTESIAN_POINT('',(0.00615655112478957,-0.000268825918565176,0.00174473886966687));
#24370=CARTESIAN_POINT('',(0.0051361018555028,-0.000655582350006689,0.00390539125841257));
#24371=CARTESIAN_POINT('',(0.00416503815747573,-0.000872296136414462,0.00492812037847502));
#24372=CARTESIAN_POINT('',(0.00180511324459718,-0.00130572370923002,0.00619497473129327));
#24373=CARTESIAN_POINT('',(0.000416252029745715,-0.0015224374956378,0.00643909996404906));
#24374=CARTESIAN_POINT('',(-0.00223424743743527,-0.00195586506845336,0.00605333155596514));
#24375=CARTESIAN_POINT('',(-0.00349588568976479,-0.00217257885486115,0.00542343791512543));
#24376=CARTESIAN_POINT('',(-0.00539693087742614,-0.00260600642767672,0.00353668295944536));
#24377=CARTESIAN_POINT('',(-0.00603633781275798,-0.0028227202140845,0.00227982164460499));
#24378=CARTESIAN_POINT('',(-0.00644203138574409,-0.00325614778690008,-0.000367688090038442));
#24379=CARTESIAN_POINT('',(-0.00620831802339835,-0.00347286157330787,-0.0017583365098415));
#24380=CARTESIAN_POINT('',(-0.00495947437447419,-0.00390628914612344,-0.00412777982800341));
#24381=CARTESIAN_POINT('',(-0.00394434408789578,-0.00412300293253122,-0.00510657472636225));
#24382=CARTESIAN_POINT('',(-0.00153097222593843,-0.0045564305053468,-0.00626825994707743));
#24383=CARTESIAN_POINT('',(-0.00013273065055952,-0.00477314429175458,-0.00645115026943376));
#24384=CARTESIAN_POINT('',(0.00249823664508958,-0.00520657186457014,-0.00594926641608398));
#24385=CARTESIAN_POINT('',(0.00373096236535976,-0.00542328565097793,-0.00526449224037788));
#24386=CARTESIAN_POINT('',(0.0055472139220739,-0.00585671322379348,-0.00329596320100655));
#24387=CARTESIAN_POINT('',(0.00613073975851787,-0.00607342701020125,-0.00201220833734133));
#24388=CARTESIAN_POINT('',(0.00641963495622596,-0.00650685458301679,0.000650574354163938));
#24389=CARTESIAN_POINT('',(0.00612500431749009,-0.00672356836942456,0.00202960218200398));
#24390=CARTESIAN_POINT('',(0.00477318663605599,-0.00715699594224009,0.00434184871435166));
#24391=CARTESIAN_POINT('',(0.00371599959335776,-0.00737370972864785,0.00527506741885931));
#24392=CARTESIAN_POINT('',(0.00125389165517365,-0.00780713730146336,0.00632950640194064));
#24393=CARTESIAN_POINT('',(-0.000151029240312234,-0.00802385108787111,0.00645072668051431));
#24394=CARTESIAN_POINT('',(-0.00275741214342121,-0.0084572786606866,0.00583369114460101));
#24395=CARTESIAN_POINT('',(-0.00395887415104431,-0.00867399244709434,0.00509543533011404));
#24396=CARTESIAN_POINT('',(-0.00568671665155151,-0.0091074200199098,0.00304879763889559));
#24397=CARTESIAN_POINT('',(-0.00621309714443561,-0.00932413380631752,0.00174041576216412));
#24398=CARTESIAN_POINT('',(-0.00636649778120604,-0.00971089047793098,-0.000644161934661731));
#24399=CARTESIAN_POINT('',(-0.00616278887993832,-0.00988093336313673,-0.00170967957115776));
#24400=CARTESIAN_POINT('',(-0.00572082786621745,-0.0100509762483425,-0.00266411098250738));
#24401=CARTESIAN_POINT('',(0.00629974209765909,6.75166926736438E-5,-0.00037104173723379));
#24402=CARTESIAN_POINT('',(0.00635931589385908,-0.000102525952360093,0.000679049064769141));
#24403=CARTESIAN_POINT('',(0.00615647876039675,-0.000272568597393834,0.00174471836192376));
#24404=CARTESIAN_POINT('',(0.00513604148551891,-0.000659325028835347,0.00390534535425919));
#24405=CARTESIAN_POINT('',(0.00416498920142043,-0.00087603881524312,0.00492806245311524));
#24406=CARTESIAN_POINT('',(0.00180509202721081,-0.00130946638805867,0.00619490191526757));
#24407=CARTESIAN_POINT('',(0.00041624713709969,-0.00152618017446645,0.00643902427856384));
#24408=CARTESIAN_POINT('',(-0.00223422117598532,-0.00195960774728202,0.00605326040482001));
#24409=CARTESIAN_POINT('',(-0.00349584459895921,-0.00217632153368981,0.00542337416777992));
#24410=CARTESIAN_POINT('',(-0.0053968674416456,-0.00260974910650538,0.00353664138910674));
#24411=CARTESIAN_POINT('',(-0.00603626686135811,-0.00282646289291316,0.00227979484747366));
#24412=CARTESIAN_POINT('',(-0.00644195566580279,-0.00325989046572873,-0.000367683768215259));
#24413=CARTESIAN_POINT('',(-0.00620824505053496,-0.00347660425213652,-0.00175831584227109));
#24414=CARTESIAN_POINT('',(-0.00495941608057806,-0.0039100318249521,-0.00412773130988427));
#24415=CARTESIAN_POINT('',(-0.003944297725889,-0.00412674561135988,-0.00510651470344163));
#24416=CARTESIAN_POINT('',(-0.00153095423081855,-0.00456017318417546,-0.00626818626965384));
#24417=CARTESIAN_POINT('',(-0.000132729090437181,-0.00477688697058323,-0.00645107444230868));
#24418=CARTESIAN_POINT('',(0.00249820728069801,-0.0052103145433988,-0.00594919648812543));
#24419=CARTESIAN_POINT('',(0.00373091851145183,-0.00542702832980658,-0.00526443036128734));
#24420=CARTESIAN_POINT('',(0.00554714871985936,-0.00586045590262214,-0.00329592446009935));
#24421=CARTESIAN_POINT('',(0.00613066769751307,-0.00607716968902991,-0.00201218468574945));
#24422=CARTESIAN_POINT('',(0.00641955949953335,-0.00651059726184545,0.000650566707282241));
#24423=CARTESIAN_POINT('',(0.00612493232389993,-0.00672731104825322,0.00202957832596403));
#24424=CARTESIAN_POINT('',(0.00477313053179474,-0.00716073862106875,0.00434179768005672));
#24425=CARTESIAN_POINT('',(0.00371595591532296,-0.0073774524074765,0.00527500541546762));
#24426=CARTESIAN_POINT('',(0.00125387691687189,-0.00781087998029202,0.00632943200462332));
#24427=CARTESIAN_POINT('',(-0.000151027465107407,-0.00802759376669976,0.00645065085836811));
#24428=CARTESIAN_POINT('',(-0.00275737973266859,-0.00846102133951525,0.00583362257511966));
#24429=CARTESIAN_POINT('',(-0.00395882761825048,-0.008677735125923,0.00509537543812641));
#24430=CARTESIAN_POINT('',(-0.00568664980961529,-0.00911116269873846,0.00304876180318409));
#24431=CARTESIAN_POINT('',(-0.00621302411539821,-0.00932787648514618,0.00174039530523502));
#24432=CARTESIAN_POINT('',(-0.0063664229490903,-0.00971463315675964,-0.000644154363151915));
#24433=CARTESIAN_POINT('',(-0.00616271644222663,-0.00988467604196539,-0.0017096594755033));
#24434=CARTESIAN_POINT('',(-0.0057207606233364,-0.0100547189271711,-0.00266407966842101));
#24435=CARTESIAN_POINT('',(0.00629970494285292,6.37733818485945E-5,-0.000371039548892805));
#24436=CARTESIAN_POINT('',(0.00635927838769681,-0.000106269263185143,0.000679045059853386));
#24437=CARTESIAN_POINT('',(0.00615644245053335,-0.000276311908218883,0.00174470807187195));
#24438=CARTESIAN_POINT('',(0.00513601119402079,-0.000663068339660396,0.00390532232119729));
#24439=CARTESIAN_POINT('',(0.00416496463702334,-0.000879782126068169,0.00492803338824204));
#24440=CARTESIAN_POINT('',(0.00180508138108541,-0.00131320969888372,0.00619486537879094));
#24441=CARTESIAN_POINT('',(0.000416244682144953,-0.0015299234852915,0.00643898630229508));
#24442=CARTESIAN_POINT('',(-0.00223420799892927,-0.00196335105810707,0.00605322470372089));
#24443=CARTESIAN_POINT('',(-0.00349582398106304,-0.00218006484451485,0.00542334218164257));
#24444=CARTESIAN_POINT('',(-0.00539683561184041,-0.00261349241733042,0.00353662053059805));
#24445=CARTESIAN_POINT('',(-0.00603623126048402,-0.00283020620373821,0.00227978140163185));
#24446=CARTESIAN_POINT('',(-0.00644191767224521,-0.00326363377655378,-0.000367681599679004));
#24447=CARTESIAN_POINT('',(-0.00620820843536279,-0.00348034756296157,-0.00175830547202366));
#24448=CARTESIAN_POINT('',(-0.00495938683078651,-0.00391377513577715,-0.00412770696522788));
#24449=CARTESIAN_POINT('',(-0.00394427446309265,-0.00413048892218493,-0.00510648458608745));
#24450=CARTESIAN_POINT('',(-0.00153094520151119,-0.00456391649500051,-0.00626814930095857));
#24451=CARTESIAN_POINT('',(-0.000132728307623607,-0.00478063028140828,-0.00645103639497011));
#24452=CARTESIAN_POINT('',(0.00249819254669687,-0.00521405785422385,-0.00594916140077757));
#24453=CARTESIAN_POINT('',(0.00373089650712975,-0.00543077164063163,-0.0052643993125735));
#24454=CARTESIAN_POINT('',(0.00554711600372078,-0.00586419921344719,-0.00329590502129811));
#24455=CARTESIAN_POINT('',(0.00613063153987892,-0.00608091299985495,-0.00201217281822681));
#24456=CARTESIAN_POINT('',(0.00641952163806455,-0.00651434057267049,0.00065056287035058));
#24457=CARTESIAN_POINT('',(0.00612489620009204,-0.00673105435907826,0.00202956635585666));
#24458=CARTESIAN_POINT('',(0.00477310238068363,-0.0071644819318938,0.00434177207287333));
#24459=CARTESIAN_POINT('',(0.00371593399924772,-0.00738119571830155,0.00527497430438391));
#24460=CARTESIAN_POINT('',(0.00125386952171934,-0.00781462329111707,0.00632939467471113));
#24461=CARTESIAN_POINT('',(-0.000151026574373135,-0.00803133707752481,0.00645061281352777));
#24462=CARTESIAN_POINT('',(-0.00275736347011246,-0.0084647646503403,0.00583358816940706));
#24463=CARTESIAN_POINT('',(-0.0039588042697593,-0.00868147843674805,0.00509534538646972));
#24464=CARTESIAN_POINT('',(-0.00568661627072304,-0.00911490600956351,0.00304874382210612));
#24465=CARTESIAN_POINT('',(-0.00621298747203993,-0.00933161979597122,0.00174038504067986));
#24466=CARTESIAN_POINT('',(-0.00636638540101182,-0.00971837646758469,-0.000644150564039167));
#24467=CARTESIAN_POINT('',(-0.00616268009557444,-0.00988841935279044,-0.00170964939222283));
#24468=CARTESIAN_POINT('',(-0.00572072688326437,-0.0100584622379962,-0.00266406395613276));
#24469=CARTESIAN_POINT('',(0.00629970494285293,-9.58825219423124E-5,-0.000371039548892805));
#24470=CARTESIAN_POINT('',(0.00635927838769681,-0.00026592516697605,0.000679045059853387));
#24471=CARTESIAN_POINT('',(0.00615644245053335,-0.00043596781200979,0.00174470807187195));
#24472=CARTESIAN_POINT('',(0.00513601119402079,-0.000822724243451304,0.00390532232119729));
#24473=CARTESIAN_POINT('',(0.00416496463702333,-0.00103943802985908,0.00492803338824205));
#24474=CARTESIAN_POINT('',(0.00180508138108541,-0.00147286560267463,0.00619486537879095));
#24475=CARTESIAN_POINT('',(0.000416244682144946,-0.00168957938908242,0.0064389863022951));
#24476=CARTESIAN_POINT('',(-0.00223420799892928,-0.00212300696189798,0.00605322470372089));
#24477=CARTESIAN_POINT('',(-0.00349582398106304,-0.00233972074830577,0.00542334218164257));
#24478=CARTESIAN_POINT('',(-0.00539683561184041,-0.00277314832112133,0.00353662053059804));
#24479=CARTESIAN_POINT('',(-0.00603623126048403,-0.00298986210752912,0.00227978140163184));
#24480=CARTESIAN_POINT('',(-0.00644191767224521,-0.00342328968034468,-0.000367681599679018));
#24481=CARTESIAN_POINT('',(-0.00620820843536279,-0.00364000346675248,-0.00175830547202367));
#24482=CARTESIAN_POINT('',(-0.00495938683078651,-0.00407343103956807,-0.0041277069652279));
#24483=CARTESIAN_POINT('',(-0.00394427446309265,-0.00429014482597584,-0.00510648458608746));
#24484=CARTESIAN_POINT('',(-0.00153094520151119,-0.00472357239879141,-0.00626814930095858));
#24485=CARTESIAN_POINT('',(-0.000132728307623605,-0.00494028618519919,-0.00645103639497012));
#24486=CARTESIAN_POINT('',(0.00249819254669687,-0.00537371375801476,-0.00594916140077757));
#24487=CARTESIAN_POINT('',(0.00373089650712976,-0.00559042754442254,-0.00526439931257351));
#24488=CARTESIAN_POINT('',(0.00554711600372077,-0.00602385511723811,-0.00329590502129811));
#24489=CARTESIAN_POINT('',(0.00613063153987892,-0.00624056890364588,-0.00201217281822679));
#24490=CARTESIAN_POINT('',(0.00641952163806455,-0.00667399647646141,0.000650562870350614));
#24491=CARTESIAN_POINT('',(0.00612489620009204,-0.00689071026286918,0.00202956635585669));
#24492=CARTESIAN_POINT('',(0.00477310238068361,-0.00732413783568471,0.00434177207287336));
#24493=CARTESIAN_POINT('',(0.0037159339992477,-0.00754085162209245,0.00527497430438394));
#24494=CARTESIAN_POINT('',(0.00125386952171932,-0.00797427919490799,0.00632939467471114));
#24495=CARTESIAN_POINT('',(-0.000151026574373135,-0.00819099298131572,0.00645061281352778));
#24496=CARTESIAN_POINT('',(-0.00275736347011246,-0.00862442055413122,0.00583358816940704));
#24497=CARTESIAN_POINT('',(-0.00395880426975933,-0.00884113434053896,0.00509534538646969));
#24498=CARTESIAN_POINT('',(-0.00568661627072307,-0.00927456191335442,0.00304874382210608));
#24499=CARTESIAN_POINT('',(-0.00621298747203995,-0.00949127569976213,0.00174038504067985));
#24500=CARTESIAN_POINT('',(-0.00636638540101182,-0.0098780323713756,-0.000644150564039162));
#24501=CARTESIAN_POINT('',(-0.00616268009557445,-0.0100480752565813,-0.00170964939222283));
#24502=CARTESIAN_POINT('',(-0.00572072688326439,-0.0102181181417871,-0.00266406395613277));
#24503=CARTESIAN_POINT('',(0.00636416127792705,-0.00025179511490817,-0.000374835893278158));
#24504=CARTESIAN_POINT('',(0.00642434425702011,-0.000421837759941906,0.00068599280682017));
#24505=CARTESIAN_POINT('',(0.00621943297486042,-0.000591880404975645,0.00176255930285932));
#24506=CARTESIAN_POINT('',(0.0051885610295241,-0.000978636836417156,0.00394528018690546));
#24507=CARTESIAN_POINT('',(0.00420757907034222,-0.00119535062282493,0.00497845526898258));
#24508=CARTESIAN_POINT('',(0.00182355033024902,-0.00162877819564049,0.00625824903282184));
#24509=CARTESIAN_POINT('',(0.00042050354933771,-0.00184549198204827,0.00650486771458397));
#24510=CARTESIAN_POINT('',(-0.00225706761865918,-0.00227891955486382,0.00611515914086064));
#24511=CARTESIAN_POINT('',(-0.00353159200574476,-0.00249563334127161,0.00547883188537516));
#24512=CARTESIAN_POINT('',(-0.00545205410980061,-0.00292906091408718,0.00357280597103028));
#24513=CARTESIAN_POINT('',(-0.00609799182677088,-0.00314577470049497,0.00230310731217089));
#24514=CARTESIAN_POINT('',(-0.00650782907726638,-0.00357920227331054,-0.000371443586725145));
#24515=CARTESIAN_POINT('',(-0.00627172861079161,-0.00379591605971833,-0.00177629582676178));
#24516=CARTESIAN_POINT('',(-0.00501012950877337,-0.0042293436325339,-0.00416994019133164));
#24517=CARTESIAN_POINT('',(-0.0039846308732299,-0.00444605741894169,-0.00515873231586488));
#24518=CARTESIAN_POINT('',(-0.00154660928701741,-0.00487948499175726,-0.0063322827699547));
#24519=CARTESIAN_POINT('',(-0.000134086336348389,-0.00509619877816504,-0.00651704109951128));
#24520=CARTESIAN_POINT('',(0.00252375316220668,-0.00552962635098061,-0.0060100310993011));
#24521=CARTESIAN_POINT('',(0.00376906971009273,-0.00574634013738839,-0.00531826276953433));
#24522=CARTESIAN_POINT('',(0.00560387211707439,-0.00617976771020394,-0.00332962754645642));
#24523=CARTESIAN_POINT('',(0.00619335797617,-0.00639648149661172,-0.0020327606531453));
#24524=CARTESIAN_POINT('',(0.00648520389484837,-0.00682990906942726,0.000657219197708537));
#24525=CARTESIAN_POINT('',(0.00618756395443112,-0.00704662285583503,0.00205033215525125));
#24526=CARTESIAN_POINT('',(0.0048219390625891,-0.00748005042865056,0.00438619553684241));
#24527=CARTESIAN_POINT('',(0.00375395411116432,-0.00769676421505832,0.00532894596089087));
#24528=CARTESIAN_POINT('',(0.00126669866764987,-0.00813019178787383,0.00639415478453699));
#24529=CARTESIAN_POINT('',(-0.000152571824439797,-0.00834690557428157,0.00651661318413464));
#24530=CARTESIAN_POINT('',(-0.00278557583011391,-0.00878033314709707,0.00589327536383009));
#24531=CARTESIAN_POINT('',(-0.00399930934369837,-0.0089970469335048,0.00514747914392788));
#24532=CARTESIAN_POINT('',(-0.00574479970107554,-0.00943047450632027,0.00307993748198947));
#24533=CARTESIAN_POINT('',(-0.00627655654486826,-0.00964718829272799,0.00175819203995327));
#24534=CARTESIAN_POINT('',(-0.00643152398676165,-0.0100339449643414,-0.00065074128296498));
#24535=CARTESIAN_POINT('',(-0.00622573444126181,-0.0102039878495472,-0.00172714191529876));
#24536=CARTESIAN_POINT('',(-0.00577925932124365,-0.0103740307347529,-0.0026913217087693));
#24537=CARTESIAN_POINT('',(0.00658422897131801,-0.000472288818425242,-0.000387797423766075));
#24538=CARTESIAN_POINT('',(0.00664649303051135,-0.000642331463458977,0.000709713898742101));
#24539=CARTESIAN_POINT('',(0.00643449607731892,-0.000812374108492715,0.00182350721780144));
#24540=CARTESIAN_POINT('',(0.00536797739059997,-0.00119913053993422,0.00408170487392976));
#24541=CARTESIAN_POINT('',(0.00435307384653242,-0.001415844326342,0.00515060633804724));
#24542=CARTESIAN_POINT('',(0.00188660726696621,-0.00184927189915755,0.00647465436404686));
#24543=CARTESIAN_POINT('',(0.00043504423146757,-0.00206598568556533,0.00672980092592901));
#24544=CARTESIAN_POINT('',(-0.00233511524237175,-0.0024994132583809,0.00632661653612109));
#24545=CARTESIAN_POINT('',(-0.00365371168071242,-0.00271612704478867,0.00566828558443103));
#24546=CARTESIAN_POINT('',(-0.0056405818544302,-0.00314955461760424,0.00369635079251448));
#24547=CARTESIAN_POINT('',(-0.00630885558980731,-0.00336626840401203,0.00238274695228799));
#24548=CARTESIAN_POINT('',(-0.00673286469020471,-0.0037996959768276,-0.000384287813919532));
#24549=CARTESIAN_POINT('',(-0.00648860005522499,-0.00401640976323539,-0.00183771873990057));
#24550=CARTESIAN_POINT('',(-0.00518337584814724,-0.00444983733605096,-0.0043141334446779));
#24551=CARTESIAN_POINT('',(-0.0041224162760492,-0.00466655112245875,-0.00533711722347419));
#24552=CARTESIAN_POINT('',(-0.00160008982019489,-0.00509997869527432,-0.00655124812960334));
#24553=CARTESIAN_POINT('',(-0.000138722936438618,-0.0053166924816821,-0.0067423952569362));
#24554=CARTESIAN_POINT('',(0.00261102256234292,-0.00575012005449767,-0.00621785324953767));
#24555=CARTESIAN_POINT('',(0.00389940117736819,-0.00596683384090545,-0.00550216411480628));
#24556=CARTESIAN_POINT('',(0.0057976496090339,-0.00640026141372101,-0.00344476344920941));
#24557=CARTESIAN_POINT('',(0.00640751942567434,-0.00661697520012878,-0.00210305191834394));
#24558=CARTESIAN_POINT('',(0.00670945714676693,-0.00705040277294432,0.000679945320849618));
#24559=CARTESIAN_POINT('',(0.00640152505121908,-0.00726711655935209,0.0021212310291777));
#24560=CARTESIAN_POINT('',(0.0049886779242921,-0.00770054413216763,0.00453786673001321));
#24561=CARTESIAN_POINT('',(0.00388376289291296,-0.00791725791857539,0.00551321672252064));
#24562=CARTESIAN_POINT('',(0.00131050011167958,-0.0083506854913909,0.00661525962980517));
#24563=CARTESIAN_POINT('',(-0.000157847638174655,-0.00856739927779865,0.00674195254458227));
#24564=CARTESIAN_POINT('',(-0.00288189885225745,-0.00900082685061413,0.00609706019252922));
#24565=CARTESIAN_POINT('',(-0.004137602316486,-0.00921754063702187,0.00532547492569906));
#24566=CARTESIAN_POINT('',(-0.00594345035809038,-0.00965096820983733,0.00318643929862331));
#24567=CARTESIAN_POINT('',(-0.00649359493546621,-0.00986768199624506,0.00181898893837771));
#24568=CARTESIAN_POINT('',(-0.00665392102966254,-0.0102544386678585,-0.000673243404907283));
#24569=CARTESIAN_POINT('',(-0.00644101544347415,-0.0104244815530643,-0.00178686512482473));
#24570=CARTESIAN_POINT('',(-0.00597910156483126,-0.01059452443827,-0.00278438549750075));
#24571=CARTESIAN_POINT('',(0.00673984032963485,-0.000536869928976456,-0.000396962609868636));
#24572=CARTESIAN_POINT('',(0.00680357593467928,-0.000706912574010191,0.00072648724369725));
#24573=CARTESIAN_POINT('',(0.00658656865545035,-0.00087695521904393,0.00186660390175619));
#24574=CARTESIAN_POINT('',(0.00549484391617253,-0.00126371165048544,0.00417817169524589));
#24575=CARTESIAN_POINT('',(0.00445595418940373,-0.00148042543689321,0.00527233552637138));
#24576=CARTESIAN_POINT('',(0.00193119525451979,-0.00191385300970877,0.00662767604124101));
#24577=CARTESIAN_POINT('',(0.000445326046404667,-0.00213056679611654,0.00688885272498515));
#24578=CARTESIAN_POINT('',(-0.00239030324635441,-0.00256399436893211,0.0064761394942418));
#24579=CARTESIAN_POINT('',(-0.00374006333099836,-0.0027807081553399,0.00580224957975431));
#24580=CARTESIAN_POINT('',(-0.00577389110109959,-0.00321413572815547,0.00378371017356644));
#24581=CARTESIAN_POINT('',(-0.00645795878655688,-0.00343084951456325,0.00243906068186606));
#24582=CARTESIAN_POINT('',(-0.00689198889812187,-0.00386427708737882,-0.000393370054067792));
#24583=CARTESIAN_POINT('',(-0.00664195132422956,-0.00408099087378661,-0.00188115129830126));
#24584=CARTESIAN_POINT('',(-0.00530587950953425,-0.00451441844660218,-0.0044160934719204));
#24585=CARTESIAN_POINT('',(-0.00421984526873124,-0.00473113223300997,-0.00546325440130608));
#24586=CARTESIAN_POINT('',(-0.00163790626786615,-0.00516455980582554,-0.00670608002025585));
#24587=CARTESIAN_POINT('',(-0.000142001507804065,-0.00538127359223332,-0.00690174470981995));
#24588=CARTESIAN_POINT('',(0.00267273134696934,-0.00581470116504889,-0.00636480570125073));
#24589=CARTESIAN_POINT('',(0.00399155944168066,-0.00603141495145667,-0.00563220200311741));
#24590=CARTESIAN_POINT('',(0.00593467098763979,-0.00646484252427222,-0.00352617682680408));
#24591=CARTESIAN_POINT('',(0.0065589544388876,-0.00668155631068,-0.00215275534862407));
#24592=CARTESIAN_POINT('',(0.00686802814190169,-0.00711498388349554,0.000696015116632774));
#24593=CARTESIAN_POINT('',(0.00655281839366796,-0.00733169766990331,0.0021713641037096));
#24594=CARTESIAN_POINT('',(0.0051065801040896,-0.00776512524271884,0.00464511445921495));
#24595=CARTESIAN_POINT('',(0.00397555156274497,-0.0079818390291266,0.00564351582764347));
#24596=CARTESIAN_POINT('',(0.00134147240977875,-0.00841526660194211,0.00677160436524751));
#24597=CARTESIAN_POINT('',(-0.000161578201842847,-0.00863198038834986,0.00690129153442303));
#24598=CARTESIAN_POINT('',(-0.00295000951439953,-0.00906540796116535,0.00624115782680529));
#24599=CARTESIAN_POINT('',(-0.00423539021533461,-0.00928212174757309,0.00545133695001203));
#24600=CARTESIAN_POINT('',(-0.00608391758475277,-0.00971554932038855,0.00326174745537375));
#24601=CARTESIAN_POINT('',(-0.00664706425323585,-0.00993226310679628,0.00186197883752874));
#24602=CARTESIAN_POINT('',(-0.0068111794868136,-0.0103190197784097,-0.00068915480792377));
#24603=CARTESIAN_POINT('',(-0.00659324209999915,-0.0104890626636155,-0.00182909581127476));
#24604=CARTESIAN_POINT('',(-0.00612041137043959,-0.0106591055488212,-0.00285019153359567));
#24605=CARTESIAN_POINT('',(0.00705106304626852,-0.000536869928976456,-0.00041529298207376));
#24606=CARTESIAN_POINT('',(0.00711774174301514,-0.000706912574010191,0.000760033933607546));
#24607=CARTESIAN_POINT('',(0.00689071381171319,-0.00087695521904393,0.0019527972696657));
#24608=CARTESIAN_POINT('',(0.00574857696731765,-0.00126371165048544,0.00437110533787816));
#24609=CARTESIAN_POINT('',(0.00466171487514634,-0.00148042543689321,0.00551579390301966));
#24610=CARTESIAN_POINT('',(0.00202037122962694,-0.00191385300970877,0.00693371939562929));
#24611=CARTESIAN_POINT('',(0.00046588967627886,-0.00213056679611654,0.00720695632309743));
#24612=CARTESIAN_POINT('',(-0.00250067925431972,-0.00256399436893211,0.00677518541048322));
#24613=CARTESIAN_POINT('',(-0.00391276663157022,-0.0027807081553399,0.00607017757040086));
#24614=CARTESIAN_POINT('',(-0.00604050959443837,-0.00321413572815547,0.00395842893567034));
#24615=CARTESIAN_POINT('',(-0.00675616518005603,-0.00343084951456325,0.00255168814102218));
#24616=CARTESIAN_POINT('',(-0.00721023731395619,-0.00386427708737882,-0.000411534534364311));
#24617=CARTESIAN_POINT('',(-0.00694865386223869,-0.00408099087378661,-0.00196801641510262));
#24618=CARTESIAN_POINT('',(-0.00555088683230826,-0.00451441844660218,-0.0046200135264054));
#24619=CARTESIAN_POINT('',(-0.00441470325409532,-0.00473113223300997,-0.00571552875696985));
#24620=CARTESIAN_POINT('',(-0.00171353916320868,-0.00516455980582554,-0.00701574380156088));
#24621=CARTESIAN_POINT('',(-0.000148558650534955,-0.00538127359223332,-0.00722044361558744));
#24622=CARTESIAN_POINT('',(0.00279614891622217,-0.00581470116504889,-0.00665871060467683));
#24623=CARTESIAN_POINT('',(0.0041758759703056,-0.00603141495145667,-0.00589227777973966));
#24624=CARTESIAN_POINT('',(0.00620871374485157,-0.00646484252427223,-0.00368900358199341));
#24625=CARTESIAN_POINT('',(0.00686182446531413,-0.00668155631068,-0.00225216220918432));
#24626=CARTESIAN_POINT('',(0.00718517013217121,-0.00711498388349554,0.000728154708199082));
#24627=CARTESIAN_POINT('',(0.00685540507856572,-0.00733169766990331,0.0022716302527734));
#24628=CARTESIAN_POINT('',(0.00534238446368461,-0.00776512524271884,0.00485960991761842));
#24629=CARTESIAN_POINT('',(0.00415912890240899,-0.0079818390291266,0.00590411403788912));
#24630=CARTESIAN_POINT('',(0.00140341700597708,-0.00841526660194211,0.00708429383613219));
#24631=CARTESIAN_POINT('',(-0.000169039329179231,-0.00863198038834986,0.00721996951410456));
#24632=CARTESIAN_POINT('',(-0.00308623083868367,-0.00906540796116535,0.00652935309535746));
#24633=CARTESIAN_POINT('',(-0.00443096601303181,-0.00928212174757309,0.00570306099863799));
#24634=CARTESIAN_POINT('',(-0.00636485203807753,-0.00971554932038855,0.00341236376887466));
#24635=CARTESIAN_POINT('',(-0.00695400288877511,-0.00993226310679628,0.00194795863583079));
#24636=CARTESIAN_POINT('',(-0.0071256964011157,-0.0103190197784097,-0.000720977613956743));
#24637=CARTESIAN_POINT('',(-0.00689769541304913,-0.0104890626636155,-0.00191355718417482));
#24638=CARTESIAN_POINT('',(-0.00640303098165626,-0.0106591055488212,-0.00298180360578551));
#24639=CARTESIAN_POINT('',(0.00720667440458535,-0.000472288818425242,-0.000424458168176322));
#24640=CARTESIAN_POINT('',(0.00727482464718306,-0.000642331463458977,0.000776807278562694));
#24641=CARTESIAN_POINT('',(0.00704278638984461,-0.000812374108492715,0.00199589395362046));
#24642=CARTESIAN_POINT('',(0.00587544349289021,-0.00119913053993422,0.00446757215919429));
#24643=CARTESIAN_POINT('',(0.00476459521801765,-0.001415844326342,0.0056375230913438));
#24644=CARTESIAN_POINT('',(0.00206495921718051,-0.00184927189915755,0.00708674107282344));
#24645=CARTESIAN_POINT('',(0.000476171491215956,-0.00206598568556533,0.00736600812215358));
#24646=CARTESIAN_POINT('',(-0.00255586725830238,-0.0024994132583809,0.00692470836860393));
#24647=CARTESIAN_POINT('',(-0.00399911828185615,-0.00271612704478868,0.00620414156572414));
#24648=CARTESIAN_POINT('',(-0.00617381884110776,-0.00314955461760424,0.00404578831672229));
#24649=CARTESIAN_POINT('',(-0.0069052683768056,-0.00336626840401203,0.00260800187060023));
#24650=CARTESIAN_POINT('',(-0.00736936152187335,-0.0037996959768276,-0.000420616774512571));
#24651=CARTESIAN_POINT('',(-0.00710200513124325,-0.00401640976323539,-0.00201144897350331));
#24652=CARTESIAN_POINT('',(-0.00567339049369526,-0.00444983733605097,-0.0047219735536479));
#24653=CARTESIAN_POINT('',(-0.00451213224677736,-0.00466655112245875,-0.00584166593480174));
#24654=CARTESIAN_POINT('',(-0.00175135561087993,-0.00509997869527433,-0.00717057569221338));
#24655=CARTESIAN_POINT('',(-0.0001518372219004,-0.00531669248168211,-0.00737979306847118));
#24656=CARTESIAN_POINT('',(0.00285785770084859,-0.00575012005449767,-0.00680566305638988));
#24657=CARTESIAN_POINT('',(0.00426803423461806,-0.00596683384090546,-0.00602231566805078));
#24658=CARTESIAN_POINT('',(0.00634573512345746,-0.00640026141372101,-0.00377041695958807));
#24659=CARTESIAN_POINT('',(0.00701325947852739,-0.00661697520012879,-0.00230186563946444));
#24660=CARTESIAN_POINT('',(0.00734374112730596,-0.00705040277294433,0.000744224503982235));
#24661=CARTESIAN_POINT('',(0.00700669842101459,-0.00726711655935209,0.00232176332730529));
#24662=CARTESIAN_POINT('',(0.00546028664348212,-0.00770054413216762,0.00496685764682015));
#24663=CARTESIAN_POINT('',(0.00425091757224101,-0.00791725791857539,0.00603441314301195));
#24664=CARTESIAN_POINT('',(0.00143438930407624,-0.0083506854913909,0.00724063857157453));
#24665=CARTESIAN_POINT('',(-0.000172769892847422,-0.00856739927779865,0.00737930850394532));
#24666=CARTESIAN_POINT('',(-0.00315434150082575,-0.00900082685061413,0.00667345072963354));
#24667=CARTESIAN_POINT('',(-0.00452875391188042,-0.00921754063702187,0.00582892302295097));
#24668=CARTESIAN_POINT('',(-0.00650531926473991,-0.00965096820983733,0.00348767192562511));
#24669=CARTESIAN_POINT('',(-0.00710747220654474,-0.00986768199624506,0.00199094853498182));
#24670=CARTESIAN_POINT('',(-0.00728295485826675,-0.0102544386678585,-0.000736889016973229));
#24671=CARTESIAN_POINT('',(-0.00704992206957412,-0.0104244815530643,-0.00195578787062486));
#24672=CARTESIAN_POINT('',(-0.00654434078726459,-0.01059452443827,-0.00304760964188044));
#24673=CARTESIAN_POINT('',(0.00742674209797632,-0.00025179511490817,-0.000437419698664237));
#24674=CARTESIAN_POINT('',(0.0074969734206743,-0.000421837759941906,0.000800528370484627));
#24675=CARTESIAN_POINT('',(0.00725784949230312,-0.000591880404975645,0.00205684186856258));
#24676=CARTESIAN_POINT('',(0.00605485985396608,-0.000978636836417156,0.00460399684621859));
#24677=CARTESIAN_POINT('',(0.00491008999420785,-0.00119535062282493,0.00580967416040847));
#24678=CARTESIAN_POINT('',(0.00212801615389771,-0.00162877819564049,0.00730314640404848));
#24679=CARTESIAN_POINT('',(0.00049071217334581,-0.00184549198204827,0.00759094133349861));
#24680=CARTESIAN_POINT('',(-0.00263391488201495,-0.00227891955486382,0.00713616576386438));
#24681=CARTESIAN_POINT('',(-0.00412123795682381,-0.00249563334127161,0.00639359526478001));
#24682=CARTESIAN_POINT('',(-0.00636234658573735,-0.00292906091408718,0.00416933313820649));
#24683=CARTESIAN_POINT('',(-0.00711613213984203,-0.00314577470049497,0.00268764151071733));
#24684=CARTESIAN_POINT('',(-0.00759439713481168,-0.00357920227331054,-0.000433461001706966));
#24685=CARTESIAN_POINT('',(-0.00731887657567664,-0.00379591605971833,-0.00207287188664212));
#24686=CARTESIAN_POINT('',(-0.00584663683306913,-0.0042293436325339,-0.00486616680699417));
#24687=CARTESIAN_POINT('',(-0.00464991764959665,-0.00444605741894168,-0.00602005084241107));
#24688=CARTESIAN_POINT('',(-0.0018048361440574,-0.00487948499175726,-0.00738954105186204));
#24689=CARTESIAN_POINT('',(-0.00015647382199062,-0.00509619877816504,-0.00760514722589611));
#24690=CARTESIAN_POINT('',(0.00294512710098484,-0.0055296263509806,-0.00701348520662647));
#24691=CARTESIAN_POINT('',(0.00439836570189353,-0.00574634013738838,-0.00620621701332274));
#24692=CARTESIAN_POINT('',(0.00653951261541697,-0.00617976771020394,-0.00388555286234104));
#24693=CARTESIAN_POINT('',(0.00722742092803174,-0.00639648149661171,-0.00237215690466308));
#24694=CARTESIAN_POINT('',(0.00756799437922453,-0.00682990906942726,0.000766950627123331));
#24695=CARTESIAN_POINT('',(0.00722065951780256,-0.00704662285583503,0.00239266220123176));
#24696=CARTESIAN_POINT('',(0.00562702550518511,-0.00748005042865056,0.00511852883999096));
#24697=CARTESIAN_POINT('',(0.00438072635398964,-0.00769676421505832,0.00621868390464172));
#24698=CARTESIAN_POINT('',(0.00147819074810594,-0.00813019178787383,0.00746174341684272));
#24699=CARTESIAN_POINT('',(-0.000178045706582277,-0.00834690557428157,0.00760464786439295));
#24700=CARTESIAN_POINT('',(-0.00325066452296929,-0.00878033314709707,0.00687723555833265));
#24701=CARTESIAN_POINT('',(-0.00466704688466808,-0.00899704693350481,0.00600691880472212));
#24702=CARTESIAN_POINT('',(-0.00670396992175478,-0.00943047450632027,0.00359417374225892));
#24703=CARTESIAN_POINT('',(-0.0073245105971427,-0.00964718829272799,0.00205174543340626));
#24704=CARTESIAN_POINT('',(-0.00750535190116764,-0.0100339449643414,-0.00075939113891553));
#24705=CARTESIAN_POINT('',(-0.00726520307178647,-0.0102039878495472,-0.00201551108015082));
#24706=CARTESIAN_POINT('',(-0.0067441830308522,-0.0103740307347529,-0.00314067343061189));
#24707=CARTESIAN_POINT('',(0.00749119843305045,-9.58825219423123E-5,-0.000441216043049591));
#24708=CARTESIAN_POINT('',(0.00756203928999761,-0.00026592516697605,0.000807476117451413));
#24709=CARTESIAN_POINT('',(0.00732084001663019,-0.00043596781200979,0.00207469309954995));
#24710=CARTESIAN_POINT('',(0.00610740968946939,-0.000822724243451302,0.00464395471192676));
#24711=CARTESIAN_POINT('',(0.00495270442752674,-0.00103943802985908,0.005860096041149));
#24712=CARTESIAN_POINT('',(0.00214648510306132,-0.00147286560267463,0.00736653005807937));
#24713=CARTESIAN_POINT('',(0.000494971040538567,-0.00168957938908242,0.00765682274578751));
#24714=CARTESIAN_POINT('',(-0.00265677450174487,-0.00212300696189798,0.00719810020100412));
#24715=CARTESIAN_POINT('',(-0.00415700598150554,-0.00233972074830576,0.0064490849685126));
#24716=CARTESIAN_POINT('',(-0.00641756508369755,-0.00277314832112133,0.00420551857863874));
#24717=CARTESIAN_POINT('',(-0.00717789270612889,-0.00298986210752912,0.00271096742125639));
#24718=CARTESIAN_POINT('',(-0.00766030853983284,-0.0034232896803447,-0.000437222988753104));
#24719=CARTESIAN_POINT('',(-0.00738239675110546,-0.00364000346675248,-0.00209086224138024));
#24720=CARTESIAN_POINT('',(-0.00589737951105599,-0.00407343103956805,-0.00490840003309794));
#24721=CARTESIAN_POINT('',(-0.00469027405973391,-0.00429014482597584,-0.0060722985721885));
#24722=CARTESIAN_POINT('',(-0.00182050022956361,-0.0047235723987914,-0.00745367452085818));
#24723=CARTESIAN_POINT('',(-0.000157831850715397,-0.00494028618519919,-0.0076711519304373));
#24724=CARTESIAN_POINT('',(0.00297068771649466,-0.00537371375801475,-0.00707435490515));
#24725=CARTESIAN_POINT('',(0.00443653890485652,-0.00559042754442253,-0.00626008047028358));
#24726=CARTESIAN_POINT('',(0.00659626872877059,-0.00602385511723809,-0.00391927538749937));
#24727=CARTESIAN_POINT('',(0.00729014736432282,-0.00624056890364586,-0.00239274473958158));
#24728=CARTESIAN_POINT('',(0.00763367663600835,-0.00667399647646141,0.000773606954481276));
#24729=CARTESIAN_POINT('',(0.00728332727214165,-0.00689071026286918,0.00241342800062633));
#24730=CARTESIAN_POINT('',(0.0056758621870906,-0.00732413783568471,0.00516295230396004));
#24731=CARTESIAN_POINT('',(0.00441874646590625,-0.00754085162209247,0.00627265556114868));
#24732=CARTESIAN_POINT('',(0.00149101989403648,-0.00797427919490797,0.00752650352666857));
#24733=CARTESIAN_POINT('',(-0.00017959095664894,-0.00819099298131572,0.00767064823499982));
#24734=CARTESIAN_POINT('',(-0.00327887688297075,-0.00862442055413122,0.00693692275275568));
#24735=CARTESIAN_POINT('',(-0.00470755195860714,-0.00884113434053896,0.00605905256218029));
#24736=CARTESIAN_POINT('',(-0.00676215335210728,-0.00927456191335442,0.00362536740214229));
#24737=CARTESIAN_POINT('',(-0.00738807966997103,-0.00949127569976214,0.00206955243267967));
#24738=CARTESIAN_POINT('',(-0.00757049048691747,-0.0098780323713756,-0.000765981857841343));
#24739=CARTESIAN_POINT('',(-0.00732825741747383,-0.0100480752565813,-0.00203300360322675));
#24740=CARTESIAN_POINT('',(-0.00680271546883148,-0.0102181181417871,-0.00316793118324842));
#24741=CARTESIAN_POINT('',(0.00749119843305045,6.37733790118039E-5,-0.000441216043049592));
#24742=CARTESIAN_POINT('',(0.00756203928999761,-0.000106269266021933,0.00080747611745141));
#24743=CARTESIAN_POINT('',(0.00732084001663019,-0.000276311911055674,0.00207469309954994));
#24744=CARTESIAN_POINT('',(0.00610740968946939,-0.000663068342497186,0.00464395471192676));
#24745=CARTESIAN_POINT('',(0.00495270442752674,-0.00087978212890496,0.00586009604114899));
#24746=CARTESIAN_POINT('',(0.00214648510306132,-0.00131320970172052,0.00736653005807937));
#24747=CARTESIAN_POINT('',(0.000494971040538567,-0.0015299234881283,0.00765682274578751));
#24748=CARTESIAN_POINT('',(-0.00265677450174487,-0.00196335106094386,0.00719810020100412));
#24749=CARTESIAN_POINT('',(-0.00415700598150554,-0.00218006484735165,0.00644908496851259));
#24750=CARTESIAN_POINT('',(-0.00641756508369755,-0.00261349242016722,0.00420551857863873));
#24751=CARTESIAN_POINT('',(-0.00717789270612889,-0.002830206206575,0.00271096742125639));
#24752=CARTESIAN_POINT('',(-0.00766030853983284,-0.00326363377939058,-0.000437222988753101));
#24753=CARTESIAN_POINT('',(-0.00738239675110545,-0.00348034756579837,-0.00209086224138024));
#24754=CARTESIAN_POINT('',(-0.00589737951105599,-0.00391377513861393,-0.00490840003309794));
#24755=CARTESIAN_POINT('',(-0.00469027405973391,-0.00413048892502172,-0.0060722985721885));
#24756=CARTESIAN_POINT('',(-0.00182050022956361,-0.0045639164978373,-0.00745367452085817));
#24757=CARTESIAN_POINT('',(-0.000157831850715396,-0.00478063028424508,-0.00767115193043729));
#24758=CARTESIAN_POINT('',(0.00297068771649466,-0.00521405785706064,-0.00707435490514999));
#24759=CARTESIAN_POINT('',(0.00443653890485651,-0.00543077164346842,-0.00626008047028358));
#24760=CARTESIAN_POINT('',(0.00659626872877058,-0.00586419921628398,-0.00391927538749937));
#24761=CARTESIAN_POINT('',(0.00729014736432282,-0.00608091300269175,-0.00239274473958158));
#24762=CARTESIAN_POINT('',(0.00763367663600835,-0.00651434057550729,0.000773606954481275));
#24763=CARTESIAN_POINT('',(0.00728332727214164,-0.00673105436191506,0.00241342800062633));
#24764=CARTESIAN_POINT('',(0.00567586218709059,-0.00716448193473059,0.00516295230396004));
#24765=CARTESIAN_POINT('',(0.00441874646590625,-0.00738119572113835,0.00627265556114868));
#24766=CARTESIAN_POINT('',(0.00149101989403648,-0.00781462329395386,0.00752650352666857));
#24767=CARTESIAN_POINT('',(-0.000179590956648939,-0.00803133708036161,0.00767064823499982));
#24768=CARTESIAN_POINT('',(-0.00327887688297075,-0.0084647646531771,0.00693692275275568));
#24769=CARTESIAN_POINT('',(-0.00470755195860714,-0.00868147843958484,0.00605905256218029));
#24770=CARTESIAN_POINT('',(-0.00676215335210728,-0.0091149060124003,0.00362536740214228));
#24771=CARTESIAN_POINT('',(-0.00738807966997102,-0.00933161979880802,0.00206955243267967));
#24772=CARTESIAN_POINT('',(-0.00757049048691747,-0.00971837647042148,-0.000765981857841343));
#24773=CARTESIAN_POINT('',(-0.00732825741747383,-0.00988841935562723,-0.00203300360322675));
#24774=CARTESIAN_POINT('',(-0.00680271546883148,-0.010058462240833,-0.00316793118324842));
#24775=CARTESIAN_POINT('',(0.0074911612783006,6.75166870000634E-5,-0.000441213854711924));
#24776=CARTESIAN_POINT('',(0.00756200178389218,-0.000102525958033674,0.000807472112541725));
#24777=CARTESIAN_POINT('',(0.00732080370682183,-0.000272568603067414,0.00207468280951373));
#24778=CARTESIAN_POINT('',(0.00610737939801719,-0.000659325034508927,0.00464393167889977));
#24779=CARTESIAN_POINT('',(0.00495267986316688,-0.000876038820916701,0.00586006697631985));
#24780=CARTESIAN_POINT('',(0.00214647445695205,-0.00130946639373226,0.00736649352165812));
#24781=CARTESIAN_POINT('',(0.000494968585587552,-0.00152618018014004,0.00765678476957631));
#24782=CARTESIAN_POINT('',(-0.00265676132470878,-0.0019596077529556,0.00719806449995911));
#24783=CARTESIAN_POINT('',(-0.00415698536364062,-0.00217632153936339,0.00644905298242372));
#24784=CARTESIAN_POINT('',(-0.0064175332539406,-0.00260974911217896,0.00420549772016165));
#24785=CARTESIAN_POINT('',(-0.00717785710530876,-0.00282646289858674,0.00271095397543496));
#24786=CARTESIAN_POINT('',(-0.00766027054633285,-0.00325989047140232,-0.000437220820220132));
#24787=CARTESIAN_POINT('',(-0.00738236013598878,-0.00347660425781011,-0.00209085187114853));
#24788=CARTESIAN_POINT('',(-0.00589735026130877,-0.00391003183062568,-0.00490837568847844));
#24789=CARTESIAN_POINT('',(-0.00469025079697282,-0.00412674561703346,-0.00607226845487996));
#24790=CARTESIAN_POINT('',(-0.00182049120026993,-0.00456017318984904,-0.00745363755221893));
#24791=CARTESIAN_POINT('',(-0.000157831067903008,-0.00477688697625682,-0.00767111388315639));
#24792=CARTESIAN_POINT('',(0.00297067298251585,-0.00521031454907239,-0.00707431981785531));
#24793=CARTESIAN_POINT('',(0.00443651690056778,-0.00542702833548016,-0.0062600494216168));
#24794=CARTESIAN_POINT('',(0.00659623601268159,-0.00586045590829572,-0.0039192559487276));
#24795=CARTESIAN_POINT('',(0.00729011120674347,-0.00607716969470349,-0.00239273287207692));
#24796=CARTESIAN_POINT('',(0.00763363877459693,-0.00651059726751903,0.00077360311755543));
#24797=CARTESIAN_POINT('',(0.0072832911483885,-0.0067273110539268,0.00241341603053711));
#24798=CARTESIAN_POINT('',(0.00567583403602215,-0.00716073862674233,0.00516292669681546));
#24799=CARTESIAN_POINT('',(0.00441872454986423,-0.00737745241315009,0.00627262445011212));
#24800=CARTESIAN_POINT('',(0.00149101249889514,-0.0078108799859656,0.00752646619681296));
#24801=CARTESIAN_POINT('',(-0.000179590065916016,-0.00802759377237335,0.00767061019021714));
#24802=CARTESIAN_POINT('',(-0.00327886062043926,-0.00846102134518883,0.00693688834709523));
#24803=CARTESIAN_POINT('',(-0.00470752861015135,-0.00867773513159658,0.00605902251056914));
#24804=CARTESIAN_POINT('',(-0.00676211981326586,-0.00911116270441204,0.00362534942109156));
#24805=CARTESIAN_POINT('',(-0.00738804302666828,-0.00932787649081976,0.00206954216814007));
#24806=CARTESIAN_POINT('',(-0.00757045293889591,-0.00971463316243323,-0.000765978058734354));
#24807=CARTESIAN_POINT('',(-0.00732822107087673,-0.00988467604763897,-0.00203299351996157));
#24808=CARTESIAN_POINT('',(-0.00680268172881059,-0.0100547189328447,-0.00316791547098399));
#24809=CARTESIAN_POINT('',(0.00749108723007599,7.12593629933681E-5,-0.000441209493425148));
#24810=CARTESIAN_POINT('',(0.00756192703542718,-9.87832820403692E-5,0.000807464130885192));
#24811=CARTESIAN_POINT('',(0.0073207313425385,-0.000268825927074109,0.00207466230180165));
#24812=CARTESIAN_POINT('',(0.00610731902812464,-0.000655582358515622,0.00464388577481585));
#24813=CARTESIAN_POINT('',(0.00495263090718565,-0.000872296144923396,0.00586000905104771));
#24814=CARTESIAN_POINT('',(0.00214645323959778,-0.00130572371773895,0.00736642070574259));
#24815=CARTESIAN_POINT('',(0.000494963692948929,-0.00152243750414673,0.0076567090842056));
#24816=CARTESIAN_POINT('',(-0.00265673506329857,-0.0019558650769623,0.00719799334892164));
#24817=CARTESIAN_POINT('',(-0.00415694427289721,-0.00217257886337008,0.00644898923517466));
#24818=CARTESIAN_POINT('',(-0.00641746981825604,-0.00260600643618565,0.00420545614988593));
#24819=CARTESIAN_POINT('',(-0.00717778615401624,-0.00282272022259344,0.00271092717834417));
#24820=CARTESIAN_POINT('',(-0.00766019482650612,-0.00325614779540901,-0.000437216498403487));
#24821=CARTESIAN_POINT('',(-0.0073822871632358,-0.0034728615818168,-0.00209083120360938));
#24822=CARTESIAN_POINT('',(-0.00589729196750083,-0.00390628915463237,-0.00490832717043271));
#24823=CARTESIAN_POINT('',(-0.00469020443503618,-0.00412300294104016,-0.00607220843205016));
#24824=CARTESIAN_POINT('',(-0.00182047320517728,-0.00455643051385573,-0.00745356387490681));
#24825=CARTESIAN_POINT('',(-0.000157829507783031,-0.00477314430026351,-0.00767103805614603));
#24826=CARTESIAN_POINT('',(0.0029706436181687,-0.00520657187307908,-0.00707424989000256));
#24827=CARTESIAN_POINT('',(0.0044364730467262,-0.00542328565948686,-0.00625998754261988));
#24828=CARTESIAN_POINT('',(0.00659617081056569,-0.00585671323230241,-0.00391921720787901));
#24829=CARTESIAN_POINT('',(0.0072900391458477,-0.00607342701871018,-0.00239270922052083));
#24830=CARTESIAN_POINT('',(0.00763356331801849,-0.00650685459152572,0.000773595470685301));
#24831=CARTESIAN_POINT('',(0.00728321915490727,-0.00672356837793349,0.00241339217453326));
#24832=CARTESIAN_POINT('',(0.00567577793184578,-0.00715699595074902,0.00516287566259773));
#24833=CARTESIAN_POINT('',(0.00441868087189551,-0.00737370973715678,0.00627256244681424));
#24834=CARTESIAN_POINT('',(0.00149099776061568,-0.00780713730997229,0.00752639179960821));
#24835=CARTESIAN_POINT('',(-0.000179588290713876,-0.00802385109638004,0.00767053436818566));
#24836=CARTESIAN_POINT('',(-0.00327882820973568,-0.00845727866919553,0.00693681977771762));
#24837=CARTESIAN_POINT('',(-0.00470748207742792,-0.00867399245560327,0.00605896261867213));
#24838=CARTESIAN_POINT('',(-0.00676205297143077,-0.00910742002841873,0.00362531358543428));
#24839=CARTESIAN_POINT('',(-0.00738796999774137,-0.00932413381482645,0.00206952171124192));
#24840=CARTESIAN_POINT('',(-0.00757037810689339,-0.00971089048643992,-0.000765970487235993));
#24841=CARTESIAN_POINT('',(-0.00732814863327465,-0.00988093337164566,-0.00203297342433751));
#24842=CARTESIAN_POINT('',(-0.00680261448603128,-0.0100509762568514,-0.003167884156945));
#24843=CARTESIAN_POINT('',(0.00750327656949163,-8.53080491936399E-9,5.83924182010614E-10));
#24844=CARTESIAN_POINT('',(0.00750045193429679,-0.000208387270651741,0.00153290805400538));
#24845=CARTESIAN_POINT('',(0.00653694841133434,-0.00062514475034539,0.00459055487999984));
#24846=CARTESIAN_POINT('',(0.00270641832097577,-0.00125028096988588,0.00751610457455796));
#24847=CARTESIAN_POINT('',(-0.00210705546339051,-0.00187541718942638,0.00770553350902045));
#24848=CARTESIAN_POINT('',(-0.00615519750508701,-0.00250055340896689,0.0050930536775311));
#24849=CARTESIAN_POINT('',(-0.00796476961812452,-0.00312568962850741,0.000627460647780618));
#24850=CARTESIAN_POINT('',(-0.00687737551287545,-0.00375082584804793,-0.00406674126964439));
#24851=CARTESIAN_POINT('',(-0.00328822051990866,-0.00437596206758845,-0.00728203064254025));
#24852=CARTESIAN_POINT('',(0.00149719851208568,-0.00500109828712896,-0.00784857616360702));
#24853=CARTESIAN_POINT('',(0.00573800786308136,-0.00562623450666946,-0.00556018257780444));
#24854=CARTESIAN_POINT('',(0.00789149013387365,-0.00625137072620993,-0.00124942470180139));
#24855=CARTESIAN_POINT('',(0.00717446965196578,-0.00687650694575041,0.00351542988874914));
#24856=CARTESIAN_POINT('',(0.00384807543662403,-0.00750164316529085,0.00700128328974673));
#24857=CARTESIAN_POINT('',(-0.000877510408965592,-0.00812677938483126,0.00794008218231011));
#24858=CARTESIAN_POINT('',(-0.00528323049698942,-0.00875191560437166,0.00599199497594793));
#24859=CARTESIAN_POINT('',(-0.00776779806369973,-0.009377051823912,0.00186177392815872));
#24860=CARTESIAN_POINT('',(-0.00753804409837646,-0.00979380930360554,-0.00133584335935025));
#24861=CARTESIAN_POINT('',(-0.00697636861983814,-0.0100021880434523,-0.00276214414835674));
#24862=CARTESIAN_POINT('',(0.00750327646842837,-8.5308003845869E-9,5.83738566996586E-10));
#24863=CARTESIAN_POINT('',(-0.00586675988532295,-0.0100021881184342,-0.00232281882532306));
#24864=CARTESIAN_POINT('',(-0.00633909957834279,-0.0097938093874645,-0.00112337476477271));
#24865=CARTESIAN_POINT('',(-0.00653231086002425,-0.00937705192552518,0.00156565350772152));
#24866=CARTESIAN_POINT('',(-0.00444292037225485,-0.00875191573261618,0.00503895285821675));
#24867=CARTESIAN_POINT('',(-0.000737941280445877,-0.00812677953970714,0.00667719248116907));
#24868=CARTESIAN_POINT('',(0.00323602849815479,-0.00750164334679806,0.00588771257234701));
#24869=CARTESIAN_POINT('',(0.00603335200295941,-0.00687650715388895,0.00295629339011012));
#24870=CARTESIAN_POINT('',(0.00663632948134336,-0.00625137096097982,-0.00105069907242596));
#24871=CARTESIAN_POINT('',(0.00482536482892095,-0.0056262347680707,-0.00467582061643415));
#24872=CARTESIAN_POINT('',(0.00125906729727915,-0.00500109857516152,-0.00660024047415044));
#24873=CARTESIAN_POINT('',(-0.00276521905501561,-0.00437596238225236,-0.0061238066311924));
#24874=CARTESIAN_POINT('',(-0.00578351087799506,-0.00375082618934319,-0.00341991802437042));
#24875=CARTESIAN_POINT('',(-0.00669795362144113,-0.003125689996434,0.000527659058564769));
#24876=CARTESIAN_POINT('',(-0.00517619987335009,-0.00250055380352483,0.00428298895775701));
#24877=CARTESIAN_POINT('',(-0.00177192579579772,-0.00187541761061565,0.00647994872559159));
#24878=CARTESIAN_POINT('',(0.00227595305361633,-0.00125028141770649,0.00632065066437801));
#24879=CARTESIAN_POINT('',(0.00549722889407064,-0.000625145224797345,0.00386041839750601));
#24880=CARTESIAN_POINT('',(0.0063074860203521,-0.000208387762857922,0.00128909831370986));
#24881=CARTESIAN_POINT('',(0.006309862017394,-9.03188821431785E-9,3.59097525483689E-9));
#24882=CARTESIAN_POINT('',(0.006309861940649,-9.03189165685046E-9,3.59083324543894E-9));
#24883=CARTESIAN_POINT('',(0.006309862017394,-9.03188821431785E-9,3.59097525483689E-9));
#24884=CARTESIAN_POINT('',(0.00630986901478792,-0.000155917358435469,3.33265209946742E-9));
#24885=CARTESIAN_POINT('',(0.00643899489450502,-0.000467728700051866,2.8884814458691E-9));
#24886=CARTESIAN_POINT('',(0.00690656929312651,-0.000661460863890071,2.25531077613276E-9));
#24887=CARTESIAN_POINT('',(0.00737414369198757,-0.000467728449513883,1.49442951234317E-9));
#24888=CARTESIAN_POINT('',(0.00750326957200423,-0.000155916940868211,8.91109424662301E-10));
#24889=CARTESIAN_POINT('',(0.00750327656949163,-8.53080492228456E-9,5.83924176101713E-10));
#24890=CARTESIAN_POINT('',(0.00749108680181898,4.8779357875437E-5,-0.000441209536398754));
#24891=CARTESIAN_POINT('',(0.00756192661576567,-0.000121263290243651,0.000807464039153491));
#24892=CARTESIAN_POINT('',(0.00732073093746893,-0.000291305938362742,0.0020746621637675));
#24893=CARTESIAN_POINT('',(0.00610731868211987,-0.000678062372889606,0.0046438855117206));
#24894=CARTESIAN_POINT('',(0.00495263062659871,-0.00089477615929738,0.00586000871905406));
#24895=CARTESIAN_POINT('',(0.00214645311799237,-0.00132820373211294,0.00736642028840452));
#24896=CARTESIAN_POINT('',(0.000494963664907198,-0.00154491751852072,0.0076567086504215));
#24897=CARTESIAN_POINT('',(-0.00265673491278359,-0.00197834509133628,0.00719799294112568));
#24898=CARTESIAN_POINT('',(-0.00415694403738921,-0.00219505887774407,0.00644898886981287));
#24899=CARTESIAN_POINT('',(-0.00641746945467996,-0.00262848645055964,0.00420545591162953));
#24900=CARTESIAN_POINT('',(-0.0071777857473651,-0.00284520023696742,0.00271092702475898));
#24901=CARTESIAN_POINT('',(-0.00766019439252454,-0.003278627809783,-0.000437216473633373));
#24902=CARTESIAN_POINT('',(-0.00738228674499883,-0.00349534159619078,-0.00209083108515518));
#24903=CARTESIAN_POINT('',(-0.00589729163339495,-0.00392876916900636,-0.00490832689235577));
#24904=CARTESIAN_POINT('',(-0.00469020416931679,-0.00414548295541414,-0.00607220808803455));
#24905=CARTESIAN_POINT('',(-0.00182047310203998,-0.00457891052822971,-0.00745356345263173));
#24906=CARTESIAN_POINT('',(-0.000157829498841341,-0.0047956243146375,-0.00767103762155014));
#24907=CARTESIAN_POINT('',(0.00297064344986951,-0.00522905188745306,-0.00707424948921717));
#24908=CARTESIAN_POINT('',(0.00443647279538173,-0.00544576567386084,-0.00625998718796581));
#24909=CARTESIAN_POINT('',(0.00659617043686546,-0.0058791932466764,-0.00391921698583922));
#24910=CARTESIAN_POINT('',(0.00729003873283697,-0.00609590703308417,-0.002392709084964));
#24911=CARTESIAN_POINT('',(0.0076335628855457,-0.00652933460589971,0.000773595426857932));
#24912=CARTESIAN_POINT('',(0.00728321874228292,-0.00674604839230748,0.00241339203780465));
#24913=CARTESIAN_POINT('',(0.00567577761028959,-0.00717947596512301,0.00516287537009956));
#24914=CARTESIAN_POINT('',(0.00441868062155905,-0.00739618975153077,0.00627256209144775));
#24915=CARTESIAN_POINT('',(0.00149099767614452,-0.00782961732434628,0.00752639137320712));
#24916=CARTESIAN_POINT('',(-0.000179588280539459,-0.00804633111075403,0.0076705339336183));
#24917=CARTESIAN_POINT('',(-0.00327882802397656,-0.00847975868356952,0.00693681938471822));
#24918=CARTESIAN_POINT('',(-0.00470748181072968,-0.00869647246997725,0.00605896227540695));
#24919=CARTESIAN_POINT('',(-0.00676205258833262,-0.00912990004279271,0.00362531338004534));
#24920=CARTESIAN_POINT('',(-0.00738796957918245,-0.00934661382920044,0.002069521593995));
#24921=CARTESIAN_POINT('',(-0.00756094313073936,-0.00971336659681803,-0.000619312571671788));
#24922=CARTESIAN_POINT('',(-0.00738067797570845,-0.0098634055780279,-0.00173515348405907));
#24923=CARTESIAN_POINT('',(-0.00697626028083462,-0.0100134445592378,-0.0027621141197859));
#24924=CARTESIAN_POINT('',(0.00749116113247787,5.25291749297248E-5,-0.000441213914320999));
#24925=CARTESIAN_POINT('',(0.00756200164933592,-0.000117513473189364,0.000807472051253157));
#24926=CARTESIAN_POINT('',(0.00732080357776379,-0.000287556121308455,0.00207468274969978));
#24927=CARTESIAN_POINT('',(0.00610737928227492,-0.000674312555835319,0.00464393159089162));
#24928=CARTESIAN_POINT('',(0.00495267976930757,-0.000891026342243092,0.00586006686526445));
#24929=CARTESIAN_POINT('',(0.00214647441627375,-0.00132445391505865,0.00736649338205411));
#24930=CARTESIAN_POINT('',(0.000494968576207295,-0.00154116770146643,0.00765678462447093));
#24931=CARTESIAN_POINT('',(-0.00265676127435993,-0.00197459527428199,0.00719806436354704));
#24932=CARTESIAN_POINT('',(-0.0041569852848607,-0.00219130906068978,0.00644905286020633));
#24933=CARTESIAN_POINT('',(-0.00641753313232054,-0.00262473663350535,0.00420549764046236));
#24934=CARTESIAN_POINT('',(-0.00717785696927964,-0.00284145041991313,0.00271095392405908));
#24935=CARTESIAN_POINT('',(-0.0076602704011614,-0.00327487799272871,-0.000437220811934266));
#24936=CARTESIAN_POINT('',(-0.00738235999608408,-0.00349159177913649,-0.00209085183152434));
#24937=CARTESIAN_POINT('',(-0.0058973501495468,-0.00392501935195207,-0.00490837559545876));
#24938=CARTESIAN_POINT('',(-0.00469025070808686,-0.00414173313835985,-0.00607226833980309));
#24939=CARTESIAN_POINT('',(-0.00182049116576941,-0.00457516071117542,-0.00745363741096344));
#24940=CARTESIAN_POINT('',(-0.000157831064911919,-0.00479187449758321,-0.00767111373777945));
#24941=CARTESIAN_POINT('',(0.00297067292621798,-0.00522530207039877,-0.00707431968378835));
#24942=CARTESIAN_POINT('',(0.00443651681649039,-0.00544201585680655,-0.00626004930298125));
#24943=CARTESIAN_POINT('',(0.00659623588767489,-0.00587544342962211,-0.00391925587445293));
#24944=CARTESIAN_POINT('',(0.007290111068587,-0.00609215721602988,-0.00239273282673172));
#24945=CARTESIAN_POINT('',(0.00763363862993019,-0.00652558478884542,0.00077360310289471));
#24946=CARTESIAN_POINT('',(0.00728329101036128,-0.00674229857525319,0.00241341598479994));
#24947=CARTESIAN_POINT('',(0.00567583392845819,-0.00717572614806872,0.00516292659897171));
#24948=CARTESIAN_POINT('',(0.00441872446612402,-0.00739243993447648,0.00627262433123825));
#24949=CARTESIAN_POINT('',(0.00149101247063865,-0.00782586750729199,0.00752646605417728));
#24950=CARTESIAN_POINT('',(-0.000179590062512566,-0.00804258129369974,0.00767061004484975));
#24951=CARTESIAN_POINT('',(-0.00327886055830087,-0.00847600886651523,0.00693688821563276));
#24952=CARTESIAN_POINT('',(-0.00470752852093795,-0.00869272265292296,0.0060590223957433));
#24953=CARTESIAN_POINT('',(-0.00676211968511546,-0.00912615022573842,0.00362534935238679));
#24954=CARTESIAN_POINT('',(-0.00738804288665588,-0.00934286401214615,0.00206954212891973));
#24955=CARTESIAN_POINT('',(-0.00756101815455094,-0.00970961677976375,-0.000619318716829726));
#24956=CARTESIAN_POINT('',(-0.00738075121083061,-0.00985965576097361,-0.00173517070120062));
#24957=CARTESIAN_POINT('',(-0.0069763295031033,-0.0100096947421835,-0.00276214152699234));
#24958=CARTESIAN_POINT('',(0.00749119842919432,5.62796276046614E-5,-0.000441216111020545));
#24959=CARTESIAN_POINT('',(0.00756203929875053,-0.000113763020514427,0.000807476071465192));
#24960=CARTESIAN_POINT('',(0.00732084002631034,-0.000283805668633518,0.00207469307905365));
#24961=CARTESIAN_POINT('',(0.00610740968946939,-0.000670562103160382,0.00464395471192676));
#24962=CARTESIAN_POINT('',(0.00495270442752674,-0.000887275889568156,0.00586009604114899));
#24963=CARTESIAN_POINT('',(0.00214648510306132,-0.00132070346238371,0.00736653005807937));
#24964=CARTESIAN_POINT('',(0.000494971040538567,-0.00153741724879149,0.00765682274578751));
#24965=CARTESIAN_POINT('',(-0.00265677450174487,-0.00197084482160706,0.00719810020100412));
#24966=CARTESIAN_POINT('',(-0.00415700598150554,-0.00218755860801484,0.00644908496851259));
#24967=CARTESIAN_POINT('',(-0.00641756508369755,-0.00262098618083041,0.00420551857863873));
#24968=CARTESIAN_POINT('',(-0.00717789270612889,-0.0028376999672382,0.00271096742125639));
#24969=CARTESIAN_POINT('',(-0.00766030853983284,-0.00327112754005377,-0.000437222988753101));
#24970=CARTESIAN_POINT('',(-0.00738239675110545,-0.00348784132646156,-0.00209086224138024));
#24971=CARTESIAN_POINT('',(-0.00589737951105598,-0.00392126889927713,-0.00490840003309794));
#24972=CARTESIAN_POINT('',(-0.00469027405973391,-0.00413798268568492,-0.0060722985721885));
#24973=CARTESIAN_POINT('',(-0.00182050022956361,-0.00457141025850048,-0.00745367452085817));
#24974=CARTESIAN_POINT('',(-0.000157831850715397,-0.00478812404490827,-0.00767115193043729));
#24975=CARTESIAN_POINT('',(0.00297068771649466,-0.00522155161772383,-0.00707435490514999));
#24976=CARTESIAN_POINT('',(0.00443653890485651,-0.00543826540413161,-0.00626008047028358));
#24977=CARTESIAN_POINT('',(0.00659626872877058,-0.00587169297694717,-0.00391927538749937));
#24978=CARTESIAN_POINT('',(0.00729014736432282,-0.00608840676335494,-0.00239274473958158));
#24979=CARTESIAN_POINT('',(0.00763367663600835,-0.00652183433617048,0.000773606954481275));
#24980=CARTESIAN_POINT('',(0.00728332727214164,-0.00673854812257825,0.00241342800062633));
#24981=CARTESIAN_POINT('',(0.00567586218709059,-0.00717197569539378,0.00516295230396003));
#24982=CARTESIAN_POINT('',(0.00441874646590624,-0.00738868948180154,0.00627265556114867));
#24983=CARTESIAN_POINT('',(0.00149101989403648,-0.00782211705461705,0.00752650352666857));
#24984=CARTESIAN_POINT('',(-0.000179590956648939,-0.0080388308410248,0.00767064823499982));
#24985=CARTESIAN_POINT('',(-0.00327887688297075,-0.00847225841384029,0.00693692275275568));
#24986=CARTESIAN_POINT('',(-0.00470755195860714,-0.00868897220024802,0.00605905256218029));
#24987=CARTESIAN_POINT('',(-0.00676215335210727,-0.00912239977306348,0.00362536740214228));
#24988=CARTESIAN_POINT('',(-0.00738807966997102,-0.00933911355947121,0.00206955243267967));
#24989=CARTESIAN_POINT('',(-0.00756105579906895,-0.00970586632708881,-0.000619321800270888));
#24990=CARTESIAN_POINT('',(-0.00738078795784222,-0.00985590530829868,-0.00173517934020444));
#24991=CARTESIAN_POINT('',(-0.00697636423659504,-0.0100059442895085,-0.00276215527904059));
#24992=CARTESIAN_POINT('',(0.00749119842919431,0.000215942673245456,-0.000441216111020545));
#24993=CARTESIAN_POINT('',(0.00756203929875052,4.59000251263681E-5,0.000807476071465192));
#24994=CARTESIAN_POINT('',(0.00732084002631033,-0.000124142622992723,0.00207469307905365));
#24995=CARTESIAN_POINT('',(0.00610740968946938,-0.000510899057519587,0.00464395471192676));
#24996=CARTESIAN_POINT('',(0.00495270442752674,-0.000727612843927361,0.005860096041149));
#24997=CARTESIAN_POINT('',(0.00214648510306132,-0.00116104041674292,0.00736653005807936));
#24998=CARTESIAN_POINT('',(0.000494971040538565,-0.0013777542031507,0.00765682274578749));
#24999=CARTESIAN_POINT('',(-0.00265677450174487,-0.00181118177596626,0.00719810020100411));
#25000=CARTESIAN_POINT('',(-0.00415700598150554,-0.00202789556237405,0.0064490849685126));
#25001=CARTESIAN_POINT('',(-0.00641756508369755,-0.00246132313518961,0.00420551857863873));
#25002=CARTESIAN_POINT('',(-0.00717789270612888,-0.00267803692159741,0.00271096742125639));
#25003=CARTESIAN_POINT('',(-0.00766030853983282,-0.00311146449441299,-0.000437222988753105));
#25004=CARTESIAN_POINT('',(-0.00738239675110542,-0.00332817828082076,-0.00209086224138025));
#25005=CARTESIAN_POINT('',(-0.00589737951105598,-0.00376160585363634,-0.00490840003309796));
#25006=CARTESIAN_POINT('',(-0.00469027405973391,-0.00397831964004412,-0.0060722985721885));
#25007=CARTESIAN_POINT('',(-0.0018205002295636,-0.00441174721285969,-0.00745367452085817));
#25008=CARTESIAN_POINT('',(-0.000157831850715366,-0.00462846099926748,-0.00767115193043729));
#25009=CARTESIAN_POINT('',(0.00297068771649469,-0.00506188857208304,-0.00707435490514999));
#25010=CARTESIAN_POINT('',(0.00443653890485652,-0.00527860235849082,-0.00626008047028357));
#25011=CARTESIAN_POINT('',(0.00659626872877058,-0.00571202993130638,-0.00391927538749938));
#25012=CARTESIAN_POINT('',(0.0072901473643228,-0.00592874371771416,-0.00239274473958159));
#25013=CARTESIAN_POINT('',(0.00763367663600834,-0.0063621712905297,0.000773606954481287));
#25014=CARTESIAN_POINT('',(0.00728332727214164,-0.00657888507693747,0.00241342800062636));
#25015=CARTESIAN_POINT('',(0.00567586218709056,-0.00701231264975299,0.00516295230396007));
#25016=CARTESIAN_POINT('',(0.00441874646590621,-0.00722902643616075,0.00627265556114869));
#25017=CARTESIAN_POINT('',(0.00149101989403646,-0.00766245400897627,0.00752650352666855));
#25018=CARTESIAN_POINT('',(-0.000179590956648946,-0.00787916779538399,0.00767064823499983));
#25019=CARTESIAN_POINT('',(-0.00327887688297074,-0.00831259536819949,0.00693692275275569));
#25020=CARTESIAN_POINT('',(-0.00470755195860713,-0.00852930915460724,0.00605905256218031));
#25021=CARTESIAN_POINT('',(-0.00676215335210728,-0.0089627367274227,0.00362536740214226));
#25022=CARTESIAN_POINT('',(-0.00738807966997103,-0.00917945051383042,0.00206955243267961));
#25023=CARTESIAN_POINT('',(-0.00756105579906895,-0.00954620328144802,-0.000619321800270949));
#25024=CARTESIAN_POINT('',(-0.00738078795784222,-0.0096962422626579,-0.00173517934020447));
#25025=CARTESIAN_POINT('',(-0.00697636423659504,-0.00984628124386777,-0.00276215527904061));
#25026=CARTESIAN_POINT('',(0.00742674209415336,0.000371855266211312,-0.00043741976605035));
#25027=CARTESIAN_POINT('',(0.0074969734293519,0.000201812618092225,0.000800528324894085));
#25028=CARTESIAN_POINT('',(0.00725784950189997,3.17699699731351E-5,0.00205684184824264));
#25029=CARTESIAN_POINT('',(0.00605485985396608,-0.000354986464553727,0.00460399684621859));
#25030=CARTESIAN_POINT('',(0.00491008999420785,-0.0005717002509615,0.00580967416040846));
#25031=CARTESIAN_POINT('',(0.00212801615389771,-0.00100512782377705,0.00730314640404847));
#25032=CARTESIAN_POINT('',(0.00049071217334581,-0.00122184161018483,0.00759094133349861));
#25033=CARTESIAN_POINT('',(-0.00263391488201495,-0.0016552691830004,0.00713616576386437));
#25034=CARTESIAN_POINT('',(-0.00412123795682381,-0.00187198296940818,0.00639359526478));
#25035=CARTESIAN_POINT('',(-0.00636234658573735,-0.00230541054222375,0.00416933313820649));
#25036=CARTESIAN_POINT('',(-0.00711613213984203,-0.00252212432863154,0.00268764151071733));
#25037=CARTESIAN_POINT('',(-0.00759439713481167,-0.00295555190144711,-0.000433461001706967));
#25038=CARTESIAN_POINT('',(-0.00731887657567663,-0.0031722656878549,-0.00207287188664212));
#25039=CARTESIAN_POINT('',(-0.00584663683306912,-0.00360569326067047,-0.00486616680699417));
#25040=CARTESIAN_POINT('',(-0.00464991764959665,-0.00382240704707826,-0.00602005084241106));
#25041=CARTESIAN_POINT('',(-0.0018048361440574,-0.00425583461989383,-0.00738954105186203));
#25042=CARTESIAN_POINT('',(-0.000156473821990613,-0.00447254840630161,-0.00760514722589611));
#25043=CARTESIAN_POINT('',(0.00294512710098485,-0.00490597597911718,-0.00701348520662646));
#25044=CARTESIAN_POINT('',(0.00439836570189353,-0.00512268976552496,-0.00620621701332274));
#25045=CARTESIAN_POINT('',(0.00653951261541697,-0.00555611733834051,-0.00388555286234104));
#25046=CARTESIAN_POINT('',(0.00722742092803173,-0.00577283112474829,-0.00237215690466308));
#25047=CARTESIAN_POINT('',(0.00756799437922453,-0.00620625869756383,0.000766950627123334));
#25048=CARTESIAN_POINT('',(0.00722065951780256,-0.0064229724839716,0.00239266220123177));
#25049=CARTESIAN_POINT('',(0.00562702550518511,-0.00685640005678713,0.00511852883999097));
#25050=CARTESIAN_POINT('',(0.00438072635398963,-0.00707311384319489,0.00621868390464173));
#25051=CARTESIAN_POINT('',(0.00147819074810594,-0.0075065414160104,0.00746174341684272));
#25052=CARTESIAN_POINT('',(-0.000178045706582278,-0.00772325520241815,0.00760464786439295));
#25053=CARTESIAN_POINT('',(-0.00325066452296928,-0.00815668277523364,0.00687723555833265));
#25054=CARTESIAN_POINT('',(-0.00466704688466808,-0.00837339656164138,0.00600691880472212));
#25055=CARTESIAN_POINT('',(-0.00670396992175478,-0.00880682413445684,0.00359417374225892));
#25056=CARTESIAN_POINT('',(-0.0073245105971427,-0.00902353792086456,0.00205174543340624));
#25057=CARTESIAN_POINT('',(-0.00749599839197253,-0.00939029068848216,-0.000613992984883923));
#25058=CARTESIAN_POINT('',(-0.00731728162491385,-0.00954032966969203,-0.0017202493791354));
#25059=CARTESIAN_POINT('',(-0.0069163376767793,-0.0096903686509019,-0.00273838893407139));
#25060=CARTESIAN_POINT('',(0.00720667440087568,0.000592348969728383,-0.000424458233565662));
#25061=CARTESIAN_POINT('',(0.00727482465560353,0.000422306321609296,0.000776807234323083));
#25062=CARTESIAN_POINT('',(0.0070427863991571,0.000252263673490207,0.00199589393390264));
#25063=CARTESIAN_POINT('',(0.00587544349289022,-0.000134492761036654,0.00446757215919429));
#25064=CARTESIAN_POINT('',(0.00476459521801765,-0.000351206547444426,0.0056375230913438));
#25065=CARTESIAN_POINT('',(0.00206495921718051,-0.000784634120259979,0.00708674107282344));
#25066=CARTESIAN_POINT('',(0.000476171491215957,-0.00100134790666776,0.00736600812215358));
#25067=CARTESIAN_POINT('',(-0.00255586725830238,-0.00143477547948332,0.00692470836860393));
#25068=CARTESIAN_POINT('',(-0.00399911828185615,-0.0016514892658911,0.00620414156572414));
#25069=CARTESIAN_POINT('',(-0.00617381884110776,-0.00208491683870668,0.00404578831672229));
#25070=CARTESIAN_POINT('',(-0.0069052683768056,-0.00230163062511446,0.00260800187060023));
#25071=CARTESIAN_POINT('',(-0.00736936152187336,-0.00273505819793004,-0.000420616774512569));
#25072=CARTESIAN_POINT('',(-0.00710200513124326,-0.00295177198433782,-0.0020114489735033));
#25073=CARTESIAN_POINT('',(-0.00567339049369526,-0.0033851995571534,-0.00472197355364789));
#25074=CARTESIAN_POINT('',(-0.00451213224677736,-0.00360191334356118,-0.00584166593480174));
#25075=CARTESIAN_POINT('',(-0.00175135561087993,-0.00403534091637675,-0.00717057569221339));
#25076=CARTESIAN_POINT('',(-0.000151837221900407,-0.00425205470278453,-0.00737979306847119));
#25077=CARTESIAN_POINT('',(0.00285785770084859,-0.0046854822756001,-0.00680566305638989));
#25078=CARTESIAN_POINT('',(0.00426803423461806,-0.00490219606200788,-0.00602231566805079));
#25079=CARTESIAN_POINT('',(0.00634573512345747,-0.00533562363482344,-0.00377041695958807));
#25080=CARTESIAN_POINT('',(0.0070132594785274,-0.00555233742123121,-0.00230186563946444));
#25081=CARTESIAN_POINT('',(0.00734374112730596,-0.00598576499404675,0.000744224503982232));
#25082=CARTESIAN_POINT('',(0.0070066984210146,-0.00620247878045452,0.00232176332730528));
#25083=CARTESIAN_POINT('',(0.00546028664348213,-0.00663590635327005,0.00496685764682014));
#25084=CARTESIAN_POINT('',(0.00425091757224103,-0.00685262013967781,0.00603441314301194));
#25085=CARTESIAN_POINT('',(0.00143438930407625,-0.00728604771249332,0.00724063857157453));
#25086=CARTESIAN_POINT('',(-0.000172769892847421,-0.00750276149890108,0.00737930850394532));
#25087=CARTESIAN_POINT('',(-0.00315434150082575,-0.00793618907171656,0.00667345072963354));
#25088=CARTESIAN_POINT('',(-0.00452875391188042,-0.0081529028581243,0.00582892302295097));
#25089=CARTESIAN_POINT('',(-0.00650531926473991,-0.00858633043093976,0.00348767192562512));
#25090=CARTESIAN_POINT('',(-0.00710747220654474,-0.00880304421734749,0.00199094853498184));
#25091=CARTESIAN_POINT('',(-0.00727387851033112,-0.00916979698496509,-0.000595799271118275));
#25092=CARTESIAN_POINT('',(-0.00710045744173322,-0.00931983596617496,-0.00166927530356775));
#25093=CARTESIAN_POINT('',(-0.00671139418215376,-0.00946987494738482,-0.0026572455567495));
#25094=CARTESIAN_POINT('',(0.00705106304263895,0.000656930080279598,-0.00041529304605117));
#25095=CARTESIAN_POINT('',(0.00711774175125379,0.000486887432160511,0.000760033890323187));
#25096=CARTESIAN_POINT('',(0.0068907138208246,0.000316844784041421,0.00195279725037364));
#25097=CARTESIAN_POINT('',(0.00574857696731766,-6.99116504854405E-5,0.00437110533787815));
#25098=CARTESIAN_POINT('',(0.00466171487514634,-0.000286625436893213,0.00551579390301966));
#25099=CARTESIAN_POINT('',(0.00202037122962695,-0.000720053009708766,0.00693371939562929));
#25100=CARTESIAN_POINT('',(0.000465889676278861,-0.000936766796116546,0.00720695632309743));
#25101=CARTESIAN_POINT('',(-0.00250067925431972,-0.00137019436893211,0.00677518541048322));
#25102=CARTESIAN_POINT('',(-0.00391276663157022,-0.00158690815533989,0.00607017757040086));
#25103=CARTESIAN_POINT('',(-0.00604050959443837,-0.00202033572815547,0.00395842893567034));
#25104=CARTESIAN_POINT('',(-0.00675616518005603,-0.00223704951456325,0.00255168814102218));
#25105=CARTESIAN_POINT('',(-0.00721023731395619,-0.00267047708737882,-0.000411534534364309));
#25106=CARTESIAN_POINT('',(-0.00694865386223869,-0.00288719087378661,-0.00196801641510262));
#25107=CARTESIAN_POINT('',(-0.00555088683230826,-0.00332061844660218,-0.0046200135264054));
#25108=CARTESIAN_POINT('',(-0.00441470325409532,-0.00353733223300997,-0.00571552875696985));
#25109=CARTESIAN_POINT('',(-0.00171353916320867,-0.00397075980582554,-0.00701574380156087));
#25110=CARTESIAN_POINT('',(-0.000148558650534957,-0.00418747359223332,-0.00722044361558744));
#25111=CARTESIAN_POINT('',(0.00279614891622217,-0.00462090116504889,-0.00665871060467684));
#25112=CARTESIAN_POINT('',(0.00417587597030559,-0.00483761495145667,-0.00589227777973966));
#25113=CARTESIAN_POINT('',(0.00620871374485157,-0.00527104252427223,-0.00368900358199341));
#25114=CARTESIAN_POINT('',(0.00686182446531413,-0.00548775631068,-0.00225216220918432));
#25115=CARTESIAN_POINT('',(0.00718517013217121,-0.00592118388349554,0.000728154708199079));
#25116=CARTESIAN_POINT('',(0.00685540507856572,-0.00613789766990331,0.00227163025277339));
#25117=CARTESIAN_POINT('',(0.00534238446368462,-0.00657132524271884,0.00485960991761841));
#25118=CARTESIAN_POINT('',(0.004159128902409,-0.0067880390291266,0.00590411403788912));
#25119=CARTESIAN_POINT('',(0.00140341700597708,-0.00722146660194211,0.00708429383613219));
#25120=CARTESIAN_POINT('',(-0.000169039329179231,-0.00743818038834986,0.00721996951410456));
#25121=CARTESIAN_POINT('',(-0.00308623083868367,-0.00787160796116534,0.00652935309535745));
#25122=CARTESIAN_POINT('',(-0.00443096601303181,-0.00808832174757308,0.00570306099863799));
#25123=CARTESIAN_POINT('',(-0.00636485203807753,-0.00852174932038855,0.00341236376887466));
#25124=CARTESIAN_POINT('',(-0.00695400288877511,-0.00873846310679627,0.0019479586358308));
#25125=CARTESIAN_POINT('',(-0.00711681603578613,-0.00910521587441387,-0.000582934372739653));
#25126=CARTESIAN_POINT('',(-0.00694713959148096,-0.00925525485562374,-0.00163323118906917));
#25127=CARTESIAN_POINT('',(-0.00656647724734397,-0.00940529383683361,-0.00259986852439682));
#25128=CARTESIAN_POINT('',(0.00673984032616548,0.000656930080279598,-0.000396962671022186));
#25129=CARTESIAN_POINT('',(0.00680357594255429,0.000486887432160511,0.000726487202323393));
#25130=CARTESIAN_POINT('',(0.00658656866415959,0.000316844784041421,0.00186660388331565));
#25131=CARTESIAN_POINT('',(0.00549484391617253,-6.99116504854403E-5,0.00417817169524589));
#25132=CARTESIAN_POINT('',(0.00445595418940373,-0.000286625436893212,0.00527233552637138));
#25133=CARTESIAN_POINT('',(0.00193119525451979,-0.000720053009708766,0.00662767604124101));
#25134=CARTESIAN_POINT('',(0.000445326046404666,-0.000936766796116546,0.00688885272498515));
#25135=CARTESIAN_POINT('',(-0.00239030324635441,-0.00137019436893211,0.0064761394942418));
#25136=CARTESIAN_POINT('',(-0.00374006333099836,-0.00158690815533989,0.00580224957975431));
#25137=CARTESIAN_POINT('',(-0.00577389110109959,-0.00202033572815547,0.00378371017356644));
#25138=CARTESIAN_POINT('',(-0.00645795878655688,-0.00223704951456325,0.00243906068186606));
#25139=CARTESIAN_POINT('',(-0.00689198889812187,-0.00267047708737883,-0.000393370054067794));
#25140=CARTESIAN_POINT('',(-0.00664195132422956,-0.00288719087378661,-0.00188115129830126));
#25141=CARTESIAN_POINT('',(-0.00530587950953425,-0.00332061844660218,-0.0044160934719204));
#25142=CARTESIAN_POINT('',(-0.00421984526873124,-0.00353733223300997,-0.00546325440130608));
#25143=CARTESIAN_POINT('',(-0.00163790626786615,-0.00397075980582554,-0.00670608002025585));
#25144=CARTESIAN_POINT('',(-0.000142001507804063,-0.00418747359223332,-0.00690174470981995));
#25145=CARTESIAN_POINT('',(0.00267273134696934,-0.00462090116504889,-0.00636480570125073));
#25146=CARTESIAN_POINT('',(0.00399155944168066,-0.00483761495145667,-0.00563220200311741));
#25147=CARTESIAN_POINT('',(0.00593467098763978,-0.00527104252427223,-0.00352617682680408));
#25148=CARTESIAN_POINT('',(0.0065589544388876,-0.00548775631068,-0.00215275534862407));
#25149=CARTESIAN_POINT('',(0.00686802814190169,-0.00592118388349554,0.000696015116632777));
#25150=CARTESIAN_POINT('',(0.00655281839366796,-0.00613789766990331,0.0021713641037096));
#25151=CARTESIAN_POINT('',(0.0051065801040896,-0.00657132524271884,0.00464511445921495));
#25152=CARTESIAN_POINT('',(0.00397555156274497,-0.0067880390291266,0.00564351582764347));
#25153=CARTESIAN_POINT('',(0.00134147240977874,-0.00722146660194211,0.00677160436524751));
#25154=CARTESIAN_POINT('',(-0.000161578201842847,-0.00743818038834986,0.00690129153442303));
#25155=CARTESIAN_POINT('',(-0.00295000951439953,-0.00787160796116534,0.0062411578268053));
#25156=CARTESIAN_POINT('',(-0.00423539021533461,-0.00808832174757308,0.00545133695001203));
#25157=CARTESIAN_POINT('',(-0.00608391758475277,-0.00852174932038855,0.00326174745537375));
#25158=CARTESIAN_POINT('',(-0.00664706425323584,-0.00873846310679627,0.00186197883752873));
#25159=CARTESIAN_POINT('',(-0.00680269108669614,-0.00910521587441387,-0.000557204575982392));
#25160=CARTESIAN_POINT('',(-0.00664050389097645,-0.00925525485562374,-0.00156114296007199));
#25161=CARTESIAN_POINT('',(-0.0062766433777244,-0.00940529383683361,-0.00248511445969145));
#25162=CARTESIAN_POINT('',(0.00658422896792875,0.000592348969728383,-0.000387797483507693));
#25163=CARTESIAN_POINT('',(0.00664649303820454,0.000422306321609297,0.000709713858323498));
#25164=CARTESIAN_POINT('',(0.00643449608582708,0.000252263673490207,0.00182350719978666));
#25165=CARTESIAN_POINT('',(0.00536797739059997,-0.000134492761036653,0.00408170487392976));
#25166=CARTESIAN_POINT('',(0.00435307384653242,-0.000351206547444425,0.00515060633804724));
#25167=CARTESIAN_POINT('',(0.00188660726696621,-0.000784634120259978,0.00647465436404687));
#25168=CARTESIAN_POINT('',(0.000435044231467567,-0.00100134790666776,0.00672980092592901));
#25169=CARTESIAN_POINT('',(-0.00233511524237175,-0.00143477547948332,0.00632661653612109));
#25170=CARTESIAN_POINT('',(-0.00365371168071242,-0.0016514892658911,0.00566828558443103));
#25171=CARTESIAN_POINT('',(-0.0056405818544302,-0.00208491683870668,0.00369635079251449));
#25172=CARTESIAN_POINT('',(-0.00630885558980731,-0.00230163062511446,0.00238274695228799));
#25173=CARTESIAN_POINT('',(-0.00673286469020471,-0.00273505819793004,-0.000384287813919537));
#25174=CARTESIAN_POINT('',(-0.00648860005522499,-0.00295177198433782,-0.00183771873990058));
#25175=CARTESIAN_POINT('',(-0.00518337584814724,-0.0033851995571534,-0.00431413344467791));
#25176=CARTESIAN_POINT('',(-0.00412241627604921,-0.00360191334356118,-0.00533711722347419));
#25177=CARTESIAN_POINT('',(-0.0016000898201949,-0.00403534091637675,-0.00655124812960334));
#25178=CARTESIAN_POINT('',(-0.000138722936438619,-0.00425205470278453,-0.00674239525693621));
#25179=CARTESIAN_POINT('',(0.00261102256234292,-0.0046854822756001,-0.00621785324953768));
#25180=CARTESIAN_POINT('',(0.00389940117736819,-0.00490219606200788,-0.00550216411480628));
#25181=CARTESIAN_POINT('',(0.0057976496090339,-0.00533562363482344,-0.00344476344920941));
#25182=CARTESIAN_POINT('',(0.00640751942567434,-0.00555233742123121,-0.00210305191834393));
#25183=CARTESIAN_POINT('',(0.00670945714676693,-0.00598576499404675,0.000679945320849626));
#25184=CARTESIAN_POINT('',(0.00640152505121908,-0.00620247878045452,0.00212123102917771));
#25185=CARTESIAN_POINT('',(0.00498867792429209,-0.00663590635327005,0.00453786673001321));
#25186=CARTESIAN_POINT('',(0.00388376289291295,-0.00685262013967781,0.00551321672252064));
#25187=CARTESIAN_POINT('',(0.00131050011167958,-0.00728604771249332,0.00661525962980517));
#25188=CARTESIAN_POINT('',(-0.000157847638174654,-0.00750276149890107,0.00674195254458227));
#25189=CARTESIAN_POINT('',(-0.00288189885225745,-0.00793618907171656,0.00609706019252921));
#25190=CARTESIAN_POINT('',(-0.00413760231648601,-0.0081529028581243,0.00532547492569905));
#25191=CARTESIAN_POINT('',(-0.00594345035809039,-0.00858633043093976,0.0031864392986233));
#25192=CARTESIAN_POINT('',(-0.00649359493546621,-0.00880304421734749,0.00181898893837771));
#25193=CARTESIAN_POINT('',(-0.00664562861215114,-0.00916979698496509,-0.000544339677603755));
#25194=CARTESIAN_POINT('',(-0.0064871860407242,-0.00931983596617496,-0.0015250988455734));
#25195=CARTESIAN_POINT('',(-0.00613172644291462,-0.00946987494738482,-0.00242773742733876));
#25196=CARTESIAN_POINT('',(0.00636416127465107,0.000371855266211312,-0.000374835951023005));
#25197=CARTESIAN_POINT('',(0.00642434426445617,0.000201812618092225,0.000685992767752494));
#25198=CARTESIAN_POINT('',(0.00621943298308421,3.17699699731348E-5,0.00176255928544665));
#25199=CARTESIAN_POINT('',(0.0051885610295241,-0.000354986464553727,0.00394528018690546));
#25200=CARTESIAN_POINT('',(0.00420757907034223,-0.0005717002509615,0.00497845526898257));
#25201=CARTESIAN_POINT('',(0.00182355033024902,-0.00100512782377705,0.00625824903282183));
#25202=CARTESIAN_POINT('',(0.000420503549337712,-0.00122184161018483,0.00650486771458397));
#25203=CARTESIAN_POINT('',(-0.00225706761865918,-0.0016552691830004,0.00611515914086064));
#25204=CARTESIAN_POINT('',(-0.00353159200574477,-0.00187198296940818,0.00547883188537516));
#25205=CARTESIAN_POINT('',(-0.00545205410980061,-0.00230541054222375,0.00357280597103028));
#25206=CARTESIAN_POINT('',(-0.00609799182677088,-0.00252212432863154,0.00230310731217089));
#25207=CARTESIAN_POINT('',(-0.00650782907726638,-0.00295555190144711,-0.00037144358672514));
#25208=CARTESIAN_POINT('',(-0.00627172861079161,-0.0031722656878549,-0.00177629582676177));
#25209=CARTESIAN_POINT('',(-0.00501012950877337,-0.00360569326067047,-0.00416994019133164));
#25210=CARTESIAN_POINT('',(-0.00398463087322989,-0.00382240704707826,-0.00515873231586488));
#25211=CARTESIAN_POINT('',(-0.0015466092870174,-0.00425583461989383,-0.0063322827699547));
#25212=CARTESIAN_POINT('',(-0.000134086336348388,-0.00447254840630161,-0.00651704109951128));
#25213=CARTESIAN_POINT('',(0.00252375316220668,-0.00490597597911718,-0.0060100310993011));
#25214=CARTESIAN_POINT('',(0.00376906971009273,-0.00512268976552496,-0.00531826276953433));
#25215=CARTESIAN_POINT('',(0.00560387211707439,-0.00555611733834051,-0.00332962754645643));
#25216=CARTESIAN_POINT('',(0.00619335797617,-0.00577283112474829,-0.00203276065314531));
#25217=CARTESIAN_POINT('',(0.00648520389484837,-0.00620625869756383,0.000657219197708529));
#25218=CARTESIAN_POINT('',(0.00618756395443112,-0.0064229724839716,0.00205033215525123));
#25219=CARTESIAN_POINT('',(0.0048219390625891,-0.00685640005678713,0.00438619553684241));
#25220=CARTESIAN_POINT('',(0.00375395411116433,-0.00707311384319489,0.00532894596089087));
#25221=CARTESIAN_POINT('',(0.00126669866764988,-0.0075065414160104,0.00639415478453698));
#25222=CARTESIAN_POINT('',(-0.000152571824439798,-0.00772325520241815,0.00651661318413464));
#25223=CARTESIAN_POINT('',(-0.00278557583011391,-0.00815668277523364,0.0058932753638301));
#25224=CARTESIAN_POINT('',(-0.00399930934369835,-0.00837339656164138,0.00514747914392789));
#25225=CARTESIAN_POINT('',(-0.00574479970107553,-0.00880682413445684,0.00307993748198948));
#25226=CARTESIAN_POINT('',(-0.00627655654486826,-0.00902353792086456,0.00175819203995327));
#25227=CARTESIAN_POINT('',(-0.00642350873050973,-0.00939029068848216,-0.000526145963838135));
#25228=CARTESIAN_POINT('',(-0.00627036185754357,-0.00954032966969203,-0.00147412477000577));
#25229=CARTESIAN_POINT('',(-0.00592678294828908,-0.0096903686509019,-0.00234659405001688));
#25230=CARTESIAN_POINT('',(0.00629970493961011,0.000215942673245455,-0.00037103960605281));
#25231=CARTESIAN_POINT('',(0.00635927839505755,4.59000251263669E-5,0.000679045021181388));
#25232=CARTESIAN_POINT('',(0.00615644245867384,-0.000124142622992724,0.00174470805463564));
#25233=CARTESIAN_POINT('',(0.00513601119402079,-0.000510899057519587,0.00390532232119729));
#25234=CARTESIAN_POINT('',(0.00416496463702333,-0.000727612843927361,0.00492803338824205));
#25235=CARTESIAN_POINT('',(0.00180508138108541,-0.00116104041674292,0.00619486537879095));
#25236=CARTESIAN_POINT('',(0.000416244682144955,-0.0013777542031507,0.00643898630229508));
#25237=CARTESIAN_POINT('',(-0.00223420799892928,-0.00181118177596627,0.00605322470372089));
#25238=CARTESIAN_POINT('',(-0.00349582398106305,-0.00202789556237404,0.00542334218164256));
#25239=CARTESIAN_POINT('',(-0.00539683561184042,-0.00246132313518961,0.00353662053059804));
#25240=CARTESIAN_POINT('',(-0.00603623126048403,-0.0026780369215974,0.00227978140163184));
#25241=CARTESIAN_POINT('',(-0.00644191767224522,-0.00311146449441298,-0.000367681599679002));
#25242=CARTESIAN_POINT('',(-0.0062082084353628,-0.00332817828082076,-0.00175830547202365));
#25243=CARTESIAN_POINT('',(-0.0049593868307865,-0.00376160585363634,-0.00412770696522788));
#25244=CARTESIAN_POINT('',(-0.00394427446309262,-0.00397831964004412,-0.00510648458608746));
#25245=CARTESIAN_POINT('',(-0.00153094520151117,-0.00441174721285968,-0.00626814930095857));
#25246=CARTESIAN_POINT('',(-0.0001327283076236,-0.00462846099926747,-0.00645103639497011));
#25247=CARTESIAN_POINT('',(0.00249819254669685,-0.00506188857208303,-0.00594916140077757));
#25248=CARTESIAN_POINT('',(0.00373089650712975,-0.00527860235849082,-0.0052643993125735));
#25249=CARTESIAN_POINT('',(0.00554711600372078,-0.00571202993130638,-0.00329590502129811));
#25250=CARTESIAN_POINT('',(0.00613063153987892,-0.00592874371771416,-0.00201217281822681));
#25251=CARTESIAN_POINT('',(0.00641952163806455,-0.0063621712905297,0.000650562870350582));
#25252=CARTESIAN_POINT('',(0.00612489620009204,-0.00657888507693745,0.00202956635585666));
#25253=CARTESIAN_POINT('',(0.00477310238068363,-0.00701231264975299,0.00434177207287334));
#25254=CARTESIAN_POINT('',(0.00371593399924772,-0.00722902643616076,0.00527497430438392));
#25255=CARTESIAN_POINT('',(0.00125386952171934,-0.00766245400897627,0.00632939467471113));
#25256=CARTESIAN_POINT('',(-0.000151026574373135,-0.00787916779538401,0.00645061281352776));
#25257=CARTESIAN_POINT('',(-0.00275736347011246,-0.0083125953681995,0.00583358816940705));
#25258=CARTESIAN_POINT('',(-0.0039588042697593,-0.00852930915460724,0.00509534538646971));
#25259=CARTESIAN_POINT('',(-0.00568661627072304,-0.0089627367274227,0.00304874382210612));
#25260=CARTESIAN_POINT('',(-0.00621298747203994,-0.00917945051383042,0.00174038504067986));
#25261=CARTESIAN_POINT('',(-0.00635845132341332,-0.00954620328144802,-0.000520817148451154));
#25262=CARTESIAN_POINT('',(-0.0062068555246152,-0.00969624226265789,-0.00145919480893673));
#25263=CARTESIAN_POINT('',(-0.00586675638847333,-0.00984628124386776,-0.00232282770504767));
#25264=CARTESIAN_POINT('',(0.00629970493961011,5.62796276089674E-5,-0.000371039606052811));
#25265=CARTESIAN_POINT('',(0.00635927839505755,-0.000113763020510121,0.000679045021181388));
#25266=CARTESIAN_POINT('',(0.00615644245867384,-0.000283805668629212,0.00174470805463564));
#25267=CARTESIAN_POINT('',(0.00513601119402079,-0.000670562103156075,0.00390532232119729));
#25268=CARTESIAN_POINT('',(0.00416496463702333,-0.000887275889563849,0.00492803338824204));
#25269=CARTESIAN_POINT('',(0.00180508138108541,-0.00132070346237941,0.00619486537879094));
#25270=CARTESIAN_POINT('',(0.000416244682144954,-0.00153741724878719,0.00643898630229508));
#25271=CARTESIAN_POINT('',(-0.00223420799892927,-0.00197084482160275,0.0060532247037209));
#25272=CARTESIAN_POINT('',(-0.00349582398106304,-0.00218755860801054,0.00542334218164257));
#25273=CARTESIAN_POINT('',(-0.00539683561184041,-0.00262098618082611,0.00353662053059805));
#25274=CARTESIAN_POINT('',(-0.00603623126048402,-0.00283769996723389,0.00227978140163185));
#25275=CARTESIAN_POINT('',(-0.00644191767224522,-0.00327112754004947,-0.000367681599679004));
#25276=CARTESIAN_POINT('',(-0.00620820843536279,-0.00348784132645725,-0.00175830547202365));
#25277=CARTESIAN_POINT('',(-0.00495938683078651,-0.00392126889927283,-0.00412770696522788));
#25278=CARTESIAN_POINT('',(-0.00394427446309264,-0.00413798268568061,-0.00510648458608745));
#25279=CARTESIAN_POINT('',(-0.00153094520151119,-0.00457141025849618,-0.00626814930095856));
#25280=CARTESIAN_POINT('',(-0.000132728307623607,-0.00478812404490397,-0.00645103639497011));
#25281=CARTESIAN_POINT('',(0.00249819254669686,-0.00522155161771953,-0.00594916140077758));
#25282=CARTESIAN_POINT('',(0.00373089650712975,-0.00543826540412731,-0.0052643993125735));
#25283=CARTESIAN_POINT('',(0.00554711600372077,-0.00587169297694287,-0.00329590502129811));
#25284=CARTESIAN_POINT('',(0.00613063153987892,-0.00608840676335064,-0.00201217281822681));
#25285=CARTESIAN_POINT('',(0.00641952163806455,-0.00652183433616618,0.000650562870350582));
#25286=CARTESIAN_POINT('',(0.00612489620009204,-0.00673854812257395,0.00202956635585666));
#25287=CARTESIAN_POINT('',(0.00477310238068363,-0.00717197569538948,0.00434177207287333));
#25288=CARTESIAN_POINT('',(0.00371593399924772,-0.00738868948179724,0.00527497430438391));
#25289=CARTESIAN_POINT('',(0.00125386952171934,-0.00782211705461275,0.00632939467471113));
#25290=CARTESIAN_POINT('',(-0.000151026574373135,-0.0080388308410205,0.00645061281352777));
#25291=CARTESIAN_POINT('',(-0.00275736347011246,-0.00847225841383599,0.00583358816940706));
#25292=CARTESIAN_POINT('',(-0.0039588042697593,-0.00868897220024372,0.00509534538646972));
#25293=CARTESIAN_POINT('',(-0.00568661627072304,-0.00912239977305918,0.00304874382210612));
#25294=CARTESIAN_POINT('',(-0.00621298747203993,-0.00933911355946691,0.00174038504067986));
#25295=CARTESIAN_POINT('',(-0.00635845132341332,-0.0097058663270845,-0.000520817148451154));
#25296=CARTESIAN_POINT('',(-0.00620685552461521,-0.00985590530829437,-0.00145919480893672));
#25297=CARTESIAN_POINT('',(-0.00586675638847333,-0.0100059442895042,-0.00232282770504767));
#25298=CARTESIAN_POINT('',(0.00629974223632648,5.25291749383375E-5,-0.000371041802752352));
#25299=CARTESIAN_POINT('',(0.00635931604447206,-0.000117513473180751,0.000679049041393414));
#25300=CARTESIAN_POINT('',(0.0061564789072203,-0.000287556121299842,0.00174471838398949));
#25301=CARTESIAN_POINT('',(0.00513604160121519,-0.000674312555826705,0.00390534544223238));
#25302=CARTESIAN_POINT('',(0.00416498929524245,-0.000891026342234479,0.00492806256412651));
#25303=CARTESIAN_POINT('',(0.00180509206787296,-0.00132445391505004,0.00619490205481612));
#25304=CARTESIAN_POINT('',(0.00041624714647622,-0.00154116770145782,0.00643902442361157));
#25305=CARTESIAN_POINT('',(-0.00223422122631418,-0.00197459527427338,0.0060532605411779));
#25306=CARTESIAN_POINT('',(-0.00349584467770784,-0.00219130906068117,0.00542337428994876));
#25307=CARTESIAN_POINT('',(-0.00539686756321734,-0.00262473663349674,0.00353664146877437));
#25308=CARTESIAN_POINT('',(-0.00603626699733319,-0.00284145041990452,0.00227979489882912));
#25309=CARTESIAN_POINT('',(-0.00644195581091657,-0.0032748779927201,-0.000367683776497834));
#25310=CARTESIAN_POINT('',(-0.00620824519038408,-0.00349159177912788,-0.00175831588187953));
#25311=CARTESIAN_POINT('',(-0.00495941619229562,-0.00392501935194346,-0.004127731402867));
#25312=CARTESIAN_POINT('',(-0.00394429781473964,-0.00414173313835124,-0.00510651481847279));
#25313=CARTESIAN_POINT('',(-0.00153095426530537,-0.00457516071116681,-0.00626818641085321));
#25314=CARTESIAN_POINT('',(-0.000132729093427084,-0.0047918744975746,-0.00645107458762786));
#25315=CARTESIAN_POINT('',(0.00249820733697351,-0.00522530207039016,-0.00594919662213914));
#25316=CARTESIAN_POINT('',(0.00373091859549582,-0.00544201585679794,-0.00526443047987576));
#25317=CARTESIAN_POINT('',(0.00554714884481638,-0.0058754434296135,-0.00329592453434451));
#25318=CARTESIAN_POINT('',(0.00613066783561465,-0.00609215721602127,-0.00201218473107663));
#25319=CARTESIAN_POINT('',(0.00641955964414262,-0.00652558478883681,0.000650566721937138));
#25320=CARTESIAN_POINT('',(0.00612493246187232,-0.00674229857524458,0.00202957837168303));
#25321=CARTESIAN_POINT('',(0.00477313063931596,-0.00717572614806011,0.00434179777786159));
#25322=CARTESIAN_POINT('',(0.00371595599902989,-0.00739243993446787,0.00527500553429426));
#25323=CARTESIAN_POINT('',(0.00125387694511716,-0.00782586750728338,0.00632943214720234));
#25324=CARTESIAN_POINT('',(-0.000151027468509505,-0.00804258129369113,0.00645065100367775));
#25325=CARTESIAN_POINT('',(-0.0027573797947823,-0.00847600886650662,0.0058336227065299));
#25326=CARTESIAN_POINT('',(-0.00395882770742843,-0.00869272265291435,0.00509537555290664));
#25327=CARTESIAN_POINT('',(-0.00568664993771477,-0.00912615022572981,0.00304876187186157));
#25328=CARTESIAN_POINT('',(-0.00621302425535498,-0.00934286401213754,0.00174039534443977));
#25329=CARTESIAN_POINT('',(-0.00635848896793125,-0.00970961677975513,-0.000520820231892307));
#25330=CARTESIAN_POINT('',(-0.00620689227162673,-0.009859655760965,-0.00145920344794052));
#25331=CARTESIAN_POINT('',(-0.005866791121965,-0.0100096947421749,-0.00232284145709589));
#25332=CARTESIAN_POINT('',(0.0062998165669852,4.87793578883542E-5,-0.000371046180674587));
#25333=CARTESIAN_POINT('',(0.00635939107804215,-0.000121263290230734,0.000679057053493061));
#25334=CARTESIAN_POINT('',(0.00615655154751501,-0.000291305938349825,0.00174473896992172));
#25335=CARTESIAN_POINT('',(0.0051361022013701,-0.000678062372876689,0.0039053915214033));
#25336=CARTESIAN_POINT('',(0.00416503843795119,-0.000894776159284463,0.00492812071033677));
#25337=CARTESIAN_POINT('',(0.00180511336615429,-0.00132820373210002,0.00619497514846554));
#25338=CARTESIAN_POINT('',(0.000416252057776306,-0.0015449175185078,0.00643910039766082));
#25339=CARTESIAN_POINT('',(-0.00223424758789045,-0.00197834509132337,0.0060533319635991));
#25340=CARTESIAN_POINT('',(-0.00349588592517923,-0.00219505887773115,0.00542343828034207));
#25341=CARTESIAN_POINT('',(-0.00539693124085779,-0.00262848645054672,0.00353668319760711));
#25342=CARTESIAN_POINT('',(-0.00603633821924757,-0.0028452002369545,0.00227982179812916));
#25343=CARTESIAN_POINT('',(-0.00644203181955326,-0.00327862780977008,-0.000367688114798717));
#25344=CARTESIAN_POINT('',(-0.00620831844146915,-0.00349534159617787,-0.00175833662824864));
#25345=CARTESIAN_POINT('',(-0.00495947470844733,-0.00392876916899344,-0.00412778010596988));
#25346=CARTESIAN_POINT('',(-0.0039443443535096,-0.00414548295540122,-0.00510657507024119));
#25347=CARTESIAN_POINT('',(-0.00153097232903477,-0.00457891052821679,-0.00626826036918475));
#25348=CARTESIAN_POINT('',(-0.000132730659497659,-0.00479562431462458,-0.006451150703857));
#25349=CARTESIAN_POINT('',(0.00249823681332191,-0.00522905188744014,-0.00594926681671015));
#25350=CARTESIAN_POINT('',(0.00373096261660437,-0.00544576567384792,-0.00526449259489105));
#25351=CARTESIAN_POINT('',(0.00554721429562567,-0.00587919324666348,-0.00329596342295813));
#25352=CARTESIAN_POINT('',(0.00613074017136452,-0.00609590703307125,-0.0020122084728443));
#25353=CARTESIAN_POINT('',(0.00641963538852694,-0.00652933460588679,0.000650574397973898));
#25354=CARTESIAN_POINT('',(0.00612500472995051,-0.00674604839229456,0.00202960231867826));
#25355=CARTESIAN_POINT('',(0.00477318695748443,-0.00717947596511009,0.00434184900673363));
#25356=CARTESIAN_POINT('',(0.00371599984359477,-0.00739618975151785,0.00527506777408462));
#25357=CARTESIAN_POINT('',(0.00125389173961125,-0.00782961732433336,0.00632950682817232));
#25358=CARTESIAN_POINT('',(-0.000151029250482608,-0.00804633111074111,0.00645072711490902));
#25359=CARTESIAN_POINT('',(-0.00275741232910654,-0.0084797586835566,0.00583369153744429));
#25360=CARTESIAN_POINT('',(-0.0039588744176366,-0.00869647246996433,0.00509543567324285));
#25361=CARTESIAN_POINT('',(-0.00568671703449746,-0.00912990004277979,0.00304879784420294));
#25362=CARTESIAN_POINT('',(-0.00621309756282825,-0.00934661382918752,0.00174041587936446));
#25363=CARTESIAN_POINT('',(-0.00635856399174266,-0.00971336659680511,-0.000520826377050229));
#25364=CARTESIAN_POINT('',(-0.00620696550674872,-0.00986340557801498,-0.00145922066508202));
#25365=CARTESIAN_POINT('',(-0.00586686034423352,-0.0100134445592248,-0.00232286886430227));
#25366=CARTESIAN_POINT('',(0.00750327656949163,-8.53080492016359E-9,5.83924176101713E-10));
#25367=CARTESIAN_POINT('',(0.00750328356622613,0.000155908244795296,8.91110510665626E-10));
#25368=CARTESIAN_POINT('',(0.00737416840995134,0.000467747108013051,1.49443482527523E-9));
#25369=CARTESIAN_POINT('',(0.00690656929314086,0.000661501357346462,2.2553121146952E-9));
#25370=CARTESIAN_POINT('',(0.0064389701765613,0.000467746857475072,2.88847076502633E-9));
#25371=CARTESIAN_POINT('',(0.00630985502057318,0.000155907827228039,3.33264413512018E-9));
#25372=CARTESIAN_POINT('',(0.006309862017394,-9.03188821051637E-9,3.5909752516927E-9));
#25373=CARTESIAN_POINT('',(-0.00600466497160202,0.00989161658584234,0.00195123602046633));
#25374=CARTESIAN_POINT('',(-0.00574414092335559,0.010028972165006,0.00275296354617664));
#25375=CARTESIAN_POINT('',(-0.00532095763677864,0.0101627934786023,0.00350161061675348));
#25376=CARTESIAN_POINT('',(-0.00421610368672497,0.0104233675746601,0.00477472643696357));
#25377=CARTESIAN_POINT('',(-0.00353443302324826,0.0105501203571216,0.00529919518659681));
#25378=CARTESIAN_POINT('',(-0.00202056207538,0.0107965573909099,0.00604079260745369));
#25379=CARTESIAN_POINT('',(-0.00118836179098845,0.0109162416422367,0.00625792127867733));
#25380=CARTESIAN_POINT('',(0.000494835703082955,0.0111485416137555,0.00635050111591244));
#25381=CARTESIAN_POINT('',(0.00134583291276282,0.0112611573339475,0.00622595228192391));
#25382=CARTESIAN_POINT('',(0.0029319010653021,0.0114793202431967,0.00565488463000731));
#25383=CARTESIAN_POINT('',(0.00366697200816151,0.0115848674322539,0.00520836581207923));
#25384=CARTESIAN_POINT('',(0.00490482050632797,0.0117888932792336,0.00406404847997765));
#25385=CARTESIAN_POINT('',(0.00540759806163502,0.0118873719371561,0.00336624996580416));
#25386=CARTESIAN_POINT('',(0.00610126561429382,0.0120772607218663,0.00182983996835635));
#25387=CARTESIAN_POINT('',(0.00629215561164556,0.012168670848654,0.000991228485082042));
#25388=CARTESIAN_POINT('',(0.00633182860310908,0.0123444225710946,-0.000694047966501003));
#25389=CARTESIAN_POINT('',(0.00618061159722085,0.0124287641667475,-0.00154071293480974));
#25390=CARTESIAN_POINT('',(0.00556000950518228,0.0125903788269186,-0.00310806215598619));
#25391=CARTESIAN_POINT('',(0.00509062441903194,0.0126676518914367,-0.00382874640885392));
#25392=CARTESIAN_POINT('',(0.00390799378434807,0.0128151294893382,-0.00503004381017692));
#25393=CARTESIAN_POINT('',(0.00319474823581453,0.0128853340227216,-0.00551065695863221));
#25394=CARTESIAN_POINT('',(0.00163730957094308,0.0130186745583536,-0.00615572684557856));
#25395=CARTESIAN_POINT('',(0.000793116454605152,0.0130818105606022,-0.00632018358406963));
#25396=CARTESIAN_POINT('',(-0.000892574732320377,0.0132010140339646,-0.00630690641188717));
#25397=CARTESIAN_POINT('',(-0.00173407280290798,0.0132570815050784,-0.00612917250121364));
#25398=CARTESIAN_POINT('',(-0.0032811564713131,0.0133621479161712,-0.0054596483638267));
#25399=CARTESIAN_POINT('',(-0.00398674206913061,0.0134111468561502,-0.00496785813711329));
#25400=CARTESIAN_POINT('',(-0.0051503049186267,0.0135020762049735,-0.00374808507395191));
#25401=CARTESIAN_POINT('',(-0.00560828217030528,0.0135440066138177,-0.00302010223750393));
#25402=CARTESIAN_POINT('',(-0.00620411058405509,0.0136207989003714,-0.00144315566807725));
#25403=CARTESIAN_POINT('',(-0.00634196174612631,0.0136556607780809,-0.000594191935098553));
#25404=CARTESIAN_POINT('',(-0.00627577492760283,0.013718316002365,0.00109019087403818));
#25405=CARTESIAN_POINT('',(-0.00607173694700813,0.0137461093489396,0.00192560995019621));
#25406=CARTESIAN_POINT('',(-0.00571279299028783,0.0137703684299469,0.0026883674746708));
#25407=CARTESIAN_POINT('',(-0.00600350244213178,0.00990699069817707,0.00195085825261618));
#25408=CARTESIAN_POINT('',(-0.00574302883248355,0.0100443462773407,0.00275243056036176));
#25409=CARTESIAN_POINT('',(-0.00531992747604663,0.010178167590937,0.00350093268958277));
#25410=CARTESIAN_POINT('',(-0.00421528743056271,0.0104387416869948,0.00477380202898718));
#25411=CARTESIAN_POINT('',(-0.00353374874151571,0.0105654944694564,0.00529816923917059));
#25412=CARTESIAN_POINT('',(-0.0020201708857016,0.0108119315032447,0.00603962308351473));
#25413=CARTESIAN_POINT('',(-0.0011881317189345,0.0109316157545714,0.00625670971767546));
#25414=CARTESIAN_POINT('',(0.000494739900720878,0.0111639157260902,0.0063492716310481));
#25415=CARTESIAN_POINT('',(0.00134557235360914,0.0112765314462822,0.00622474691026));
#25416=CARTESIAN_POINT('',(0.00293133343639884,0.0114946943555314,0.00565378981954506));
#25417=CARTESIAN_POINT('',(0.00366626206630027,0.0116002415445887,0.00520735744961822));
#25418=CARTESIAN_POINT('',(0.00490387091156926,0.0118042673915684,0.00406326166237021));
#25419=CARTESIAN_POINT('',(0.00540655112693682,0.0119027460494908,0.00336559824504905));
#25420=CARTESIAN_POINT('',(0.00610008438251554,0.012092634834201,0.00182948570331425));
#25421=CARTESIAN_POINT('',(0.0062909374227267,0.0121840449609887,0.000991036578900582));
#25422=CARTESIAN_POINT('',(0.0063306027333251,0.0123597966834293,-0.00069391359577114));
#25423=CARTESIAN_POINT('',(0.00617941500371233,0.0124441382790822,-0.0015404146460292));
#25424=CARTESIAN_POINT('',(0.00555893306296025,0.0126057529392533,-0.00310746042152328));
#25425=CARTESIAN_POINT('',(0.00508963885182094,0.0126830260037714,-0.0038280051467593));
#25426=CARTESIAN_POINT('',(0.00390723717961403,0.012830503601673,-0.00502906997163746));
#25427=CARTESIAN_POINT('',(0.00319412971854643,0.0129007081350563,-0.00550959007127961));
#25428=CARTESIAN_POINT('',(0.00163699258063019,0.0130340486706883,-0.00615453506986708));
#25429=CARTESIAN_POINT('',(0.000792962903781556,0.0130971846729369,-0.0063189599688124));
#25430=CARTESIAN_POINT('',(-0.000892401925938069,0.0132163881462993,-0.0063056853671487));
#25431=CARTESIAN_POINT('',(-0.00173373707880906,0.0132724556174131,-0.00612798586653968));
#25432=CARTESIAN_POINT('',(-0.00328052122503168,0.0133775220285059,-0.00545859135196174));
#25433=CARTESIAN_POINT('',(-0.00398597021838331,0.013426520968485,-0.00496689633799283));
#25434=CARTESIAN_POINT('',(-0.00514930779700927,0.0135174503173082,-0.00374735942824544));
#25435=CARTESIAN_POINT('',(-0.0056071963822836,0.0135593807261525,-0.00301951753246696));
#25436=CARTESIAN_POINT('',(-0.00620290944103967,0.0136361730127061,-0.00144287626681137));
#25437=CARTESIAN_POINT('',(-0.0063407339145214,0.0136710348904156,-0.00059407689693426));
#25438=CARTESIAN_POINT('',(-0.00627455991005623,0.0137336901146997,0.00108997980830424));
#25439=CARTESIAN_POINT('',(-0.00607056143210933,0.0137614834612744,0.00192523714366564));
#25440=CARTESIAN_POINT('',(-0.00571168696851309,0.0137857425422816,0.00268784699493865));
#25441=CARTESIAN_POINT('',(-0.00600291424347733,0.00992240968822442,0.00195066711549076));
#25442=CARTESIAN_POINT('',(-0.00574246615396974,0.0100597652673881,0.00275216088845479));
#25443=CARTESIAN_POINT('',(-0.00531940625127602,0.0101935865809844,0.00350058968249362));
#25444=CARTESIAN_POINT('',(-0.00421487443391306,0.0104541606770422,0.00477333431135781));
#25445=CARTESIAN_POINT('',(-0.0035334025192438,0.0105809134595037,0.00529765014618318));
#25446=CARTESIAN_POINT('',(-0.00201997295760744,0.010827350493292,0.00603903134590732));
#25447=CARTESIAN_POINT('',(-0.00118801531064032,0.0109470347446188,0.00625609671080609));
#25448=CARTESIAN_POINT('',(0.000494691428125635,0.0111793347161375,0.00634864955534043));
#25449=CARTESIAN_POINT('',(0.00134544051992447,0.0112919504363295,0.00622413703497599));
#25450=CARTESIAN_POINT('',(0.0029310462363186,0.0115101133455788,0.00565323588430534));
#25451=CARTESIAN_POINT('',(0.0036659028609139,0.011615660534636,0.00520684725399913));
#25452=CARTESIAN_POINT('',(0.0049033904503219,0.0118196863816157,0.00406286356058454));
#25453=CARTESIAN_POINT('',(0.00540602141513462,0.0119181650395382,0.00336526849747616));
#25454=CARTESIAN_POINT('',(0.00609948672115694,0.0121080538242483,0.00182930645777559));
#25455=CARTESIAN_POINT('',(0.00629032106236656,0.012199463951036,0.000990939481183401));
#25456=CARTESIAN_POINT('',(0.0063299824867198,0.0123752156734767,-0.000693845608950566));
#25457=CARTESIAN_POINT('',(0.00617880956986341,0.0124595572691296,-0.00154026372249235));
#25458=CARTESIAN_POINT('',(0.0055583884213982,0.0126211719293006,-0.00310715596524024));
#25459=CARTESIAN_POINT('',(0.00508914018978937,0.0126984449938188,-0.00382763009444637));
#25460=CARTESIAN_POINT('',(0.00390685436447006,0.0128459225917203,-0.00502857724389744));
#25461=CARTESIAN_POINT('',(0.00319381677075958,0.0129161271251037,-0.00550905026414239));
#25462=CARTESIAN_POINT('',(0.00163683219478167,0.0130494676607356,-0.00615393207365249));
#25463=CARTESIAN_POINT('',(0.000792885212514244,0.0131126036629842,-0.00631834086291762));
#25464=CARTESIAN_POINT('',(-0.000892314492041417,0.0132318071363466,-0.00630506756184519));
#25465=CARTESIAN_POINT('',(-0.00173356721432965,0.0132878746074604,-0.00612738547150761));
#25466=CARTESIAN_POINT('',(-0.00328019981295779,0.0133929410185533,-0.0054580565414708));
#25467=CARTESIAN_POINT('',(-0.0039855796892977,0.0134419399585323,-0.00496640970177156));
#25468=CARTESIAN_POINT('',(-0.00514880328885811,0.0135328693073556,-0.0037469922772707));
#25469=CARTESIAN_POINT('',(-0.0056066470120786,0.0135747997161998,-0.00301922169246908));
#25470=CARTESIAN_POINT('',(-0.00620230170530172,0.0136515920027535,-0.00144273489968662));
#25471=CARTESIAN_POINT('',(-0.00634011267530433,0.0136864538804629,-0.000594018691705766));
#25472=CARTESIAN_POINT('',(-0.00627394515429791,0.013749109104747,0.00108987301653347));
#25473=CARTESIAN_POINT('',(-0.00606996666328886,0.0137769024513217,0.00192504851679185));
#25474=CARTESIAN_POINT('',(-0.00571112736074713,0.013801161532329,0.00268758365066568));
#25475=CARTESIAN_POINT('',(-0.00600291424347733,0.0100627296731023,0.00195066711549077));
#25476=CARTESIAN_POINT('',(-0.00574246615396974,0.010200085252266,0.00275216088845479));
#25477=CARTESIAN_POINT('',(-0.00531940625127601,0.0103339065658623,0.00350058968249363));
#25478=CARTESIAN_POINT('',(-0.00421487443391307,0.0105944806619201,0.00477333431135782));
#25479=CARTESIAN_POINT('',(-0.00353340251924381,0.0107212334443816,0.00529765014618319));
#25480=CARTESIAN_POINT('',(-0.00201997295760744,0.0109676704781699,0.00603903134590733));
#25481=CARTESIAN_POINT('',(-0.00118801531064032,0.0110873547294967,0.0062560967108061));
#25482=CARTESIAN_POINT('',(0.000494691428125638,0.0113196547010155,0.00634864955534044));
#25483=CARTESIAN_POINT('',(0.00134544051992447,0.0114322704212074,0.006224137034976));
#25484=CARTESIAN_POINT('',(0.0029310462363186,0.0116504333304567,0.00565323588430534));
#25485=CARTESIAN_POINT('',(0.0036659028609139,0.0117559805195139,0.00520684725399913));
#25486=CARTESIAN_POINT('',(0.00490339045032191,0.0119600063664936,0.00406286356058454));
#25487=CARTESIAN_POINT('',(0.0054060214151346,0.0120584850244161,0.00336526849747616));
#25488=CARTESIAN_POINT('',(0.00609948672115694,0.0122483738091262,0.00182930645777561));
#25489=CARTESIAN_POINT('',(0.00629032106236657,0.012339783935914,0.000990939481183417));
#25490=CARTESIAN_POINT('',(0.00632998248671981,0.0125155356583546,-0.000693845608950559));
#25491=CARTESIAN_POINT('',(0.00617880956986342,0.0125998772540075,-0.00154026372249234));
#25492=CARTESIAN_POINT('',(0.0055583884213982,0.0127614919141786,-0.00310715596524025));
#25493=CARTESIAN_POINT('',(0.00508914018978937,0.0128387649786967,-0.00382763009444637));
#25494=CARTESIAN_POINT('',(0.00390685436447006,0.0129862425765982,-0.00502857724389744));
#25495=CARTESIAN_POINT('',(0.00319381677075959,0.0130564471099816,-0.00550905026414239));
#25496=CARTESIAN_POINT('',(0.00163683219478168,0.0131897876456135,-0.00615393207365249));
#25497=CARTESIAN_POINT('',(0.000792885212514246,0.0132529236478621,-0.00631834086291763));
#25498=CARTESIAN_POINT('',(-0.000892314492041417,0.0133721271212245,-0.00630506756184518));
#25499=CARTESIAN_POINT('',(-0.00173356721432965,0.0134281945923383,-0.00612738547150761));
#25500=CARTESIAN_POINT('',(-0.00328019981295779,0.0135332610034312,-0.00545805654147079));
#25501=CARTESIAN_POINT('',(-0.00398557968929771,0.0135822599434102,-0.00496640970177156));
#25502=CARTESIAN_POINT('',(-0.00514880328885811,0.0136731892922335,-0.0037469922772707));
#25503=CARTESIAN_POINT('',(-0.0056066470120786,0.0137151197010777,-0.00301922169246908));
#25504=CARTESIAN_POINT('',(-0.00620230170530172,0.0137919119876314,-0.00144273489968662));
#25505=CARTESIAN_POINT('',(-0.00634011267530434,0.0138267738653408,-0.000594018691705788));
#25506=CARTESIAN_POINT('',(-0.00627394515429791,0.0138894290896249,0.00108987301653344));
#25507=CARTESIAN_POINT('',(-0.00606996666328888,0.0139172224361996,0.00192504851679183));
#25508=CARTESIAN_POINT('',(-0.00571112736074714,0.0139414815172069,0.00268758365066566));
#25509=CARTESIAN_POINT('',(-0.00604151039169543,0.0101876306679329,0.00196320906329477));
#25510=CARTESIAN_POINT('',(-0.00577938773336043,0.0103249862470965,0.00276985609535972));
#25511=CARTESIAN_POINT('',(-0.00535360773805049,0.0104588075606928,0.00352309696358349));
#25512=CARTESIAN_POINT('',(-0.00424197425772759,0.0107193816567506,0.00480402479119866));
#25513=CARTESIAN_POINT('',(-0.00355612077271463,0.0108461344392122,0.00533171175059006));
#25514=CARTESIAN_POINT('',(-0.00203296051206952,0.0110925714730005,0.00607785971150886));
#25515=CARTESIAN_POINT('',(-0.00119565373643737,0.0112122557243272,0.00629632071303625));
#25516=CARTESIAN_POINT('',(0.000497872080540071,0.011444555695846,0.0063894686324227));
#25517=CARTESIAN_POINT('',(0.00135409112188536,0.011557171416038,0.00626415555028175));
#25518=CARTESIAN_POINT('',(0.00294989159881799,0.0117753343252872,0.00568958375156659));
#25519=CARTESIAN_POINT('',(0.00368947303440534,0.0118808815143445,0.00524032503499238));
#25520=CARTESIAN_POINT('',(0.00493491713501468,0.0120849073613242,0.00408898602007905));
#25521=CARTESIAN_POINT('',(0.00544077980003667,0.0121833860192466,0.00338690572173993));
#25522=CARTESIAN_POINT('',(0.00613870378873374,0.0123732748039568,0.00184106810891984));
#25523=CARTESIAN_POINT('',(0.00633076511240882,0.0124646849307445,0.000997310794438878));
#25524=CARTESIAN_POINT('',(0.00637068154260601,0.0126404366531851,-0.000698306736809025));
#25525=CARTESIAN_POINT('',(0.00621853664912812,0.012724778248838,-0.00155016695357596));
#25526=CARTESIAN_POINT('',(0.00559412646040137,0.0128863929090091,-0.00312713363730202));
#25527=CARTESIAN_POINT('',(0.0051218611651525,0.0129636659735273,-0.00385224010426115));
#25528=CARTESIAN_POINT('',(0.00393197375215438,0.0131111435714288,-0.00506090882565251));
#25529=CARTESIAN_POINT('',(0.00321435163440513,0.0131813481048121,-0.00554447108008473));
#25530=CARTESIAN_POINT('',(0.00164735631947105,0.0133146886404441,-0.00619349920135166));
#25531=CARTESIAN_POINT('',(0.00079798312228622,0.0133778246426927,-0.00635896506818637));
#25532=CARTESIAN_POINT('',(-0.000898051689175196,0.0134970281160551,-0.00634560642551571));
#25533=CARTESIAN_POINT('',(-0.00174471330345179,0.0135530955871689,-0.00616678191601034));
#25534=CARTESIAN_POINT('',(-0.0033012900822888,0.0136581619982617,-0.00549314948978108));
#25535=CARTESIAN_POINT('',(-0.00401120524684925,0.0137071609382408,-0.00499834157305719));
#25536=CARTESIAN_POINT('',(-0.00518190787220253,0.013798090287064,-0.00377108382071775));
#25537=CARTESIAN_POINT('',(-0.00564269533299538,0.0138400206959083,-0.0030386339851022));
#25538=CARTESIAN_POINT('',(-0.00624217982886001,0.0139168129824619,-0.00145201106252507));
#25539=CARTESIAN_POINT('',(-0.00638087686393179,0.0139516748601714,-0.000597837975563495));
#25540=CARTESIAN_POINT('',(-0.00631428391431779,0.0140143300844555,0.0010968804297296));
#25541=CARTESIAN_POINT('',(-0.00610899392963201,0.0140421234310302,0.00193742574806112));
#25542=CARTESIAN_POINT('',(-0.00574784744522067,0.0140663825120374,0.00270486365379789));
#25543=CARTESIAN_POINT('',(-0.00618115256778337,0.0103897247227974,0.00200858625673483));
#25544=CARTESIAN_POINT('',(-0.00591297126251429,0.0105270803019611,0.00283387795537971));
#25545=CARTESIAN_POINT('',(-0.0054773498796663,0.0106609016155573,0.00360452907156096));
#25546=CARTESIAN_POINT('',(-0.00434002234137772,0.0109214757116152,0.00491506399039386));
#25547=CARTESIAN_POINT('',(-0.00363831618593712,0.0110482284940767,0.00545494779304551));
#25548=CARTESIAN_POINT('',(-0.00207994992554408,0.011294665527865,0.00621834205798284));
#25549=CARTESIAN_POINT('',(-0.00122328982059163,0.0114143497791917,0.00644185252026851));
#25550=CARTESIAN_POINT('',(0.000509379789081899,0.0116466497507105,0.00653715344069573));
#25551=CARTESIAN_POINT('',(0.00138538929380299,0.0117592654709025,0.00640894389883727));
#25552=CARTESIAN_POINT('',(0.0030180747608711,0.0119774283801518,0.00582109157073635));
#25553=CARTESIAN_POINT('',(0.00377475072321812,0.012082975569209,0.00536144878449388));
#25554=CARTESIAN_POINT('',(0.00504898175178574,0.0122870014161887,0.00418349796639993));
#25555=CARTESIAN_POINT('',(0.00556653681800634,0.0123854800741112,0.00346518993454846));
#25556=CARTESIAN_POINT('',(0.00628059247216568,0.0125753688588213,0.00188362216252356));
#25557=CARTESIAN_POINT('',(0.00647709306010441,0.012666778985609,0.00102036242235014));
#25558=CARTESIAN_POINT('',(0.00651793211011238,0.0128425307080496,-0.000714447249029106));
#25559=CARTESIAN_POINT('',(0.00636227057218162,0.0129268723037026,-0.00158599718023493));
#25560=CARTESIAN_POINT('',(0.00572342790020611,0.0130884869638736,-0.00319941353383765));
#25561=CARTESIAN_POINT('',(0.00524024676616137,0.0131657600283918,-0.00394127995623455));
#25562=CARTESIAN_POINT('',(0.00402285655057284,0.0133132376262933,-0.0051778855873524));
#25563=CARTESIAN_POINT('',(0.00328864746902905,0.0133834421596767,-0.00567262479607335));
#25564=CARTESIAN_POINT('',(0.00168543296029903,0.0135167826953086,-0.00633665441420447));
#25565=CARTESIAN_POINT('',(0.000816427533112797,0.0135799186975572,-0.00650594482361463));
#25566=CARTESIAN_POINT('',(-0.000918809063405364,0.0136991221709196,-0.00649227741214095));
#25567=CARTESIAN_POINT('',(-0.0017850402327373,0.0137551896420334,-0.0063093195912571));
#25568=CARTESIAN_POINT('',(-0.00337759539356031,0.0138602560531262,-0.00562011696953312));
#25569=CARTESIAN_POINT('',(-0.0041039193850514,0.0139092549931053,-0.005113872168693));
#25570=CARTESIAN_POINT('',(-0.00530168137992607,0.0140001843419285,-0.00385824784375061));
#25571=CARTESIAN_POINT('',(-0.00577311938330966,0.0140421147507728,-0.00310886831964835));
#25572=CARTESIAN_POINT('',(-0.00638646023530149,0.0141189070373265,-0.00148557253495975));
#25573=CARTESIAN_POINT('',(-0.00652836308390973,0.0141537689150359,-0.000611656274373407));
#25574=CARTESIAN_POINT('',(-0.00646023091913374,0.01421642413932,0.00112223348884646));
#25575=CARTESIAN_POINT('',(-0.00625019590574951,0.0142442174858947,0.00198220699147998));
#25576=CARTESIAN_POINT('',(-0.00588070195891569,0.0142684765669019,0.00276738329245592));
#25577=CARTESIAN_POINT('',(-0.0062821985956532,0.0104669177828314,0.00204142150237086));
#25578=CARTESIAN_POINT('',(-0.00600963321227745,0.010604273361995,0.00288020460849478));
#25579=CARTESIAN_POINT('',(-0.00556689053450765,0.0107380946755913,0.00366345389844858));
#25580=CARTESIAN_POINT('',(-0.00441097060121332,0.0109986687716491,0.00499541270974823));
#25581=CARTESIAN_POINT('',(-0.00369779334568878,0.0111254215541106,0.00554412223109408));
#25582=CARTESIAN_POINT('',(-0.00211395178455655,0.0113718585878989,0.00631999603885528));
#25583=CARTESIAN_POINT('',(-0.00124328747894885,0.0114915428392257,0.00654716032527062));
#25584=CARTESIAN_POINT('',(0.000517706845209291,0.0117238428107445,0.00664401917188651));
#25585=CARTESIAN_POINT('',(0.00140803686375974,0.0118364585309365,0.00651371373208705));
#25586=CARTESIAN_POINT('',(0.00306741256042482,0.0120546214401857,0.00591625152264486));
#25587=CARTESIAN_POINT('',(0.00383645823853945,0.012160168629243,0.00544909475300213));
#25588=CARTESIAN_POINT('',(0.00513151968386402,0.0123641944762227,0.0042518874532263));
#25589=CARTESIAN_POINT('',(0.00565753545107396,0.0124626731341451,0.00352183692309322));
#25590=CARTESIAN_POINT('',(0.00638326408802082,0.0126525619188553,0.00191441456498304));
#25591=CARTESIAN_POINT('',(0.00658297695775774,0.012743972045643,0.00103704273700594));
#25592=CARTESIAN_POINT('',(0.00662448362173253,0.0129197237680836,-0.00072612663339072));
#25593=CARTESIAN_POINT('',(0.0064662774159704,0.0130040653637365,-0.00161192417581028));
#25594=CARTESIAN_POINT('',(0.00581699130100769,0.0131656800239076,-0.0032517157583115));
#25595=CARTESIAN_POINT('',(0.0053259113918071,0.0132429530884257,-0.00400570979839314));
#25596=CARTESIAN_POINT('',(0.00408861996130697,0.0133904306863273,-0.00526253076729722));
#25597=CARTESIAN_POINT('',(0.00334240844000743,0.0134606352197106,-0.00576535769611964));
#25598=CARTESIAN_POINT('',(0.00171298547643764,0.0135939757553426,-0.00644024249935811));
#25599=CARTESIAN_POINT('',(0.000829774034167402,0.0136571117575912,-0.00661230037377415));
#25600=CARTESIAN_POINT('',(-0.000933829240501756,0.0137763152309536,-0.00659840953509567));
#25601=CARTESIAN_POINT('',(-0.00181422107290067,0.0138323827020674,-0.00641246082200114));
#25602=CARTESIAN_POINT('',(-0.0034328104355008,0.0139374491131602,-0.00571199150097489));
#25603=CARTESIAN_POINT('',(-0.004171007965702,0.0139864480531392,-0.00519747089304317));
#25604=CARTESIAN_POINT('',(-0.00538835030430519,0.0140773774019625,-0.00392132032333643));
#25605=CARTESIAN_POINT('',(-0.00586749511270716,0.0141193078108067,-0.0031596903615614));
#25606=CARTESIAN_POINT('',(-0.00649086251818467,0.0141961000973604,-0.00150985784455599));
#25607=CARTESIAN_POINT('',(-0.00663508511526021,0.0142309619750699,-0.00062165528932561));
#25608=CARTESIAN_POINT('',(-0.00656583916392981,0.014293617199354,0.00114057913476716));
#25609=CARTESIAN_POINT('',(-0.00635237061552386,0.0143214105459286,0.00201461100362956));
#25610=CARTESIAN_POINT('',(-0.00597683638813717,0.0143456696269359,0.00281262292798174));
#25611=CARTESIAN_POINT('',(-0.00650814438282647,0.0105441108428653,0.00211484334367094));
#25612=CARTESIAN_POINT('',(-0.00622577590278555,0.010681466422029,0.00298379415403012));
#25613=CARTESIAN_POINT('',(-0.00576710952548274,0.0108152877356253,0.00379521381693169));
#25614=CARTESIAN_POINT('',(-0.00456961573309102,0.0110758618316831,0.00517507790812964));
#25615=CARTESIAN_POINT('',(-0.00383078831800211,0.0112026146141446,0.00574352233642602));
#25616=CARTESIAN_POINT('',(-0.0021899822526698,0.0114490516479329,0.00654730125026951));
#25617=CARTESIAN_POINT('',(-0.00128800360242641,0.0115687358992597,0.00678263573581662));
#25618=CARTESIAN_POINT('',(0.000536326708762601,0.0118010358707784,0.0068829782112943));
#25619=CARTESIAN_POINT('',(0.0014586783697082,0.0119136515909704,0.00674798620122487));
#25620=CARTESIAN_POINT('',(0.00317773523408718,0.0121318145002197,0.00612903564384791));
#25621=CARTESIAN_POINT('',(0.00397444043752055,0.0122373616892769,0.00564507709654037));
#25622=CARTESIAN_POINT('',(0.00531608011071332,0.0124413875362566,0.00440481099471639));
#25623=CARTESIAN_POINT('',(0.00586101458047273,0.0125398661941791,0.00364850344019995));
#25624=CARTESIAN_POINT('',(0.00661284480043267,0.0127297549788892,0.00198326847007294));
#25625=CARTESIAN_POINT('',(0.00681974055063322,0.0128211651056769,0.00107434105446238));
#25626=CARTESIAN_POINT('',(0.00686274004482053,0.0129969168281176,-0.000752242530758643));
#25627=CARTESIAN_POINT('',(0.00669884378880731,0.0130812584237705,-0.00166989870036911));
#25628=CARTESIAN_POINT('',(0.00602620542540606,0.0132428730839416,-0.00336866708760947));
#25629=CARTESIAN_POINT('',(0.00551746331801803,0.0133201461484597,-0.00414977930523935));
#25630=CARTESIAN_POINT('',(0.00423567141814074,0.0134676237463612,-0.00545180314362154));
#25631=CARTESIAN_POINT('',(0.00346262162565148,0.0135378282797446,-0.00597271476437384));
#25632=CARTESIAN_POINT('',(0.00177459477547475,0.0136711688153765,-0.00667187249942069));
#25633=CARTESIAN_POINT('',(0.000859617717787273,0.0137343048176251,-0.00685011861371523));
#25634=CARTESIAN_POINT('',(-0.000967415377523374,0.0138535082909875,-0.00683572817661878));
#25635=CARTESIAN_POINT('',(-0.00187947141514655,0.0139095757621013,-0.00664309162522779));
#25636=CARTESIAN_POINT('',(-0.00355627502266023,0.0140146421731942,-0.00591742919867961));
#25637=CARTESIAN_POINT('',(-0.00432102259255075,0.0140636411131732,-0.00538440332352243));
#25638=CARTESIAN_POINT('',(-0.00558214791075367,0.0141545704619965,-0.00406235467519978));
#25639=CARTESIAN_POINT('',(-0.00607852565906609,0.0141965008708407,-0.00327333190203431));
#25640=CARTESIAN_POINT('',(-0.00672431311971763,0.0142732931573944,-0.00156416144766781));
#25641=CARTESIAN_POINT('',(-0.00687372283205676,0.0143081550351038,-0.000644013766466768));
#25642=CARTESIAN_POINT('',(-0.00680198637827826,0.0143708102593879,0.00118160124613701));
#25643=CARTESIAN_POINT('',(-0.00658084021216063,0.0143986036059626,0.00208706857753974));
#25644=CARTESIAN_POINT('',(-0.00619179950685455,0.0144228626869699,0.00291378182829478));
#25645=CARTESIAN_POINT('',(-0.00663304414212992,0.0105441108428653,0.00215542993933499));
#25646=CARTESIAN_POINT('',(-0.00634525664353049,0.010681466422029,0.00304105704645039));
#25647=CARTESIAN_POINT('',(-0.00587778786161648,0.0108152877356253,0.00386804890852719));
#25648=CARTESIAN_POINT('',(-0.00465731260513313,0.0110758618316831,0.00527439438715669));
#25649=CARTESIAN_POINT('',(-0.00390430613056378,0.0112026146141446,0.0058537480037094));
#25650=CARTESIAN_POINT('',(-0.00223201086177059,0.0114490516479329,0.00667295248081131));
#25651=CARTESIAN_POINT('',(-0.00131272206754674,0.0115687358992597,0.00691280334136051));
#25652=CARTESIAN_POINT('',(0.000546619516188517,0.0118010358707784,0.00701507151951131));
#25653=CARTESIAN_POINT('',(0.00148667230569993,0.0119136515909704,0.00687748883711291));
#25654=CARTESIAN_POINT('',(0.00323872010819583,0.0121318145002197,0.00624665981314244));
#25655=CARTESIAN_POINT('',(0.00405071512118033,0.0122373616892769,0.00575341347157038));
#25656=CARTESIAN_POINT('',(0.00541810260548434,0.0124413875362566,0.00448934504938012));
#25657=CARTESIAN_POINT('',(0.00597349507680387,0.0125398661941791,0.00371852296876192));
#25658=CARTESIAN_POINT('',(0.00673975389698938,0.0127297549788892,0.00202132997270337));
#25659=CARTESIAN_POINT('',(0.00695062024585536,0.0128211651056769,0.00109495905726303));
#25660=CARTESIAN_POINT('',(0.00699444495628839,0.0129969168281176,-0.000766679043764951));
#25661=CARTESIAN_POINT('',(0.00682740331785544,0.0130812584237705,-0.00170194622935258));
#25662=CARTESIAN_POINT('',(0.00614185614900286,0.0132428730839416,-0.00343331619243359));
#25663=CARTESIAN_POINT('',(0.00562335061858323,0.0133201461484597,-0.00422941896992696));
#25664=CARTESIAN_POINT('',(0.00431695946424038,0.0134676237463612,-0.00555643034000104));
#25665=CARTESIAN_POINT('',(0.00352907384031716,0.0135378282797446,-0.00608733893258175));
#25666=CARTESIAN_POINT('',(0.00180865155837324,0.0136711688153765,-0.00679991441432962));
#25667=CARTESIAN_POINT('',(0.000876114900352538,0.0137343048176251,-0.00698158130349679));
#25668=CARTESIAN_POINT('',(-0.0009859813374486,0.0138535082909875,-0.00696691469518718));
#25669=CARTESIAN_POINT('',(-0.00191554091722904,0.0139095757621013,-0.0067705811977104));
#25670=CARTESIAN_POINT('',(-0.00362452456787917,0.0140146421731942,-0.00603099236494257));
#25671=CARTESIAN_POINT('',(-0.00440394863874886,0.0140636411131732,-0.00548773702965151));
#25672=CARTESIAN_POINT('',(-0.00568927659282304,0.0141545704619965,-0.00414031654747732));
#25673=CARTESIAN_POINT('',(-0.00619518047602752,0.0141965008708407,-0.00333615140059418));
#25674=CARTESIAN_POINT('',(-0.00685336143836741,0.0142732931573944,-0.00159417974118338));
#25675=CARTESIAN_POINT('',(-0.00700563851750283,0.0143081550351038,-0.000656373228655721));
#25676=CARTESIAN_POINT('',(-0.00693252534783064,0.0143708102593879,0.00120427771158615));
#25677=CARTESIAN_POINT('',(-0.00670713509902304,0.0143986036059626,0.00212712213930035));
#25678=CARTESIAN_POINT('',(-0.00631062819635044,0.0144228626869699,0.00296970109308201));
#25679=CARTESIAN_POINT('',(-0.0068589899293032,0.0104669177828314,0.00222885178063507));
#25680=CARTESIAN_POINT('',(-0.00656139933403859,0.010604273361995,0.00314464659198573));
#25681=CARTESIAN_POINT('',(-0.00607800685259157,0.0107380946755913,0.0039998088270103));
#25682=CARTESIAN_POINT('',(-0.00481595773701083,0.0109986687716491,0.00545405958553811));
#25683=CARTESIAN_POINT('',(-0.00403730110287711,0.0111254215541107,0.00605314810904135));
#25684=CARTESIAN_POINT('',(-0.00230804132988384,0.0113718585878989,0.00690025769222555));
#25685=CARTESIAN_POINT('',(-0.00135743819102429,0.0114915428392257,0.00714827875190651));
#25686=CARTESIAN_POINT('',(0.000565239379741828,0.0117238428107445,0.0072540305589191));
#25687=CARTESIAN_POINT('',(0.00153731381164839,0.0118364585309365,0.00711176130625072));
#25688=CARTESIAN_POINT('',(0.0033490427818582,0.0120546214401857,0.00645944393434549));
#25689=CARTESIAN_POINT('',(0.00418869732016144,0.012160168629243,0.00594939581510862));
#25690=CARTESIAN_POINT('',(0.00560266303233365,0.0123641944762227,0.0046422685908702));
#25691=CARTESIAN_POINT('',(0.00617697420620264,0.0124626731341451,0.00384518948586864));
#25692=CARTESIAN_POINT('',(0.00696933460940123,0.0126525619188553,0.00209018387779328));
#25693=CARTESIAN_POINT('',(0.00718738383873084,0.012743972045643,0.00113225737471947));
#25694=CARTESIAN_POINT('',(0.0072327013793764,0.0129197237680836,-0.000792794941132875));
#25695=CARTESIAN_POINT('',(0.00705996969069235,0.0130040653637365,-0.00175992075391141));
#25696=CARTESIAN_POINT('',(0.00635107027340123,0.0131656800239076,-0.00355026752173156));
#25697=CARTESIAN_POINT('',(0.00581490254479415,0.0132429530884257,-0.00437348847677317));
#25698=CARTESIAN_POINT('',(0.00446401092107414,0.0133904306863273,-0.00574570271632536));
#25699=CARTESIAN_POINT('',(0.00364928702596121,0.0134606352197106,-0.00629469600083594));
#25700=CARTESIAN_POINT('',(0.00187026085741034,0.0135939757553426,-0.0070315444143922));
#25701=CARTESIAN_POINT('',(0.000905958583972411,0.0136571117575912,-0.00721939954343787));
#25702=CARTESIAN_POINT('',(-0.00101956747447021,0.0137763152309536,-0.0072042333367103));
#25703=CARTESIAN_POINT('',(-0.00198079125947491,0.0138323827020674,-0.00700121200093705));
#25704=CARTESIAN_POINT('',(-0.0037479891550386,0.0139374491131602,-0.00623643006264729));
#25705=CARTESIAN_POINT('',(-0.0045539632655976,0.0139864480531392,-0.00567466946013077));
#25706=CARTESIAN_POINT('',(-0.00588307419927152,0.0140773774019625,-0.00428135089934067));
#25707=CARTESIAN_POINT('',(-0.00640621102238644,0.0141193078108067,-0.0034497929410671));
#25708=CARTESIAN_POINT('',(-0.00708681203990037,0.0141961000973604,-0.0016484833442952));
#25709=CARTESIAN_POINT('',(-0.00724427623429938,0.0142309619750699,-0.000678731705796876));
#25710=CARTESIAN_POINT('',(-0.0071686725621791,0.014293617199354,0.00124529982295599));
#25711=CARTESIAN_POINT('',(-0.00693560469565981,0.0143214105459286,0.00219957971321054));
#25712=CARTESIAN_POINT('',(-0.00652559131506782,0.0143456696269359,0.00307085999339506));
#25713=CARTESIAN_POINT('',(-0.00696003595717303,0.0103897247227974,0.00226168702627111));
#25714=CARTESIAN_POINT('',(-0.00665806128380176,0.0105270803019611,0.0031909732451008));
#25715=CARTESIAN_POINT('',(-0.00616754750743291,0.0106609016155573,0.00405873365389792));
#25716=CARTESIAN_POINT('',(-0.00488690599684642,0.0109214757116152,0.00553440830489247));
#25717=CARTESIAN_POINT('',(-0.00409677826262877,0.0110482284940767,0.00614232254708991));
#25718=CARTESIAN_POINT('',(-0.00234204318889632,0.011294665527865,0.00700191167309799));
#25719=CARTESIAN_POINT('',(-0.00137743584938151,0.0114143497791917,0.00725358655690862));
#25720=CARTESIAN_POINT('',(0.000573566435869221,0.0116466497507105,0.00736089629010987));
#25721=CARTESIAN_POINT('',(0.00155996138160514,0.0117592654709025,0.0072165311395005));
#25722=CARTESIAN_POINT('',(0.00339838058141192,0.0119774283801518,0.006554603886254));
#25723=CARTESIAN_POINT('',(0.00425040483548277,0.012082975569209,0.00603704178361687));
#25724=CARTESIAN_POINT('',(0.00568520096441194,0.0122870014161887,0.00471065807769657));
#25725=CARTESIAN_POINT('',(0.00626797283927026,0.0123854800741112,0.0039018364744134));
#25726=CARTESIAN_POINT('',(0.00707200622525638,0.0125753688588213,0.00212097628025274));
#25727=CARTESIAN_POINT('',(0.00729326773638417,0.012666778985609,0.00114893768937527));
#25728=CARTESIAN_POINT('',(0.00733925289099655,0.0128425307080496,-0.00080447432549449));
#25729=CARTESIAN_POINT('',(0.00716397653448113,0.0129268723037026,-0.00178584774948676));
#25730=CARTESIAN_POINT('',(0.0064446336742028,0.0130884869638736,-0.00360256974620541));
#25731=CARTESIAN_POINT('',(0.00590056717043989,0.0131657600283918,-0.00443791831893177));
#25732=CARTESIAN_POINT('',(0.00452977433180828,0.0133132376262933,-0.00583034789627018));
#25733=CARTESIAN_POINT('',(0.00370304799693959,0.0133834421596767,-0.00638742890088223));
#25734=CARTESIAN_POINT('',(0.00189781337354896,0.0135167826953086,-0.00713513249954584));
#25735=CARTESIAN_POINT('',(0.000919305085027019,0.0135799186975572,-0.00732575509359739));
#25736=CARTESIAN_POINT('',(-0.0010345876515666,0.0136991221709196,-0.00731036545966502));
#25737=CARTESIAN_POINT('',(-0.00200997209963829,0.0137551896420334,-0.00710435323168109));
#25738=CARTESIAN_POINT('',(-0.00380320419697909,0.0138602560531262,-0.00632830459408906));
#25739=CARTESIAN_POINT('',(-0.00462105184624821,0.0139092549931053,-0.00575826818448095));
#25740=CARTESIAN_POINT('',(-0.00596974312365063,0.0140001843419285,-0.00434442337892649));
#25741=CARTESIAN_POINT('',(-0.00650058675178394,0.0140421147507728,-0.00350061498298014));
#25742=CARTESIAN_POINT('',(-0.00719121432278355,0.0141189070373265,-0.00167276865389143));
#25743=CARTESIAN_POINT('',(-0.00735099826564986,0.0141537689150359,-0.000688730720749077));
#25744=CARTESIAN_POINT('',(-0.00727428080697517,0.01421642413932,0.0012636454688767));
#25745=CARTESIAN_POINT('',(-0.00703777940543416,0.0142442174858947,0.00223198372536013));
#25746=CARTESIAN_POINT('',(-0.00662172574428931,0.0142684765669019,0.00311609962892087));
#25747=CARTESIAN_POINT('',(-0.00709967813326097,0.0101876306679329,0.00230706421971116));
#25748=CARTESIAN_POINT('',(-0.00679164481295561,0.0103249862470965,0.00325499510512079));
#25749=CARTESIAN_POINT('',(-0.00629128964904872,0.0104588075606928,0.00414016576187539));
#25750=CARTESIAN_POINT('',(-0.00498495408049655,0.0107193816567506,0.00564544750408768));
#25751=CARTESIAN_POINT('',(-0.00417897367585126,0.0108461344392122,0.00626555858954536));
#25752=CARTESIAN_POINT('',(-0.00238903260237088,0.0110925714730005,0.00714239401957196));
#25753=CARTESIAN_POINT('',(-0.00140507193353578,0.0112122557243272,0.00739911836414088));
#25754=CARTESIAN_POINT('',(0.000585074144411049,0.011444555695846,0.00750858109838291));
#25755=CARTESIAN_POINT('',(0.00159125955352277,0.011557171416038,0.00736131948805603));
#25756=CARTESIAN_POINT('',(0.00346656374346502,0.0117753343252872,0.00668611170542376));
#25757=CARTESIAN_POINT('',(0.00433568252429554,0.0118808815143445,0.00615816553311837));
#25758=CARTESIAN_POINT('',(0.00579926558118299,0.0120849073613242,0.00480517002401746));
#25759=CARTESIAN_POINT('',(0.00639372985723993,0.0121833860192466,0.00398012068722193));
#25760=CARTESIAN_POINT('',(0.00721389490868831,0.0123732748039568,0.00216353033385647));
#25761=CARTESIAN_POINT('',(0.00743959568407976,0.0124646849307445,0.00117198931728653));
#25762=CARTESIAN_POINT('',(0.00748650345850291,0.0126404366531851,-0.00082061483771457));
#25763=CARTESIAN_POINT('',(0.00730771045753463,0.012724778248838,-0.00182167797614574));
#25764=CARTESIAN_POINT('',(0.00657393511400755,0.0128863929090091,-0.00367484964274103));
#25765=CARTESIAN_POINT('',(0.00601895277144875,0.0129636659735273,-0.00452695817090515));
#25766=CARTESIAN_POINT('',(0.00462065713022674,0.0131111435714288,-0.00594732465797007));
#25767=CARTESIAN_POINT('',(0.00377734383156351,0.0131813481048121,-0.00651558261687087));
#25768=CARTESIAN_POINT('',(0.00193589001437694,0.0133146886404441,-0.00727828771239866));
#25769=CARTESIAN_POINT('',(0.0009377494958536,0.0133778246426927,-0.00747273484902566));
#25770=CARTESIAN_POINT('',(-0.00105534502579677,0.0134970281160551,-0.00745703644629025));
#25771=CARTESIAN_POINT('',(-0.0020502990289238,0.0135530955871689,-0.00724689090692786));
#25772=CARTESIAN_POINT('',(-0.00387950950825059,0.0136581619982617,-0.00645527207384111));
#25773=CARTESIAN_POINT('',(-0.00471376598445036,0.0137071609382408,-0.00587379878011676));
#25774=CARTESIAN_POINT('',(-0.00608951663137417,0.013798090287064,-0.00443158740195936));
#25775=CARTESIAN_POINT('',(-0.00663101080209822,0.0138400206959083,-0.0035708493175263));
#25776=CARTESIAN_POINT('',(-0.00733549472922503,0.013916812982462,-0.00170633012632612));
#25777=CARTESIAN_POINT('',(-0.0074984844856278,0.0139516748601714,-0.000702549019558997));
#25778=CARTESIAN_POINT('',(-0.00742022781179112,0.0140143300844555,0.00128899852799355));
#25779=CARTESIAN_POINT('',(-0.00717898138155166,0.0140421234310302,0.00227676496877898));
#25780=CARTESIAN_POINT('',(-0.00675458025798432,0.0140663825120374,0.00317861926757889));
#25781=CARTESIAN_POINT('',(-0.00713827428147907,0.0100627296731023,0.00231960616751517));
#25782=CARTESIAN_POINT('',(-0.0068285663923463,0.010200085252266,0.00327269031202572));
#25783=CARTESIAN_POINT('',(-0.00632549113582319,0.0103339065658623,0.00416267304296526));
#25784=CARTESIAN_POINT('',(-0.00501205390431109,0.0105944806619201,0.00567613798392852));
#25785=CARTESIAN_POINT('',(-0.0042016919293221,0.0107212334443816,0.00629962019395224));
#25786=CARTESIAN_POINT('',(-0.00240202015683297,0.0109676704781699,0.0071812223851735));
#25787=CARTESIAN_POINT('',(-0.00141271035933283,0.0110873547294967,0.00743934236637103));
#25788=CARTESIAN_POINT('',(0.000588254796825484,0.0113196547010154,0.00754940017546517));
#25789=CARTESIAN_POINT('',(0.00159991015548366,0.0114322704212074,0.00740133800336178));
#25790=CARTESIAN_POINT('',(0.00348540910596441,0.0116504333304567,0.00672245957268501));
#25791=CARTESIAN_POINT('',(0.00435925269778697,0.0117559805195139,0.00619164331411162));
#25792=CARTESIAN_POINT('',(0.00583079226587576,0.0119600063664936,0.00483129248351197));
#25793=CARTESIAN_POINT('',(0.00642848824214198,0.0120584850244161,0.00400175791148571));
#25794=CARTESIAN_POINT('',(0.0072531119762651,0.0122483738091262,0.00217529198500073));
#25795=CARTESIAN_POINT('',(0.00748003973412201,0.0123397839359139,0.001178360630542));
#25796=CARTESIAN_POINT('',(0.00752720251438913,0.0125155356583546,-0.000825075965573034));
#25797=CARTESIAN_POINT('',(0.00734743753679934,0.0125998772540075,-0.00183158120722935));
#25798=CARTESIAN_POINT('',(0.00660967315301072,0.0127614919141786,-0.0036948273148028));
#25799=CARTESIAN_POINT('',(0.00605167374681188,0.0128387649786967,-0.00455156818071994));
#25800=CARTESIAN_POINT('',(0.00464577651791105,0.0129862425765982,-0.00597965623972514));
#25801=CARTESIAN_POINT('',(0.00379787869520906,0.0130564471099816,-0.0065510034328132));
#25802=CARTESIAN_POINT('',(0.00194641413906631,0.0131897876456136,-0.00731785484009783));
#25803=CARTESIAN_POINT('',(0.000942847405625574,0.0132529236478621,-0.0075133590542944));
#25804=CARTESIAN_POINT('',(-0.00106108222293055,0.0133721271212245,-0.00749757530996077));
#25805=CARTESIAN_POINT('',(-0.00206144511804592,0.0134281945923384,-0.00728628735143058));
#25806=CARTESIAN_POINT('',(-0.0039005997775816,0.0135332610034312,-0.00649036502215139));
#25807=CARTESIAN_POINT('',(-0.0047393915420019,0.0135822599434102,-0.00590573065140239));
#25808=CARTESIAN_POINT('',(-0.0061226212147186,0.0136731892922335,-0.0044556789454064));
#25809=CARTESIAN_POINT('',(-0.006667059123015,0.0137151197010777,-0.00359026161015942));
#25810=CARTESIAN_POINT('',(-0.00737537285278333,0.0137919119876314,-0.00171560628916458));
#25811=CARTESIAN_POINT('',(-0.00753924867425526,0.0138267738653408,-0.000706368303416717));
#25812=CARTESIAN_POINT('',(-0.00746056657181099,0.0138894290896249,0.00129600594118969));
#25813=CARTESIAN_POINT('',(-0.0072180086478948,0.0139172224361996,0.00228914220004824));
#25814=CARTESIAN_POINT('',(-0.00679130034245786,0.0139414815172069,0.0031958992707111));
#25815=CARTESIAN_POINT('',(-0.00713827428147907,0.00992240968822442,0.00231960616751517));
#25816=CARTESIAN_POINT('',(-0.00682856639234631,0.0100597652673881,0.00327269031202572));
#25817=CARTESIAN_POINT('',(-0.0063254911358232,0.0101935865809844,0.00416267304296526));
#25818=CARTESIAN_POINT('',(-0.00501205390431109,0.0104541606770422,0.00567613798392852));
#25819=CARTESIAN_POINT('',(-0.0042016919293221,0.0105809134595037,0.00629962019395224));
#25820=CARTESIAN_POINT('',(-0.00240202015683297,0.010827350493292,0.0071812223851735));
#25821=CARTESIAN_POINT('',(-0.00141271035933283,0.0109470347446188,0.00743934236637104));
#25822=CARTESIAN_POINT('',(0.000588254796825481,0.0111793347161375,0.00754940017546518));
#25823=CARTESIAN_POINT('',(0.00159991015548366,0.0112919504363295,0.00740133800336179));
#25824=CARTESIAN_POINT('',(0.00348540910596441,0.0115101133455788,0.00672245957268501));
#25825=CARTESIAN_POINT('',(0.00435925269778697,0.011615660534636,0.00619164331411162));
#25826=CARTESIAN_POINT('',(0.00583079226587576,0.0118196863816157,0.00483129248351197));
#25827=CARTESIAN_POINT('',(0.00642848824214198,0.0119181650395382,0.00400175791148571));
#25828=CARTESIAN_POINT('',(0.00725311197626511,0.0121080538242483,0.00217529198500073));
#25829=CARTESIAN_POINT('',(0.00748003973412201,0.012199463951036,0.00117836063054201));
#25830=CARTESIAN_POINT('',(0.00752720251438913,0.0123752156734767,-0.000825075965573031));
#25831=CARTESIAN_POINT('',(0.00734743753679934,0.0124595572691296,-0.00183158120722935));
#25832=CARTESIAN_POINT('',(0.00660967315301072,0.0126211719293006,-0.00369482731480281));
#25833=CARTESIAN_POINT('',(0.00605167374681189,0.0126984449938188,-0.00455156818071995));
#25834=CARTESIAN_POINT('',(0.00464577651791106,0.0128459225917203,-0.00597965623972514));
#25835=CARTESIAN_POINT('',(0.00379787869520906,0.0129161271251037,-0.0065510034328132));
#25836=CARTESIAN_POINT('',(0.00194641413906631,0.0130494676607356,-0.00731785484009783));
#25837=CARTESIAN_POINT('',(0.000942847405625573,0.0131126036629842,-0.0075133590542944));
#25838=CARTESIAN_POINT('',(-0.00106108222293055,0.0132318071363466,-0.00749757530996077));
#25839=CARTESIAN_POINT('',(-0.00206144511804593,0.0132878746074604,-0.00728628735143058));
#25840=CARTESIAN_POINT('',(-0.00390059977758161,0.0133929410185533,-0.00649036502215139));
#25841=CARTESIAN_POINT('',(-0.0047393915420019,0.0134419399585323,-0.00590573065140239));
#25842=CARTESIAN_POINT('',(-0.0061226212147186,0.0135328693073556,-0.0044556789454064));
#25843=CARTESIAN_POINT('',(-0.006667059123015,0.0135747997161998,-0.00359026161015942));
#25844=CARTESIAN_POINT('',(-0.00737537285278333,0.0136515920027535,-0.00171560628916457));
#25845=CARTESIAN_POINT('',(-0.00753924867425526,0.0136864538804629,-0.000706368303416719));
#25846=CARTESIAN_POINT('',(-0.007460566571811,0.013749109104747,0.00129600594118969));
#25847=CARTESIAN_POINT('',(-0.0072180086478948,0.0137769024513217,0.00228914220004825));
#25848=CARTESIAN_POINT('',(-0.00679130034245786,0.013801161532329,0.0031958992707111));
#25849=CARTESIAN_POINT('',(-0.00713768608282461,0.00990699069817707,0.00231941503038975));
#25850=CARTESIAN_POINT('',(-0.0068280037138325,0.0100443462773407,0.00327242064011874));
#25851=CARTESIAN_POINT('',(-0.00632496991105259,0.010178167590937,0.00416233003587611));
#25852=CARTESIAN_POINT('',(-0.00501164090766143,0.0104387416869948,0.00567567026629915));
#25853=CARTESIAN_POINT('',(-0.00420134570705017,0.0105654944694564,0.00629910110096484));
#25854=CARTESIAN_POINT('',(-0.00240182222873878,0.0108119315032447,0.00718063064756609));
#25855=CARTESIAN_POINT('',(-0.00141259395103865,0.0109316157545714,0.00743872935950167));
#25856=CARTESIAN_POINT('',(0.000588206324230238,0.0111639157260902,0.00754877809975751));
#25857=CARTESIAN_POINT('',(0.00159977832179899,0.0112765314462822,0.00740072812807777));
#25858=CARTESIAN_POINT('',(0.00348512190588417,0.0114946943555314,0.00672190563744528));
#25859=CARTESIAN_POINT('',(0.0043588934924006,0.0116002415445887,0.00619113311849253));
#25860=CARTESIAN_POINT('',(0.00583031180462841,0.0118042673915684,0.00483089438172629));
#25861=CARTESIAN_POINT('',(0.00642795853033978,0.0119027460494908,0.0040014281639128));
#25862=CARTESIAN_POINT('',(0.00725251431490651,0.012092634834201,0.00217511273946207));
#25863=CARTESIAN_POINT('',(0.00747942337376187,0.0121840449609887,0.00117826353282482));
#25864=CARTESIAN_POINT('',(0.00752658226778383,0.0123597966834293,-0.000825007978752457));
#25865=CARTESIAN_POINT('',(0.00734683210295042,0.0124441382790822,-0.00183143028369249));
#25866=CARTESIAN_POINT('',(0.00660912851144867,0.0126057529392533,-0.00369452285851977));
#25867=CARTESIAN_POINT('',(0.00605117508478032,0.0126830260037714,-0.00455119312840702));
#25868=CARTESIAN_POINT('',(0.00464539370276709,0.012830503601673,-0.00597916351198512));
#25869=CARTESIAN_POINT('',(0.00379756574742221,0.0129007081350563,-0.00655046362567598));
#25870=CARTESIAN_POINT('',(0.00194625375321779,0.0130340486706883,-0.00731725184388323));
#25871=CARTESIAN_POINT('',(0.000942769714358262,0.0130971846729369,-0.00751273994839962));
#25872=CARTESIAN_POINT('',(-0.0010609947890339,0.0132163881462993,-0.00749695750465726));
#25873=CARTESIAN_POINT('',(-0.00206127525356652,0.0132724556174131,-0.00728568695639851));
#25874=CARTESIAN_POINT('',(-0.00390027836550772,0.0133775220285059,-0.00648983021166044));
#25875=CARTESIAN_POINT('',(-0.00473900101291629,0.013426520968485,-0.00590524401518111));
#25876=CARTESIAN_POINT('',(-0.00612211670656743,0.0135174503173082,-0.00445531179443167));
#25877=CARTESIAN_POINT('',(-0.00666650975281,0.0135593807261525,-0.00358996577016154));
#25878=CARTESIAN_POINT('',(-0.00737476511704538,0.0136361730127061,-0.00171546492203982));
#25879=CARTESIAN_POINT('',(-0.00753862743503819,0.0136710348904156,-0.000706310098188223));
#25880=CARTESIAN_POINT('',(-0.00745995181605267,0.0137336901146997,0.00129589914941892));
#25881=CARTESIAN_POINT('',(-0.00721741387907434,0.0137614834612743,0.00228895357317447));
#25882=CARTESIAN_POINT('',(-0.0067907407346919,0.0137857425422816,0.00319563592643815));
#25883=CARTESIAN_POINT('',(-0.00713652355335438,0.00989161658584234,0.0023190372625396));
#25884=CARTESIAN_POINT('',(-0.00682689162296045,0.010028972165006,0.00327188765430387));
#25885=CARTESIAN_POINT('',(-0.00632393975032057,0.0101627934786023,0.00416165210870539));
#25886=CARTESIAN_POINT('',(-0.00501082465149917,0.0104233675746601,0.00567474585832276));
#25887=CARTESIAN_POINT('',(-0.00420066142531763,0.0105501203571216,0.00629807515353861));
#25888=CARTESIAN_POINT('',(-0.0024014310390604,0.0107965573909099,0.00717946112362713));
#25889=CARTESIAN_POINT('',(-0.00141236387898469,0.0109162416422367,0.0074375177984998));
#25890=CARTESIAN_POINT('',(0.000588110521868161,0.0111485416137555,0.00754754861489316));
#25891=CARTESIAN_POINT('',(0.00159951776264531,0.0112611573339475,0.00739952275641386));
#25892=CARTESIAN_POINT('',(0.00348455427698092,0.0114793202431967,0.00672081082698304));
#25893=CARTESIAN_POINT('',(0.00435818355053937,0.0115848674322539,0.00619012475603152));
#25894=CARTESIAN_POINT('',(0.0058293622098697,0.0117888932792336,0.00483010756411885));
#25895=CARTESIAN_POINT('',(0.00642691159564158,0.0118873719371561,0.00400077644315771));
#25896=CARTESIAN_POINT('',(0.00725133308312823,0.0120772607218663,0.00217475847441996));
#25897=CARTESIAN_POINT('',(0.00747820518484301,0.012168670848654,0.00117807162664336));
#25898=CARTESIAN_POINT('',(0.00752535639799984,0.0123444225710946,-0.000824873608022594));
#25899=CARTESIAN_POINT('',(0.0073456355094419,0.0124287641667475,-0.00183113199491196));
#25900=CARTESIAN_POINT('',(0.00660805206922664,0.0125903788269186,-0.00369392112405686));
#25901=CARTESIAN_POINT('',(0.00605018951756932,0.0126676518914367,-0.00455045186631239));
#25902=CARTESIAN_POINT('',(0.00464463709803305,0.0128151294893382,-0.00597818967344566));
#25903=CARTESIAN_POINT('',(0.0037969472301541,0.0128853340227216,-0.00654939673832338));
#25904=CARTESIAN_POINT('',(0.00194593676290491,0.0130186745583536,-0.00731606006817175));
#25905=CARTESIAN_POINT('',(0.000942616163534665,0.0130818105606022,-0.00751151633314239));
#25906=CARTESIAN_POINT('',(-0.00106082198265159,0.0132010140339646,-0.00749573645991879));
#25907=CARTESIAN_POINT('',(-0.0020609395294676,0.0132570815050784,-0.00728450032172455));
#25908=CARTESIAN_POINT('',(-0.0038996431192263,0.0133621479161712,-0.00648877319979548));
#25909=CARTESIAN_POINT('',(-0.00473822916216899,0.0134111468561502,-0.00590428221606065));
#25910=CARTESIAN_POINT('',(-0.00612111958495,0.0135020762049735,-0.0044545861487252));
#25911=CARTESIAN_POINT('',(-0.00666542396478831,0.0135440066138177,-0.00358938106512457));
#25912=CARTESIAN_POINT('',(-0.00737356397402995,0.0136207989003714,-0.00171518552077393));
#25913=CARTESIAN_POINT('',(-0.00753739960343328,0.0136556607780809,-0.000706195060023929));
#25914=CARTESIAN_POINT('',(-0.00745873679850607,0.013718316002365,0.00129568808368499));
#25915=CARTESIAN_POINT('',(-0.00721623836417553,0.0137461093489396,0.0022885807666439));
#25916=CARTESIAN_POINT('',(-0.00678963471291716,0.0137703684299469,0.00319511544670599));
#25917=CARTESIAN_POINT('',(-0.00586854359428379,0.0100021880658147,0.00232352468558585));
#25918=CARTESIAN_POINT('',(-0.00586854666444476,0.0101583123241833,0.00232352584836629));
#25919=CARTESIAN_POINT('',(-0.00598875051569713,0.0104696625508096,0.00237111789406724));
#25920=CARTESIAN_POINT('',(-0.00642351691599961,0.0106633822281906,0.00254325419483785));
#25921=CARTESIAN_POINT('',(-0.00685828316600545,0.0104696620957779,0.00271539041001652));
#25922=CARTESIAN_POINT('',(-0.00697848678069458,0.0101583117238101,0.00276298232952899));
#25923=CARTESIAN_POINT('',(-0.00697848972311123,0.0100021874495698,0.00276298343174812));
#25924=CARTESIAN_POINT('',(0.00749108874705881,-4.87817538710732E-5,0.000441214548496381));
#25925=CARTESIAN_POINT('',(0.00756192879546182,0.000121259456510575,-0.000807448822781952));
#25926=CARTESIAN_POINT('',(0.00732073880436713,0.000291300666892227,-0.0020746366380809));
#25927=CARTESIAN_POINT('',(0.00610734286898242,0.000678055776640972,-0.00464385789087092));
#25928=CARTESIAN_POINT('',(0.00495265952689379,0.000894769676008066,-0.00585998761368964));
#25929=CARTESIAN_POINT('',(0.00214648654660137,0.00132819747474226,-0.00736641318963322));
#25930=CARTESIAN_POINT('',(0.00049499690839756,0.00154491137410936,-0.00765670904275807));
#25931=CARTESIAN_POINT('',(-0.00265670621037452,0.00197833917284356,-0.00719800623814542));
#25932=CARTESIAN_POINT('',(-0.00415691969094279,0.00219505307221066,-0.00644900758040792));
#25933=CARTESIAN_POINT('',(-0.00641745568980185,0.00262848087094487,-0.00420548154343388));
#25934=CARTESIAN_POINT('',(-0.00717777820809264,0.00284519477031198,-0.00271095416419734));
#25935=CARTESIAN_POINT('',(-0.00766019843077886,0.00327862256904619,0.000437190225863992));
#25936=CARTESIAN_POINT('',(-0.00738229613517428,0.0034953364684133,0.00209080723668879));
#25937=CARTESIAN_POINT('',(-0.0058973088636481,0.00392876426714751,0.00490831015468373));
#25938=CARTESIAN_POINT('',(-0.0046902238877265,0.00414547816651461,0.00607219606185387));
#25939=CARTESIAN_POINT('',(-0.00182049443363357,0.00457890596524882,0.00745356085311647));
#25940=CARTESIAN_POINT('',(-0.000157849955462233,0.00479561986461592,0.00767103973720893));
#25941=CARTESIAN_POINT('',(0.00297062710608921,0.00522904766335012,0.00707425910289169));
#25942=CARTESIAN_POINT('',(0.00443645968946931,0.00544576156271722,0.00625999958448199));
#25943=CARTESIAN_POINT('',(0.00659616431998675,0.00587918936145141,0.00391923224552048));
#25944=CARTESIAN_POINT('',(0.00729003636712409,0.00609590326081851,0.00239272442496866));
#25945=CARTESIAN_POINT('',(0.00763356678947157,0.00652933105955269,-0.000773582057105439));
#25946=CARTESIAN_POINT('',(0.00728322516468172,0.00674604495891977,-0.00241338071862772));
#25947=CARTESIAN_POINT('',(0.00567578698717706,0.00717947275765394,-0.00516286883051849));
#25948=CARTESIAN_POINT('',(0.00441869043446227,0.00739618665702102,-0.00627255828088698));
#25949=CARTESIAN_POINT('',(0.00149100660428099,0.00782961445575517,-0.00752639218982749));
#25950=CARTESIAN_POINT('',(-0.000179580673185502,0.00804632835512224,-0.00767053664839951));
#25951=CARTESIAN_POINT('',(-0.00327882363689482,0.00847975615385636,-0.00693682426351677));
#25952=CARTESIAN_POINT('',(-0.00470747932313764,0.00869647005322342,-0.00605896742006202));
#25953=CARTESIAN_POINT('',(-0.00676205316791046,0.00912989785195752,-0.00362531766556786));
#25954=CARTESIAN_POINT('',(-0.00738797132644047,0.00934661175132457,-0.00206952475452845));
#25955=CARTESIAN_POINT('',(-0.00756094562580771,0.0097133646794052,0.000619311369760928));
#25956=CARTESIAN_POINT('',(-0.00738068052708896,0.0098634037081188,0.00173515302320011));
#25957=CARTESIAN_POINT('',(-0.0069762626742443,0.0100134427368324,0.00276211433842094));
#25958=CARTESIAN_POINT('',(0.00749116155653293,-5.25309875529011E-5,0.000441218836871587));
#25959=CARTESIAN_POINT('',(0.00756200229346425,0.000117510222828747,-0.00080745667076322));
#25960=CARTESIAN_POINT('',(0.00732080995812869,0.000287551433210399,-0.00207465680246657));
#25961=CARTESIAN_POINT('',(0.00610740222916858,0.000674306542959144,-0.00464390302674667));
#25962=CARTESIAN_POINT('',(0.00495270766416033,0.000891020442326238,-0.00586004456971178));
#25963=CARTESIAN_POINT('',(0.00214650740933066,0.00132444824106043,-0.00736648478732597));
#25964=CARTESIAN_POINT('',(0.000495001719509243,0.00154116214042753,-0.00765678346197505));
#25965=CARTESIAN_POINT('',(-0.00265673203217274,0.00197458993916174,-0.00719807619901047));
#25966=CARTESIAN_POINT('',(-0.0041569600940333,0.00219130383852884,-0.00644907026139681));
#25967=CARTESIAN_POINT('',(-0.00641751806412282,0.00262473163726305,-0.00420552241852026));
#25968=CARTESIAN_POINT('',(-0.0071778479723518,0.00284144553663015,-0.00271098051325737));
#25969=CARTESIAN_POINT('',(-0.00766027288391087,0.00327487333536436,0.000437194475124882));
#25970=CARTESIAN_POINT('',(-0.00738236788724097,0.00349158723473147,0.00209082755824425));
#25971=CARTESIAN_POINT('',(-0.00589736618241331,0.00392501503346568,0.00490835786089751));
#25972=CARTESIAN_POINT('',(-0.00469026947425555,0.00414172893283278,0.0060722550804314));
#25973=CARTESIAN_POINT('',(-0.00182051212788961,0.00457515673156699,0.00745363329783904));
#25974=CARTESIAN_POINT('',(-0.000157851489681442,0.00479187063093409,0.00767111429571278));
#25975=CARTESIAN_POINT('',(0.00297065597903474,0.0052252984296683,0.00707432786099915));
#25976=CARTESIAN_POINT('',(0.00443650280954275,0.0054420123290354,0.00626006042841178));
#25977=CARTESIAN_POINT('',(0.00659622843126237,0.00587544012776958,0.00391927033841303));
#25978=CARTESIAN_POINT('',(0.00729010722247398,0.00609215402713668,0.00239274768100166));
#25979=CARTESIAN_POINT('',(0.00763364098375792,0.00652558182587087,-0.000773589575919415));
#25980=CARTESIAN_POINT('',(0.00728329595383027,0.00674229572523794,-0.00241340417542911));
#25981=CARTESIAN_POINT('',(0.00567584215286522,0.00717572352397212,-0.00516291901090978));
#25982=CARTESIAN_POINT('',(0.00441873338182783,0.0073924374233392,-0.00627261924688074));
#25983=CARTESIAN_POINT('',(0.00149102109608724,0.00782586522207334,-0.00752646534243265));
#25984=CARTESIAN_POINT('',(-0.000179582418615949,0.00804257912144041,-0.0076706112020136));
#25985=CARTESIAN_POINT('',(-0.00327885550534983,0.00847600692017453,-0.0069368916858293));
#25986=CARTESIAN_POINT('',(-0.00470752507738052,0.00869272081954159,-0.00605902631006405));
#25987=CARTESIAN_POINT('',(-0.00676211889153913,0.00912614861827569,-0.00362535290176405));
#25988=CARTESIAN_POINT('',(-0.00738804313366706,0.00934286251764274,-0.00206954486922928));
#25989=CARTESIAN_POINT('',(-0.00756101911425425,0.00970961544572337,0.000619317389144314));
#25990=CARTESIAN_POINT('',(-0.00738075226345279,0.00985965447443697,0.00173516988798218));
#25991=CARTESIAN_POINT('',(-0.00697633047987761,0.0100096935031506,0.00276214118473116));
#25992=CARTESIAN_POINT('',(0.00749119806593967,-5.62808667625207E-5,0.000441220987224087));
#25993=CARTESIAN_POINT('',(0.00756203914812496,0.000113760343619128,-0.00080746060603598));
#25994=CARTESIAN_POINT('',(0.00732084563729892,0.000283801554000779,-0.00207466691364739));
#25995=CARTESIAN_POINT('',(0.00610743199459687,0.000670556663749525,-0.00464392565957112));
#25996=CARTESIAN_POINT('',(0.00495273180199492,0.000887270563116618,-0.00586007312960187));
#25997=CARTESIAN_POINT('',(0.00214651787068722,0.00132069836185081,-0.00736652068909999));
#25998=CARTESIAN_POINT('',(0.000495004131981458,0.00153741226121791,-0.00765682077856736));
#25999=CARTESIAN_POINT('',(-0.00265674498019283,0.00197084005995212,-0.00719811128001756));
#26000=CARTESIAN_POINT('',(-0.00415698035366135,0.00218755395931922,-0.00644910169200039));
#26001=CARTESIAN_POINT('',(-0.00641754934095159,0.00262098175805343,-0.00420554291482479));
#26002=CARTESIAN_POINT('',(-0.0071778829547733,0.00283769565742053,-0.00271099372566635));
#26003=CARTESIAN_POINT('',(-0.00766031021750945,0.00327112345615474,0.000437196605863993));
#26004=CARTESIAN_POINT('',(-0.00738240386642389,0.00348783735552185,0.0020908377482359));
#26005=CARTESIAN_POINT('',(-0.00589739492419641,0.00392126515425606,0.00490838178258605));
#26006=CARTESIAN_POINT('',(-0.0046902923330545,0.00413797905362316,0.00607228467456428));
#26007=CARTESIAN_POINT('',(-0.0018205210004546,0.00457140685235737,0.00745366962434564));
#26008=CARTESIAN_POINT('',(-0.000157852258996615,0.00478812075172448,0.00767115168214876));
#26009=CARTESIAN_POINT('',(0.00297067045701477,0.00522154855045868,0.00707436233889838));
#26010=CARTESIAN_POINT('',(0.00443652443156816,0.00543826244982578,0.00626009093784488));
#26011=CARTESIAN_POINT('',(0.00659626057906547,0.00587169024855996,0.00391928943962101));
#26012=CARTESIAN_POINT('',(0.00729014275200938,0.00608840414792706,0.00239275934245064));
#26013=CARTESIAN_POINT('',(0.00763367818756156,0.00652183194666125,-0.000773593346135324));
#26014=CARTESIAN_POINT('',(0.00728333145016984,0.00673854584602832,-0.00241341593755091));
#26015=CARTESIAN_POINT('',(0.00567586981501456,0.0071719736447625,-0.00516294417324391));
#26016=CARTESIAN_POINT('',(0.00441875491725102,0.00738868754412958,-0.00627264981752131));
#26017=CARTESIAN_POINT('',(0.00149102836282355,0.00782211534286372,-0.00752650202389819));
#26018=CARTESIAN_POINT('',(-0.000179583293840374,0.00803882924223079,-0.00767064858599767));
#26019=CARTESIAN_POINT('',(-0.0032788714853909,0.00847225704096491,-0.00693692549391075));
#26020=CARTESIAN_POINT('',(-0.00470754802027749,0.00868897094033197,-0.00605905583972435));
#26021=CARTESIAN_POINT('',(-0.00676215184783665,0.00912239873906607,-0.0036253705705171));
#26022=CARTESIAN_POINT('',(-0.00738807914050922,0.00933911263843312,-0.00206955495549626));
#26023=CARTESIAN_POINT('',(-0.00756105596412327,0.00970586556651375,0.000619320407489371));
#26024=CARTESIAN_POINT('',(-0.00738078823476169,0.00985590459522735,0.00173517834461774));
#26025=CARTESIAN_POINT('',(-0.0069763644801705,0.0100059436239409,0.00276215464648008));
#26026=CARTESIAN_POINT('',(0.00749119806593967,-0.000184931740797058,0.000441220987224088));
#26027=CARTESIAN_POINT('',(0.00756203914812497,-1.48905304154092E-5,-0.000807460606035978));
#26028=CARTESIAN_POINT('',(0.00732084563729892,0.000155150679966243,-0.00207466691364739));
#26029=CARTESIAN_POINT('',(0.00610743199459687,0.000541905789714988,-0.00464392565957112));
#26030=CARTESIAN_POINT('',(0.00495273180199493,0.000758619689082079,-0.00586007312960188));
#26031=CARTESIAN_POINT('',(0.00214651787068723,0.00119204748781627,-0.0073665206891));
#26032=CARTESIAN_POINT('',(0.000495004131981461,0.00140876138718337,-0.00765682077856735));
#26033=CARTESIAN_POINT('',(-0.00265674498019281,0.00184218918591758,-0.00719811128001758));
#26034=CARTESIAN_POINT('',(-0.00415698035366134,0.00205890308528468,-0.00644910169200041));
#26035=CARTESIAN_POINT('',(-0.00641754934095157,0.00249233088401889,-0.0042055429148248));
#26036=CARTESIAN_POINT('',(-0.00717788295477331,0.002709044783386,-0.00271099372566636));
#26037=CARTESIAN_POINT('',(-0.00766031021750946,0.00314247258212021,0.000437196605863996));
#26038=CARTESIAN_POINT('',(-0.00738240386642388,0.00335918648148731,0.00209083774823591));
#26039=CARTESIAN_POINT('',(-0.00589739492419643,0.00379261428022152,0.00490838178258604));
#26040=CARTESIAN_POINT('',(-0.00469029233305451,0.00400932817958862,0.00607228467456427));
#26041=CARTESIAN_POINT('',(-0.00182052100045464,0.00444275597832283,0.00745366962434565));
#26042=CARTESIAN_POINT('',(-0.000157852258996646,0.00465946987768994,0.00767115168214877));
#26043=CARTESIAN_POINT('',(0.00297067045701475,0.00509289767642415,0.00707436233889838));
#26044=CARTESIAN_POINT('',(0.00443652443156816,0.00530961157579124,0.00626009093784489));
#26045=CARTESIAN_POINT('',(0.00659626057906547,0.00574303937452543,0.00391928943962101));
#26046=CARTESIAN_POINT('',(0.00729014275200938,0.00595975327389252,0.00239275934245064));
#26047=CARTESIAN_POINT('',(0.00763367818756156,0.00639318107262671,-0.000773593346135321));
#26048=CARTESIAN_POINT('',(0.00728333145016984,0.00660989497199379,-0.00241341593755092));
#26049=CARTESIAN_POINT('',(0.00567586981501457,0.00704332277072797,-0.00516294417324391));
#26050=CARTESIAN_POINT('',(0.00441875491725102,0.00726003667009504,-0.00627264981752131));
#26051=CARTESIAN_POINT('',(0.00149102836282355,0.00769346446882918,-0.00752650202389819));
#26052=CARTESIAN_POINT('',(-0.000179583293840374,0.00791017836819625,-0.0076706485859977));
#26053=CARTESIAN_POINT('',(-0.0032788714853909,0.00834360616693037,-0.00693692549391075));
#26054=CARTESIAN_POINT('',(-0.00470754802027749,0.00856032006629743,-0.00605905583972436));
#26055=CARTESIAN_POINT('',(-0.00676215184783666,0.00899374786503153,-0.0036253705705171));
#26056=CARTESIAN_POINT('',(-0.00738807914050924,0.00921046176439859,-0.00206955495549626));
#26057=CARTESIAN_POINT('',(-0.00756105596412329,0.00957721469247922,0.000619320407489369));
#26058=CARTESIAN_POINT('',(-0.0073807882347617,0.00972725372119282,0.00173517834461774));
#26059=CARTESIAN_POINT('',(-0.0069763644801705,0.00987729274990641,0.00276215464648008));
#26060=CARTESIAN_POINT('',(0.00745069368358014,-0.000309832735627617,0.000438835336302264));
#26061=CARTESIAN_POINT('',(0.00752115173300428,-0.000139791525245969,-0.000803094723190638));
#26062=CARTESIAN_POINT('',(0.00728126233856912,3.02496851356814E-5,-0.00206344933520408));
#26063=CARTESIAN_POINT('',(0.00607440953829996,0.000417004794884424,-0.00461881627934798));
#26064=CARTESIAN_POINT('',(0.00492595272862557,0.000633718694251518,-0.00582838812533328));
#26065=CARTESIAN_POINT('',(0.00213491179916027,0.00106714649298571,-0.00732669042856967));
#26066=CARTESIAN_POINT('',(0.000492327679369366,0.00128386039235281,-0.00761542088582076));
#26067=CARTESIAN_POINT('',(-0.00264238014648235,0.00171728819108701,-0.00715919159734653));
#26068=CARTESIAN_POINT('',(-0.00413450385254315,0.00193400209045411,-0.00641423185162121));
#26069=CARTESIAN_POINT('',(-0.0063828501019208,0.00236742988918832,-0.00418280383934554));
#26070=CARTESIAN_POINT('',(-0.00713907264523764,0.00258414378855543,-0.0026963355727952));
#26071=CARTESIAN_POINT('',(-0.00761889145761131,0.00301757158728964,0.00043483271448983));
#26072=CARTESIAN_POINT('',(-0.00734248772666813,0.00323428548665675,0.00207953273522452));
#26073=CARTESIAN_POINT('',(-0.00586550812360295,0.00366771328539096,0.00488184250666003));
#26074=CARTESIAN_POINT('',(-0.00466493225148094,0.00388442718475806,0.00603945225736085));
#26075=CARTESIAN_POINT('',(-0.00181067757113305,0.00431785498349227,0.00741336815563682));
#26076=CARTESIAN_POINT('',(-0.000156998762907161,0.00453456888285937,0.00762967430321196));
#26077=CARTESIAN_POINT('',(0.00295460825027614,0.00496799668159358,0.00703611175806975));
#26078=CARTESIAN_POINT('',(0.00441253645523355,0.00518471058096067,0.0062262430653524));
#26079=CARTESIAN_POINT('',(0.0065605950609086,0.00561813837969487,0.00389809811659861));
#26080=CARTESIAN_POINT('',(0.00725072546162622,0.00583485227906196,0.00237982186056218));
#26081=CARTESIAN_POINT('',(0.00759240342518085,0.00626828007779614,-0.000769410581188136));
#26082=CARTESIAN_POINT('',(0.00724395098801784,0.00648499397716323,-0.00240036676690202));
#26083=CARTESIAN_POINT('',(0.00564518078514423,0.0069184217758974,-0.00513502849633172));
#26084=CARTESIAN_POINT('',(0.00439486301943362,0.00713513567526448,-0.00623873404004755));
#26085=CARTESIAN_POINT('',(0.00148296647707642,0.00756856347399862,-0.00748580675551491));
#26086=CARTESIAN_POINT('',(-0.000178612299570156,0.00778527737336569,-0.00762917392726645));
#26087=CARTESIAN_POINT('',(-0.00326114285731525,0.00821870517209982,-0.00689941802446038));
#26088=CARTESIAN_POINT('',(-0.00468209463841377,0.00843541907146688,-0.00602629494990277));
#26089=CARTESIAN_POINT('',(-0.00672558936722847,0.00886884687020098,-0.00360576844619859));
#26090=CARTESIAN_POINT('',(-0.00734813231494467,0.00908556076956803,-0.00205836501705201));
#26091=CARTESIAN_POINT('',(-0.0075201738650095,0.00945231369764866,0.000615971785497641));
#26092=CARTESIAN_POINT('',(-0.00734088083061299,0.00960235272636225,0.00172579635704863));
#26093=CARTESIAN_POINT('',(-0.00693864376688846,0.00975239175507584,0.00274721987009954));
#26094=CARTESIAN_POINT('',(0.00730414745151005,-0.000511926790492136,0.000430203970181813));
#26095=CARTESIAN_POINT('',(0.00737321967538551,-0.000341885580110489,-0.000787298810665295));
#26096=CARTESIAN_POINT('',(0.00713804861837784,-0.00017184436972884,-0.00202286375512473));
#26097=CARTESIAN_POINT('',(0.00595493316902575,0.000214910740019902,-0.00452796968826424));
#26098=CARTESIAN_POINT('',(0.00482906513098801,0.000431624639386996,-0.00571375070295582));
#26099=CARTESIAN_POINT('',(0.00209292063789989,0.000865052438121187,-0.00718258319219017));
#26100=CARTESIAN_POINT('',(0.000482644182849518,0.00108176633748828,-0.00746563466673295));
#26101=CARTESIAN_POINT('',(-0.0025904076898751,0.00151519413622248,-0.00701837886261136));
#26102=CARTESIAN_POINT('',(-0.00405318310754934,0.00173190803558958,-0.00628807158394699));
#26103=CARTESIAN_POINT('',(-0.00625730707572365,0.00216533583432379,-0.00410053309138883));
#26104=CARTESIAN_POINT('',(-0.00699865562622372,0.0023820497336909,-0.00264330187749505));
#26105=CARTESIAN_POINT('',(-0.00746903697652796,0.00281547753242511,0.000426280075152402));
#26106=CARTESIAN_POINT('',(-0.00719806977633214,0.00303219143179222,0.00203863081390608));
#26107=CARTESIAN_POINT('',(-0.00575014059526331,0.00346561923052643,0.0047858225043229));
#26108=CARTESIAN_POINT('',(-0.0045731786143903,0.00368233312989354,0.00592066345598604));
#26109=CARTESIAN_POINT('',(-0.00177506370928174,0.00411576092862775,0.00726755607205175));
#26110=CARTESIAN_POINT('',(-0.000153910785046186,0.00433247482799485,0.00747960773645432));
#26111=CARTESIAN_POINT('',(0.0028964946403615,0.00476590262672905,0.0068977198565423));
#26112=CARTESIAN_POINT('',(0.00432574714153362,0.00498261652609615,0.00610378031222772));
#26113=CARTESIAN_POINT('',(0.00643155600399064,0.00541604432483035,0.00382142718963702));
#26114=CARTESIAN_POINT('',(0.00710811236527552,0.00563275822419744,0.0023330136113609));
#26115=CARTESIAN_POINT('',(0.00744306993200983,0.00606618602293162,-0.000754277195442262));
#26116=CARTESIAN_POINT('',(0.00710147113745925,0.00628289992229871,-0.00235315442396932));
#26117=CARTESIAN_POINT('',(0.00553414683199158,0.00671632772103287,-0.00503402862844448));
#26118=CARTESIAN_POINT('',(0.00430842132107451,0.00693304162039995,-0.00611602560439259));
#26119=CARTESIAN_POINT('',(0.0014537983004299,0.0073664694191341,-0.0073385698913229));
#26120=CARTESIAN_POINT('',(-0.000175099209297627,0.00758318331850117,-0.00747911720230511));
#26121=CARTESIAN_POINT('',(-0.00319700007836367,0.0080166111172353,-0.00676371472515694));
#26122=CARTESIAN_POINT('',(-0.00459000343770219,0.00823332501660236,-0.00590776493702659));
#26123=CARTESIAN_POINT('',(-0.00659330506967508,0.00866675281533646,-0.00353484729416248));
#26124=CARTESIAN_POINT('',(-0.00720360334230944,0.00888346671470351,-0.00201787943942874));
#26125=CARTESIAN_POINT('',(-0.00737226104088444,0.00925021964278414,0.00060385635731609));
#26126=CARTESIAN_POINT('',(-0.00719649448600018,0.00940025867149773,0.00169185200714157));
#26127=CARTESIAN_POINT('',(-0.00680216894415417,0.00955029770021132,0.00269318534154035));
#26128=CARTESIAN_POINT('',(0.00719810560179949,-0.000589119850526096,0.000423958254983186));
#26129=CARTESIAN_POINT('',(0.00726617503288742,-0.000419078640144449,-0.000775868780985295));
#26130=CARTESIAN_POINT('',(0.00703441819691637,-0.000249037429762799,-0.00199349575348868));
#26131=CARTESIAN_POINT('',(0.00586847925604845,0.000137717679985943,-0.00446223247740363));
#26132=CARTESIAN_POINT('',(0.0047589566067198,0.000354431579353036,-0.00563079828484695));
#26133=CARTESIAN_POINT('',(0.00206253554816646,0.000787859378087228,-0.00707830621634101));
#26134=CARTESIAN_POINT('',(0.000475637138941769,0.00100457327745433,-0.00735724834039175));
#26135=CARTESIAN_POINT('',(-0.00255280006697832,0.00143800107618853,-0.00691648581054723));
#26136=CARTESIAN_POINT('',(-0.00399433886367372,0.00165471497555563,-0.00619678115665198));
#26137=CARTESIAN_POINT('',(-0.00616646328855728,0.00208814277428983,-0.00404100141891139));
#26138=CARTESIAN_POINT('',(-0.00689704891674545,0.00230485667365694,-0.00260492633506608));
#26139=CARTESIAN_POINT('',(-0.00736060125534275,0.00273828447239115,0.000420091327189137));
#26140=CARTESIAN_POINT('',(-0.00709356796575188,0.00295499837175826,0.00200903390559903));
#26141=CARTESIAN_POINT('',(-0.00566665986751712,0.00338842617049247,0.00471634177791178));
#26142=CARTESIAN_POINT('',(-0.00450678505887322,0.00360514006985957,0.00583470707181465));
#26143=CARTESIAN_POINT('',(-0.00174929327675202,0.00403856786859379,0.0071620454571755));
#26144=CARTESIAN_POINT('',(-0.000151676303274696,0.00425528176796089,0.00737101854863349));
#26145=CARTESIAN_POINT('',(0.00285444323718545,0.00468870956669509,0.0067975785358435));
#26146=CARTESIAN_POINT('',(0.00426294580416829,0.00490542346606219,0.00601516543159552));
#26147=CARTESIAN_POINT('',(0.00633818246522956,0.00533885126479639,0.00376594758569781));
#26148=CARTESIAN_POINT('',(0.00700491655930799,0.00555556516416348,0.00229914284404808));
#26149=CARTESIAN_POINT('',(0.00733501120121953,0.00598899296289766,-0.000743326574643574));
#26150=CARTESIAN_POINT('',(0.00699837174905264,0.00620570686226475,-0.0023189912516855));
#26151=CARTESIAN_POINT('',(0.00545380190870928,0.00663913466099891,-0.00496094443746942));
#26152=CARTESIAN_POINT('',(0.0042458715205328,0.00685584856036599,-0.00602723294621141));
#26153=CARTESIAN_POINT('',(0.0014326920095305,0.00728927635910014,-0.00723202829551418));
#26154=CARTESIAN_POINT('',(-0.000172557113295315,0.00750599025846721,-0.00737053513607497));
#26155=CARTESIAN_POINT('',(-0.00315058592748773,0.00793941805720134,-0.00666551889530388));
#26156=CARTESIAN_POINT('',(-0.00452336561885433,0.00815613195656839,-0.00582199581397199));
#26157=CARTESIAN_POINT('',(-0.00649758325272985,0.0085895597553025,-0.0034835282664449));
#26158=CARTESIAN_POINT('',(-0.00709902119523878,0.00880627365466954,-0.0019885838002497));
#26159=CARTESIAN_POINT('',(-0.00726523031587315,0.00917302658275018,0.000595089551126265));
#26160=CARTESIAN_POINT('',(-0.00709201554553608,0.00932306561146377,0.00166728964480362));
#26161=CARTESIAN_POINT('',(-0.00670341483470192,0.00947310464017736,0.00265408558936171));
#26162=CARTESIAN_POINT('',(0.00696098881738686,-0.000666312910560056,0.000409992411230955));
#26163=CARTESIAN_POINT('',(0.00702681593563455,-0.000496271700178409,-0.000750310457635969));
#26164=CARTESIAN_POINT('',(0.00680269352999158,-0.000326230489796759,-0.00192782690546716));
#26165=CARTESIAN_POINT('',(0.00567516242971034,6.05246199519836E-5,-0.00431523960526808));
#26166=CARTESIAN_POINT('',(0.0046021891806539,0.000277238519319077,-0.00544531103905756));
#26167=CARTESIAN_POINT('',(0.00199459242202009,0.000710666318053268,-0.00684513580985419));
#26168=CARTESIAN_POINT('',(0.000459968912442717,0.000927380217420367,-0.00711488914686134));
#26169=CARTESIAN_POINT('',(-0.00246870686570896,0.00136080801615457,-0.00668864601969691));
#26170=CARTESIAN_POINT('',(-0.00386275913428326,0.00157752191552167,-0.00599264955552532));
#26171=CARTESIAN_POINT('',(-0.00596333040511978,0.00201094971425588,-0.00390788455243758));
#26172=CARTESIAN_POINT('',(-0.00666984940738199,0.00222766361362299,-0.00251911601352144));
#26173=CARTESIAN_POINT('',(-0.00711813161158341,0.0026610914123572,0.000406252866047666));
#26174=CARTESIAN_POINT('',(-0.00685989481352263,0.0028778053117243,0.00194285320670063));
#26175=CARTESIAN_POINT('',(-0.0054799912854655,0.00331123311045851,0.00456097815053046));
#26176=CARTESIAN_POINT('',(-0.00435832455546914,0.00352794700982562,0.00564250275370733));
#26177=CARTESIAN_POINT('',(-0.00169166883780598,0.00396137480855983,0.00692611654996442));
#26178=CARTESIAN_POINT('',(-0.000146679850139156,0.00417808870792693,0.00712820574304464));
#26179=CARTESIAN_POINT('',(0.00276041344113459,0.00461151650666113,0.00657365573540438));
#26180=CARTESIAN_POINT('',(0.00412251774474152,0.00482823040602823,0.0058170165346839));
#26181=CARTESIAN_POINT('',(0.00612939288526007,0.00526165820476242,0.00364189141992498));
#26182=CARTESIAN_POINT('',(0.00677416372217169,0.00547837210412952,0.00222340550588654));
#26183=CARTESIAN_POINT('',(0.00709338453361007,0.0059117999028637,-0.000718840242141883));
#26184=CARTESIAN_POINT('',(0.00676783450813683,0.00612851380223079,-0.00224260007613187));
#26185=CARTESIAN_POINT('',(0.00527414519860304,0.00656194160096496,-0.00479752321836861));
#26186=CARTESIAN_POINT('',(0.00410600591454249,0.00677865550033204,-0.00582868652661536));
#26187=CARTESIAN_POINT('',(0.00138549690832657,0.00721208329906618,-0.00699379404485457));
#26188=CARTESIAN_POINT('',(-0.000166872813828816,0.00742879719843325,-0.00712773825484702));
#26189=CARTESIAN_POINT('',(-0.0030468007310112,0.00786222499716737,-0.00644594634464542));
#26190=CARTESIAN_POINT('',(-0.0043743589260382,0.00807893889653443,-0.00563021022445137));
#26191=CARTESIAN_POINT('',(-0.00628354276311055,0.00851236669526854,-0.00336877543192919));
#26192=CARTESIAN_POINT('',(-0.00686516840515589,0.00872908059463558,-0.00192307675960106));
#26193=CARTESIAN_POINT('',(-0.00702590233906683,0.00909583352271622,0.000575486376540256));
#26194=CARTESIAN_POINT('',(-0.00685839353244121,0.00924587255142981,0.00161236653292798));
#26195=CARTESIAN_POINT('',(-0.00648259393290923,0.0093959115801434,0.00256665588558687));
#26196=CARTESIAN_POINT('',(0.0068299138826848,-0.000666312910560056,0.000402272282677348));
#26197=CARTESIAN_POINT('',(0.00689450148087976,-0.000496271700178409,-0.000736182163966646));
#26198=CARTESIAN_POINT('',(0.00667459928452825,-0.000326230489796759,-0.00189152605908168));
#26199=CARTESIAN_POINT('',(0.00556829951634954,6.05246199519835E-5,-0.00423398394399313));
#26200=CARTESIAN_POINT('',(0.00451553027885621,0.000277238519319077,-0.00534277621137702));
#26201=CARTESIAN_POINT('',(0.00195703438560715,0.000710666318053268,-0.00671624237921652));
#26202=CARTESIAN_POINT('',(0.000451307729851413,0.000927380217420367,-0.00698091627967214));
#26203=CARTESIAN_POINT('',(-0.00242222128733637,0.00136080801615457,-0.00656269928091072));
#26204=CARTESIAN_POINT('',(-0.00379002364876842,0.00157752191552167,-0.00587980838169368));
#26205=CARTESIAN_POINT('',(-0.00585104130884863,0.00201094971425588,-0.00383429935844122));
#26206=CARTESIAN_POINT('',(-0.00654425660749678,0.00222766361362299,-0.00247168123440579));
#26207=CARTESIAN_POINT('',(-0.00698409768900928,0.0026610914123572,0.000398603152869458));
#26208=CARTESIAN_POINT('',(-0.00673072347187363,0.0028778053117243,0.00190626941610928));
#26209=CARTESIAN_POINT('',(-0.00537680343116006,0.00331123311045851,0.00447509524956026));
#26210=CARTESIAN_POINT('',(-0.00427625760758213,0.00352794700982562,0.00553625481977141));
#26211=CARTESIAN_POINT('',(-0.00165981483138966,0.00396137480855983,0.00679569825762958));
#26212=CARTESIAN_POINT('',(-0.000143917878775103,0.00417808870792693,0.00699398212527661));
#26213=CARTESIAN_POINT('',(0.00270843504825977,0.00461151650666113,0.00644987425566405));
#26214=CARTESIAN_POINT('',(0.00404489102268007,0.00482823040602823,0.00570748251840448));
#26215=CARTESIAN_POINT('',(0.00601397684405166,0.00526165820476243,0.00357331485809136));
#26216=CARTESIAN_POINT('',(0.00664660669100294,0.00547837210412952,0.00218153893503782));
#26217=CARTESIAN_POINT('',(0.00695981659679091,0.0059117999028637,-0.000705304530438881));
#26218=CARTESIAN_POINT('',(0.00664039665562761,0.00612851380223079,-0.00220037207286204));
#26219=CARTESIAN_POINT('',(0.0051748334117791,0.00656194160096496,-0.00470718619024285));
#26220=CARTESIAN_POINT('',(0.0040286901090939,0.00677865550033204,-0.00571893276520051));
#26221=CARTESIAN_POINT('',(0.00135940809802203,0.00721208329906618,-0.00686210139000368));
#26222=CARTESIAN_POINT('',(-0.00016373061036463,0.00742879719843325,-0.00699352343984919));
#26223=CARTESIAN_POINT('',(-0.00298942968541062,0.00786222499716738,-0.00632456962384003));
#26224=CARTESIAN_POINT('',(-0.00429199005206994,0.00807893889653443,-0.00552419375798534));
#26225=CARTESIAN_POINT('',(-0.00616522409043646,0.00851236669526854,-0.00330534162513106));
#26226=CARTESIAN_POINT('',(-0.00673589776214366,0.00872908059463559,-0.00188686535813147));
#26227=CARTESIAN_POINT('',(-0.00689360508727178,0.00909583352271622,0.00056465000814407));
#26228=CARTESIAN_POINT('',(-0.00672925045981043,0.00924587255142981,0.00158200578339029));
#26229=CARTESIAN_POINT('',(-0.00636052714056878,0.0093959115801434,0.00251832593399067));
#26230=CARTESIAN_POINT('',(0.00659279709827217,-0.000589119850526096,0.000388306438925115));
#26231=CARTESIAN_POINT('',(0.00665514238362688,-0.000419078640144449,-0.000710623840617322));
#26232=CARTESIAN_POINT('',(0.00644287461760345,-0.000249037429762799,-0.00182585721106015));
#26233=CARTESIAN_POINT('',(0.00537498269001143,0.000137717679985943,-0.00408699107185757));
#26234=CARTESIAN_POINT('',(0.00435876285279031,0.000354431579353036,-0.00515728896558762));
#26235=CARTESIAN_POINT('',(0.00188909125946077,0.000787859378087228,-0.0064830719727297));
#26236=CARTESIAN_POINT('',(0.000435639503352361,0.00100457327745433,-0.00673855708614173));
#26237=CARTESIAN_POINT('',(-0.00233812808606701,0.00143800107618853,-0.0063348594900604));
#26238=CARTESIAN_POINT('',(-0.00365844391937797,0.00165471497555563,-0.00567567678056703));
#26239=CARTESIAN_POINT('',(-0.00564790842541112,0.00208814277428983,-0.00370118249196741));
#26240=CARTESIAN_POINT('',(-0.00631705709813331,0.00230485667365694,-0.00238587091286116));
#26241=CARTESIAN_POINT('',(-0.00674162804524994,0.00273828447239115,0.000384764691727985));
#26242=CARTESIAN_POINT('',(-0.00649705031964438,0.00295499837175826,0.00184008871721088));
#26243=CARTESIAN_POINT('',(-0.00519013484910844,0.00338842617049247,0.00431973162217894));
#26244=CARTESIAN_POINT('',(-0.00412779710417805,0.00360514006985957,0.0053440505016641));
#26245=CARTESIAN_POINT('',(-0.00160219039244362,0.00403856786859379,0.0065597693504185));
#26246=CARTESIAN_POINT('',(-0.000138921425639559,0.00425528176796089,0.00675116931968775));
#26247=CARTESIAN_POINT('',(0.0026144052522089,0.00468870956669509,0.00622595145522493));
#26248=CARTESIAN_POINT('',(0.00390446296325331,0.00490542346606219,0.00550933362149286));
#26249=CARTESIAN_POINT('',(0.00580518726408218,0.00533885126479638,0.00344925869231854));
#26250=CARTESIAN_POINT('',(0.00641585385386665,0.00555556516416348,0.00210580159687627));
#26251=CARTESIAN_POINT('',(0.00671818992918146,0.00598899296289766,-0.000680818197937192));
#26252=CARTESIAN_POINT('',(0.0064098594147118,0.00620570686226475,-0.0021239808973084));
#26253=CARTESIAN_POINT('',(0.00499517670167286,0.00663913466099892,-0.00454376497114204));
#26254=CARTESIAN_POINT('',(0.00388882450310359,0.00685584856036599,-0.00552038634560447));
#26255=CARTESIAN_POINT('',(0.00131221299681809,0.00728927635910014,-0.00662386713934407));
#26256=CARTESIAN_POINT('',(-0.000158046310898131,0.00750599025846721,-0.00675072655862124));
#26257=CARTESIAN_POINT('',(-0.00288564448893408,0.00793941805720134,-0.00610499707318157));
#26258=CARTESIAN_POINT('',(-0.00414298335925381,0.0081561319565684,-0.00533240816846472));
#26259=CARTESIAN_POINT('',(-0.00595118360081716,0.0085895597553025,-0.00319058879061535));
#26260=CARTESIAN_POINT('',(-0.00650204497206078,0.00880627365466955,-0.00182135831748283));
#26261=CARTESIAN_POINT('',(-0.00665427711046546,0.00917302658275018,0.000545046833558058));
#26262=CARTESIAN_POINT('',(-0.00649562844671556,0.00932306561146377,0.00152708267151465));
#26263=CARTESIAN_POINT('',(-0.00613970623877609,0.00947310464017736,0.00243089623021583));
#26264=CARTESIAN_POINT('',(0.00648675524856161,-0.000511926790492136,0.000382060723726489));
#26265=CARTESIAN_POINT('',(0.0065480977411288,-0.000341885580110489,-0.00069919381093732));
#26266=CARTESIAN_POINT('',(0.00633924419614199,-0.00017184436972884,-0.0017964892094241));
#26267=CARTESIAN_POINT('',(0.00528852877703413,0.000214910740019903,-0.00402125386099697));
#26268=CARTESIAN_POINT('',(0.00428865432852211,0.000431624639386996,-0.00507433654747875));
#26269=CARTESIAN_POINT('',(0.00185870616972735,0.000865052438121187,-0.00637879499688054));
#26270=CARTESIAN_POINT('',(0.000428632459444612,0.00108176633748828,-0.00663017075980053));
#26271=CARTESIAN_POINT('',(-0.00230052046317024,0.00151519413622248,-0.00623296643799627));
#26272=CARTESIAN_POINT('',(-0.00359959967550236,0.00173190803558958,-0.00558438635327201));
#26273=CARTESIAN_POINT('',(-0.00555706463824476,0.00216533583432379,-0.00364165081948996));
#26274=CARTESIAN_POINT('',(-0.00621545038865505,0.0023820497336909,-0.00234749537043218));
#26275=CARTESIAN_POINT('',(-0.00663319232406474,0.00281547753242511,0.000378575943764719));
#26276=CARTESIAN_POINT('',(-0.00639254850906414,0.00303219143179222,0.00181049180890383));
#26277=CARTESIAN_POINT('',(-0.00510665412136226,0.00346561923052643,0.00425025089576781));
#26278=CARTESIAN_POINT('',(-0.00406140354866099,0.00368233312989354,0.00525809411749271));
#26279=CARTESIAN_POINT('',(-0.00157641995991389,0.00411576092862774,0.00645425873554226));
#26280=CARTESIAN_POINT('',(-0.000136686943868066,0.00433247482799485,0.00664258013186692));
#26281=CARTESIAN_POINT('',(0.00257235384903287,0.00476590262672905,0.00612581013452613));
#26282=CARTESIAN_POINT('',(0.00384166162588797,0.00498261652609615,0.00542071874086066));
#26283=CARTESIAN_POINT('',(0.00571181372532109,0.00541604432483035,0.00339377908837933));
#26284=CARTESIAN_POINT('',(0.00631265804789911,0.00563275822419744,0.00207193082956346));
#26285=CARTESIAN_POINT('',(0.00661013119839116,0.00606618602293162,-0.000669867577138504));
#26286=CARTESIAN_POINT('',(0.0063067600263052,0.00628289992229871,-0.00208981772502459));
#26287=CARTESIAN_POINT('',(0.00491483177839056,0.00671632772103287,-0.00447068078016699));
#26288=CARTESIAN_POINT('',(0.00382627470256189,0.00693304162039996,-0.00543159368742329));
#26289=CARTESIAN_POINT('',(0.0012911067059187,0.0073664694191341,-0.00651732554353535));
#26290=CARTESIAN_POINT('',(-0.00015550421489582,0.00758318331850118,-0.00664214449239111));
#26291=CARTESIAN_POINT('',(-0.00283923033805814,0.0080166111172353,-0.0060068012433285));
#26292=CARTESIAN_POINT('',(-0.00407634554040595,0.00823332501660236,-0.00524663904541012));
#26293=CARTESIAN_POINT('',(-0.00585546178387193,0.00866675281533646,-0.00313926976289777));
#26294=CARTESIAN_POINT('',(-0.00639746282499011,0.00888346671470351,-0.00179206267830379));
#26295=CARTESIAN_POINT('',(-0.00654724638545417,0.00925021964278415,0.000536280027368236));
#26296=CARTESIAN_POINT('',(-0.00639114950625147,0.00940025867149774,0.0015025203091767));
#26297=CARTESIAN_POINT('',(-0.00604095212932383,0.00955029770021133,0.00239179647803719));
#26298=CARTESIAN_POINT('',(0.00634020901649153,-0.000309832735627617,0.000373429357606039));
#26299=CARTESIAN_POINT('',(0.00640016568351004,-0.000139791525245969,-0.000683397898411977));
#26300=CARTESIAN_POINT('',(0.00619603047595072,3.0249685135681E-5,-0.00175590362934475));
#26301=CARTESIAN_POINT('',(0.00516905240775992,0.000417004794884424,-0.00393040726991323));
#26302=CARTESIAN_POINT('',(0.00419176673088455,0.000633718694251517,-0.0049596991251013));
#26303=CARTESIAN_POINT('',(0.00181671500846697,0.00106714649298571,-0.00623468776050105));
#26304=CARTESIAN_POINT('',(0.000418948962924764,0.00128386039235281,-0.00648038454071273));
#26305=CARTESIAN_POINT('',(-0.00224854800656299,0.00171728819108701,-0.0060921537032611));
#26306=CARTESIAN_POINT('',(-0.00351827893050854,0.00193400209045412,-0.0054582260855978));
#26307=CARTESIAN_POINT('',(-0.0054315216120476,0.00236742988918832,-0.00355938007153327));
#26308=CARTESIAN_POINT('',(-0.00607503336964112,0.00258414378855543,-0.00229446167513204));
#26309=CARTESIAN_POINT('',(-0.00648333784298138,0.00301757158728964,0.000370023304427295));
#26310=CARTESIAN_POINT('',(-0.00624813055872813,0.00323428548665674,0.00176958988758539));
#26311=CARTESIAN_POINT('',(-0.0049912865930226,0.00366771328539096,0.00415423089343069));
#26312=CARTESIAN_POINT('',(-0.00396964991157034,0.00388442718475806,0.00513930531611789));
#26313=CARTESIAN_POINT('',(-0.00154080609806258,0.00431785498349227,0.00630844665195719));
#26314=CARTESIAN_POINT('',(-0.000133598966007101,0.00453456888285937,0.00649251356510929));
#26315=CARTESIAN_POINT('',(0.00251424023911821,0.00496799668159358,0.00598741823299868));
#26316=CARTESIAN_POINT('',(0.00375487231218804,0.00518471058096067,0.00529825598773598));
#26317=CARTESIAN_POINT('',(0.00558277466840314,0.00561813837969487,0.00331710816141773));
#26318=CARTESIAN_POINT('',(0.00617004495154841,0.00583485227906196,0.00202512258036218));
#26319=CARTESIAN_POINT('',(0.00646079770522014,0.00626828007779614,-0.000654734191392628));
#26320=CARTESIAN_POINT('',(0.0061642801757466,0.00648499397716323,-0.00204260538209188));
#26321=CARTESIAN_POINT('',(0.00480379782523792,0.00691842177589739,-0.00436968091227974));
#26322=CARTESIAN_POINT('',(0.00373983300420278,0.00713513567526448,-0.00530888525176834));
#26323=CARTESIAN_POINT('',(0.00126193852927218,0.00756856347399863,-0.00637008867934335));
#26324=CARTESIAN_POINT('',(-0.00015199112462329,0.00778527737336569,-0.00649208776742977));
#26325=CARTESIAN_POINT('',(-0.00277508755910656,0.00821870517209982,-0.00587109794402506));
#26326=CARTESIAN_POINT('',(-0.00398425433969437,0.00843541907146687,-0.00512810903253394));
#26327=CARTESIAN_POINT('',(-0.00572317748631853,0.00886884687020098,-0.00306834861086167));
#26328=CARTESIAN_POINT('',(-0.00625293385235488,0.00908556076956803,-0.00175157710068052));
#26329=CARTESIAN_POINT('',(-0.00639933356132911,0.00945231369764866,0.000524164599186684));
#26330=CARTESIAN_POINT('',(-0.00624676316163866,0.00960235272636225,0.00146857595926964));
#26331=CARTESIAN_POINT('',(-0.00590447730658955,0.00975239175507584,0.00233776194947801));
#26332=CARTESIAN_POINT('',(0.00629970463413201,-0.000184931740797059,0.000371043706684215));
#26333=CARTESIAN_POINT('',(0.00635927826838935,-1.48905304154102E-5,-0.000679032015566637));
#26334=CARTESIAN_POINT('',(0.00615644717722092,0.000155150679966241,-0.00174468605090144));
#26335=CARTESIAN_POINT('',(0.00513602995146302,0.000541905789714986,-0.00390529788969009));
#26336=CARTESIAN_POINT('',(0.00416498765751519,0.00075861968908208,-0.00492801412083271));
#26337=CARTESIAN_POINT('',(0.00180510893694002,0.00119204748781627,-0.00619485749997073));
#26338=CARTESIAN_POINT('',(0.000416272510312666,0.00140876138718337,-0.00643898464796613));
#26339=CARTESIAN_POINT('',(-0.00223418317285251,0.00184218918591758,-0.00605323402059007));
#26340=CARTESIAN_POINT('',(-0.00349580242939034,0.00205890308528468,-0.00542335624521861));
#26341=CARTESIAN_POINT('',(-0.00539682237301682,0.00249233088401889,-0.00353664099605402));
#26342=CARTESIAN_POINT('',(-0.00603622306010546,0.002709044783386,-0.00227980352226088));
#26343=CARTESIAN_POINT('',(-0.00644191908308324,0.00314247258212021,0.000367659413053137));
#26344=CARTESIAN_POINT('',(-0.00620821441897237,0.00335918648148731,0.00175828487457401));
#26345=CARTESIAN_POINT('',(-0.00495939979242913,0.00379261428022152,0.00412769161750468));
#26346=CARTESIAN_POINT('',(-0.00394428982999677,0.00400932817958863,0.00510647289891446));
#26347=CARTESIAN_POINT('',(-0.00153096266874102,0.00444275597832284,0.00626814518324836));
#26348=CARTESIAN_POINT('',(-0.000132745469917628,0.00465946987768994,0.00645103618617248));
#26349=CARTESIAN_POINT('',(0.00249817803237959,0.00509289767642414,0.00594916765217005));
#26350=CARTESIAN_POINT('',(0.00373088433585343,0.00530961157579123,0.0052644081152435));
#26351=CARTESIAN_POINT('',(0.00554710915024626,0.00574303937452542,0.00329591683839534));
#26352=CARTESIAN_POINT('',(0.00613062766116525,0.00595975327389252,0.00201218509847372));
#26353=CARTESIAN_POINT('',(0.00641952294283942,0.0063931810726267,-0.000650551426445439));
#26354=CARTESIAN_POINT('',(0.0061248997135946,0.00660989497199379,-0.00202955621144299));
#26355=CARTESIAN_POINT('',(0.00477310879536758,0.00704332277072796,-0.00434176523536755));
#26356=CARTESIAN_POINT('',(0.00371594110638537,0.00726003667009504,-0.00527496947429457));
#26357=CARTESIAN_POINT('',(0.00125387664352505,0.00769346446882918,-0.00632939341096007));
#26358=CARTESIAN_POINT('',(-0.00015102013035307,0.00791017836819625,-0.00645061310869855));
#26359=CARTESIAN_POINT('',(-0.00275735893103092,0.00834360616693037,-0.0058335904745747));
#26360=CARTESIAN_POINT('',(-0.00395880095783066,0.00856032006629742,-0.00509534814271236));
#26361=CARTESIAN_POINT('',(-0.00568661500571035,0.00899374786503153,-0.00304874648654315));
#26362=CARTESIAN_POINT('',(-0.00621298702679032,0.00921046176439858,-0.00174038716223627));
#26363=CARTESIAN_POINT('',(-0.00635845146221533,0.00957721469247922,0.000520815977194954));
#26364=CARTESIAN_POINT('',(-0.00620685575748995,0.0097272537211928,0.00145919397170054));
#26365=CARTESIAN_POINT('',(-0.00586675659330751,0.00987729274990639,0.00232282717309746));
#26366=CARTESIAN_POINT('',(0.00629970463413201,-5.62808667607383E-5,0.000371043706684215));
#26367=CARTESIAN_POINT('',(0.00635927826838935,0.00011376034362091,-0.000679032015566637));
#26368=CARTESIAN_POINT('',(0.00615644717722091,0.000283801554002562,-0.00174468605090144));
#26369=CARTESIAN_POINT('',(0.00513602995146302,0.000670556663751307,-0.00390529788969009));
#26370=CARTESIAN_POINT('',(0.00416498765751519,0.000887270563118401,-0.00492801412083271));
#26371=CARTESIAN_POINT('',(0.00180510893694002,0.00132069836185259,-0.00619485749997072));
#26372=CARTESIAN_POINT('',(0.000416272510312665,0.00153741226121969,-0.00643898464796613));
#26373=CARTESIAN_POINT('',(-0.00223418317285251,0.0019708400599539,-0.00605323402059007));
#26374=CARTESIAN_POINT('',(-0.00349580242939034,0.002187553959321,-0.00542335624521861));
#26375=CARTESIAN_POINT('',(-0.00539682237301682,0.00262098175805521,-0.00353664099605401));
#26376=CARTESIAN_POINT('',(-0.00603622306010547,0.00283769565742231,-0.00227980352226088));
#26377=CARTESIAN_POINT('',(-0.00644191908308324,0.00327112345615653,0.000367659413053137));
#26378=CARTESIAN_POINT('',(-0.00620821441897237,0.00348783735552363,0.00175828487457401));
#26379=CARTESIAN_POINT('',(-0.00495939979242914,0.00392126515425784,0.00412769161750468));
#26380=CARTESIAN_POINT('',(-0.00394428982999677,0.00413797905362495,0.00510647289891447));
#26381=CARTESIAN_POINT('',(-0.00153096266874101,0.00457140685235916,0.00626814518324837));
#26382=CARTESIAN_POINT('',(-0.000132745469917627,0.00478812075172626,0.00645103618617248));
#26383=CARTESIAN_POINT('',(0.00249817803237959,0.00522154855046046,0.00594916765217005));
#26384=CARTESIAN_POINT('',(0.00373088433585343,0.00543826244982756,0.0052644081152435));
#26385=CARTESIAN_POINT('',(0.00554710915024626,0.00587169024856175,0.00329591683839534));
#26386=CARTESIAN_POINT('',(0.00613062766116525,0.00608840414792885,0.00201218509847372));
#26387=CARTESIAN_POINT('',(0.00641952294283942,0.00652183194666303,-0.000650551426445441));
#26388=CARTESIAN_POINT('',(0.0061248997135946,0.00673854584603012,-0.00202955621144299));
#26389=CARTESIAN_POINT('',(0.00477310879536758,0.00717197364476428,-0.00434176523536755));
#26390=CARTESIAN_POINT('',(0.00371594110638537,0.00738868754413136,-0.00527496947429457));
#26391=CARTESIAN_POINT('',(0.00125387664352505,0.00782211534286551,-0.00632939341096007));
#26392=CARTESIAN_POINT('',(-0.000151020130353072,0.00803882924223258,-0.00645061310869855));
#26393=CARTESIAN_POINT('',(-0.00275735893103092,0.0084722570409667,-0.0058335904745747));
#26394=CARTESIAN_POINT('',(-0.00395880095783065,0.00868897094033375,-0.00509534814271236));
#26395=CARTESIAN_POINT('',(-0.00568661500571035,0.00912239873906786,-0.00304874648654315));
#26396=CARTESIAN_POINT('',(-0.00621298702679033,0.00933911263843491,-0.00174038716223628));
#26397=CARTESIAN_POINT('',(-0.00635845146221534,0.00970586556651554,0.000520815977194954));
#26398=CARTESIAN_POINT('',(-0.00620685575748996,0.00985590459522913,0.00145919397170054));
#26399=CARTESIAN_POINT('',(-0.00586675659330751,0.0100059436239427,0.00232282717309746));
#26400=CARTESIAN_POINT('',(0.00629974114353878,-5.25309875491508E-5,0.000371045857036716));
#26401=CARTESIAN_POINT('',(0.0063593151230501,0.000117510222832498,-0.000679035950839401));
#26402=CARTESIAN_POINT('',(0.00615648285639118,0.000287551433214149,-0.00174469616208227));
#26403=CARTESIAN_POINT('',(0.00513605971689134,0.000674306542962894,-0.00390532052251457));
#26404=CARTESIAN_POINT('',(0.00416501179534981,0.000891020442329988,-0.00492804268072283));
#26405=CARTESIAN_POINT('',(0.00180511939829658,0.00132444824106418,-0.00619489340174477));
#26406=CARTESIAN_POINT('',(0.000416274922784883,0.00154116214043128,-0.00643902196455848));
#26407=CARTESIAN_POINT('',(-0.00223419612087262,0.00197458993916549,-0.0060532691015972));
#26408=CARTESIAN_POINT('',(-0.00349582268901842,0.00219130383853259,-0.00542338767582222));
#26409=CARTESIAN_POINT('',(-0.00539685364984562,0.0026247316372668,-0.00353666149235856));
#26410=CARTESIAN_POINT('',(-0.00603625804252701,0.0028414455366339,-0.00227981673466987));
#26411=CARTESIAN_POINT('',(-0.00644195641668186,0.00327487333536811,0.000367661543792251));
#26412=CARTESIAN_POINT('',(-0.00620825039815532,0.00349158723473522,0.00175829506456568));
#26413=CARTESIAN_POINT('',(-0.00495942853421227,0.00392501503346943,0.00412771553919324));
#26414=CARTESIAN_POINT('',(-0.00394431268879574,0.00414172893283653,0.00510650249304738));
#26415=CARTESIAN_POINT('',(-0.00153097154130601,0.00457515673157075,0.00626818150975501));
#26416=CARTESIAN_POINT('',(-0.0001327462392328,0.00479187063093785,0.0064510735726085));
#26417=CARTESIAN_POINT('',(0.00249819251035964,0.00522529842967205,0.00594920213006932));
#26418=CARTESIAN_POINT('',(0.00373090595787887,0.00544201232903915,0.00526443862467663));
#26419=CARTESIAN_POINT('',(0.0055471412980494,0.00587544012777333,0.00329593593960333));
#26420=CARTESIAN_POINT('',(0.00613066319070069,0.00609215402714043,0.00201219675992271));
#26421=CARTESIAN_POINT('',(0.00641956014664309,0.00652558182587462,-0.000650555196661354));
#26422=CARTESIAN_POINT('',(0.00612493520993421,0.0067422957252417,-0.0020295679735648));
#26423=CARTESIAN_POINT('',(0.00477313645751695,0.00717572352397587,-0.00434179039770171));
#26424=CARTESIAN_POINT('',(0.00371596264180859,0.00739243742334294,-0.00527500004493517));
#26425=CARTESIAN_POINT('',(0.00125388391026136,0.0078258652220771,-0.00632943009242565));
#26426=CARTESIAN_POINT('',(-0.000151021005577498,0.00804257912144416,-0.00645065049268266));
#26427=CARTESIAN_POINT('',(-0.002757374911072,0.00847600692017828,-0.00583362428265618));
#26428=CARTESIAN_POINT('',(-0.00395882390072764,0.00869272081954534,-0.00509537767237269));
#26429=CARTESIAN_POINT('',(-0.0056866479620079,0.00912614861827944,-0.00304876415529623));
#26430=CARTESIAN_POINT('',(-0.00621302303363253,0.00934286251764649,-0.00174039724850326));
#26431=CARTESIAN_POINT('',(-0.0063584883120844,0.00970961544572712,0.000520818995540014));
#26432=CARTESIAN_POINT('',(-0.0062068917287989,0.00985965447444072,0.0014592024283361));
#26433=CARTESIAN_POINT('',(-0.00586679059360044,0.0100096935031543,0.0023228406348464));
#26434=CARTESIAN_POINT('',(0.00629981395301298,-4.87817538653648E-5,0.000371050145411927));
#26435=CARTESIAN_POINT('',(0.0063593886210526,0.000121259456516284,-0.000679043798820677));
#26436=CARTESIAN_POINT('',(0.00615655401015281,0.000291300666897935,-0.00174471632646797));
#26437=CARTESIAN_POINT('',(0.00513611907707756,0.00067805577664668,-0.00390536565839037));
#26438=CARTESIAN_POINT('',(0.00416505993261639,0.000894769676013774,-0.00492809963674502));
#26439=CARTESIAN_POINT('',(0.0018051402610259,0.00132819747474797,-0.0061949649994376));
#26440=CARTESIAN_POINT('',(0.000416279733896571,0.00154491137411507,-0.00643909638377553));
#26441=CARTESIAN_POINT('',(-0.00223422194267086,0.00197833917284927,-0.00605333906246232));
#26442=CARTESIAN_POINT('',(-0.00349586309210897,0.00219505307221637,-0.00542345035681118));
#26443=CARTESIAN_POINT('',(-0.00539691602416666,0.00262848087095058,-0.00353670236744498));
#26444=CARTESIAN_POINT('',(-0.00603632780678623,0.00284519477031769,-0.00227984308372992));
#26445=CARTESIAN_POINT('',(-0.00644203086981395,0.0032786225690519,0.000367665793053145));
#26446=CARTESIAN_POINT('',(-0.00620832215022209,0.00349533646841901,0.00175831538612116));
#26447=CARTESIAN_POINT('',(-0.00495948585297754,0.00392876426715322,0.00412776324540707));
#26448=CARTESIAN_POINT('',(-0.00394435827532484,0.00414547816652032,0.00510656151162497));
#26449=CARTESIAN_POINT('',(-0.00153098923556207,0.00457890596525453,0.00626825395447765));
#26450=CARTESIAN_POINT('',(-0.00013274777345201,0.00479561986462163,0.00645114813111243));
#26451=CARTESIAN_POINT('',(0.00249822138330521,0.00522904766335583,0.00594927088817685));
#26452=CARTESIAN_POINT('',(0.00373094907795236,0.00544576156272293,0.00526449946860648));
#26453=CARTESIAN_POINT('',(0.00554720540932508,0.00587918936145712,0.00329597403249593));
#26454=CARTESIAN_POINT('',(0.00613073404605065,0.00609590326082422,0.00201222001595574));
#26455=CARTESIAN_POINT('',(0.00641963434092953,0.0065293310595584,-0.000650562715475337));
#26456=CARTESIAN_POINT('',(0.00612500599908283,0.00674604495892549,-0.00202959143036622));
#26457=CARTESIAN_POINT('',(0.00477319162320516,0.00717947275765965,-0.00434184057809305));
#26458=CARTESIAN_POINT('',(0.00371600558917419,0.00739618665702673,-0.00527506101092899));
#26459=CARTESIAN_POINT('',(0.00125389840206763,0.00782961445576088,-0.00632950324503089));
#26460=CARTESIAN_POINT('',(-0.000151022751007946,0.00804632835512795,-0.00645072504629683));
#26461=CARTESIAN_POINT('',(-0.00275740677952704,0.00847975615386207,-0.00583369170496878));
#26462=CARTESIAN_POINT('',(-0.00395886965497057,0.00869647005322912,-0.00509543656237478));
#26463=CARTESIAN_POINT('',(-0.00568671368563664,0.00912989785196323,-0.00304879939149245));
#26464=CARTESIAN_POINT('',(-0.00621309484085919,0.00934661175133028,-0.00174041736320412));
#26465=CARTESIAN_POINT('',(-0.00635856180053102,0.00971336467941091,0.000520825014923407));
#26466=CARTESIAN_POINT('',(-0.0062069634651628,0.00986340370812451,0.00145921929311818));
#26467=CARTESIAN_POINT('',(-0.00586685839923381,0.0100134427368381,0.00232286748115665));
#26468=CARTESIAN_POINT('',(-0.00697636803347297,0.0100021874430334,0.00276214562330082));
#26469=CARTESIAN_POINT('',(-0.00753804382756523,0.00979380836024526,0.00133584489681522));
#26470=CARTESIAN_POINT('',(-0.00776779845912848,0.00937705019466896,-0.00186177246719335));
#26471=CARTESIAN_POINT('',(-0.00528323152104243,0.00875191294630448,-0.00599199413777197));
#26472=CARTESIAN_POINT('',(-0.00087751154538944,0.00812677569793997,-0.0079400821121839));
#26473=CARTESIAN_POINT('',(0.0038480746341964,0.00750163844957543,-0.00700128379985256));
#26474=CARTESIAN_POINT('',(0.0071744693740918,0.00687650120121086,-0.00351543059877151));
#26475=CARTESIAN_POINT('',(0.0078914902835435,0.00625136395284629,0.00124942414839732));
#26476=CARTESIAN_POINT('',(0.00573800816630541,0.00562622670448166,0.005560182342935));
#26477=CARTESIAN_POINT('',(0.0014971987061511,0.00500108945611705,0.00784857616645092));
#26478=CARTESIAN_POINT('',(-0.00328822052470963,0.00437595220775241,0.00728203066161055));
#26479=CARTESIAN_POINT('',(-0.00687737560563289,0.00375081495938778,0.00406674111468162));
#26480=CARTESIAN_POINT('',(-0.00796476957421187,0.00312567771102313,-0.000627461007861309));
#26481=CARTESIAN_POINT('',(-0.00615519713512889,0.00250054046265849,-0.00509305407738273));
#26482=CARTESIAN_POINT('',(-0.00210705476033651,0.00187540321429386,-0.00770553365716223));
#26483=CARTESIAN_POINT('',(0.00270641916035431,0.00125026596592923,-0.00751610423345641));
#26484=CARTESIAN_POINT('',(0.00653694894897428,0.000625128717564618,-0.00459055394770496));
#26485=CARTESIAN_POINT('',(0.0075004521700649,0.000208370551988218,-0.00153290696293537));
#26486=CARTESIAN_POINT('',(0.00750327649637306,-8.53079997731299E-9,5.83687127765024E-10));
#26487=CARTESIAN_POINT('',(0.00630986196639554,-9.03189203241712E-9,3.59078576052906E-9));
#26488=CARTESIAN_POINT('',(0.00630748748308214,0.000208370074868084,-0.00128909129339307));
#26489=CARTESIAN_POINT('',(0.00549723302828212,0.000625128288388326,-0.0038604125171732));
#26490=CARTESIAN_POINT('',(0.00227595940277768,0.0012502656086687,-0.00632064842559635));
#26491=CARTESIAN_POINT('',(-0.00177191976628907,0.00187540292894909,-0.00647995041664462));
#26492=CARTESIAN_POINT('',(-0.00517619621271276,0.00250054024922949,-0.00428299345973494));
#26493=CARTESIAN_POINT('',(-0.00669795326198427,0.0031256775695099,-0.000527664383287013));
#26494=CARTESIAN_POINT('',(-0.0057835134182492,0.0037508148897903,0.00341991386813026));
#26495=CARTESIAN_POINT('',(-0.00276522310213338,0.0043759522100707,0.00612380489522609));
#26496=CARTESIAN_POINT('',(0.00125906345149119,0.0050010895303511,0.00660024130588146));
#26497=CARTESIAN_POINT('',(0.00482536249576932,0.00562622685063147,0.00467582317649158));
#26498=CARTESIAN_POINT('',(0.00663632912242476,0.00625136417091186,0.00105070204310645));
#26499=CARTESIAN_POINT('',(0.00603335321048816,0.00687650149119221,-0.00295629117688575));
#26500=CARTESIAN_POINT('',(0.0032360303450091,0.00750163881147252,-0.00588771168090631));
#26501=CARTESIAN_POINT('',(-0.000737939723699143,0.00812677613175284,-0.00667719275794199));
#26502=CARTESIAN_POINT('',(-0.00444291960613415,0.00875191345203308,-0.00503895366700153));
#26503=CARTESIAN_POINT('',(-0.00653231080331541,0.00937705077231335,-0.00156565414967004));
#26504=CARTESIAN_POINT('',(-0.00633909965413823,0.00979380898583348,0.00112337445858087));
#26505=CARTESIAN_POINT('',(-0.00586675994202744,0.0100021880925935,0.00232281866952534));
#26506=CARTESIAN_POINT('',(0.00629981376813919,-7.12754161583918E-5,0.000371050098800527));
#26507=CARTESIAN_POINT('',(0.00635938760157998,9.87634366672949E-5,-0.000679029292887613));
#26508=CARTESIAN_POINT('',(0.0061565597919047,0.000268802289492985,-0.00174468683320115));
#26509=CARTESIAN_POINT('',(0.00513614563794227,0.000655555202048129,-0.00390533092155032));
#26510=CARTESIAN_POINT('',(0.00416509255857977,0.000872269261777583,-0.00492807221758922));
#26511=CARTESIAN_POINT('',(0.00180517935721193,0.0013056973812365,-0.00619495373145521));
#26512=CARTESIAN_POINT('',(0.00041631923520657,0.00152241144096596,-0.00643909394928229));
#26513=CARTESIAN_POINT('',(-0.00223418666799694,0.00195583956042489,-0.00605335220863278));
#26514=CARTESIAN_POINT('',(-0.0034958324491951,0.00217255362015435,-0.00542347025015618));
#26515=CARTESIAN_POINT('',(-0.00539689715743606,0.00260598173961328,-0.00353673137452573));
#26516=CARTESIAN_POINT('',(-0.00603631608447885,0.00282269579934275,-0.00227987445737188));
#26517=CARTESIAN_POINT('',(-0.00644203278688762,0.00325612391880168,0.000367634290427892));
#26518=CARTESIAN_POINT('',(-0.0062083305622536,0.00347283797853115,0.00175828612107382));
#26519=CARTESIAN_POINT('',(-0.00495950418817836,0.00390626609799008,0.00412774140168303));
#26520=CARTESIAN_POINT('',(-0.00394438003873714,0.00412298015771955,0.00510654485164633));
#26521=CARTESIAN_POINT('',(-0.00153101401290164,0.00455640827717848,0.00626824802518821));
#26522=CARTESIAN_POINT('',(-0.000132772136507351,0.00477312233690794,0.00645114774876679));
#26523=CARTESIAN_POINT('',(0.00249820074447072,0.00520655045636687,0.00594927968387582));
#26524=CARTESIAN_POINT('',(0.0037309317490545,0.00542326451609633,0.00526451189540625));
#26525=CARTESIAN_POINT('',(0.0055471956057837,0.00585669263555524,0.00329599076501096));
#26526=CARTESIAN_POINT('',(0.00613072845792912,0.0060734066952847,0.00201223742308522));
#26527=CARTESIAN_POINT('',(0.00641963610782257,0.0065068348147436,-0.000650546460226448));
#26528=CARTESIAN_POINT('',(0.00612501090557062,0.00672354887447305,-0.00202957700161239));
#26529=CARTESIAN_POINT('',(0.0047732006664181,0.00715697699393194,-0.00434183081328834));
#26530=CARTESIAN_POINT('',(0.00371601562951754,0.00737369105366138,-0.00527505408357836));
#26531=CARTESIAN_POINT('',(0.00125390849600593,0.00780711917312025,-0.00632950136668111));
#26532=CARTESIAN_POINT('',(-0.000151013600605117,0.00802383323284968,-0.00645072537949384));
#26533=CARTESIAN_POINT('',(-0.00275740029882653,0.00845726135230853,-0.00583369489991698));
#26534=CARTESIAN_POINT('',(-0.00395886490043688,0.00867397541203794,-0.00509544040752736));
#26535=CARTESIAN_POINT('',(-0.00568671181406075,0.00910740353149676,-0.00304880313354801));
#26536=CARTESIAN_POINT('',(-0.00621309412607427,0.00932411759122617,-0.00174042035195825));
#26537=CARTESIAN_POINT('',(-0.0063664962444253,0.00971087477110569,0.000644159634078352));
#26538=CARTESIAN_POINT('',(-0.00616278732211593,0.00988091789125582,0.0017096785410187));
#26539=CARTESIAN_POINT('',(-0.0057208257156327,0.0100509610114059,0.00266411091696313));
#26540=CARTESIAN_POINT('',(0.00629974101447218,-6.75276211545794E-5,0.000371045813712693));
#26541=CARTESIAN_POINT('',(0.00635931415992202,0.000102511231671107,-0.000679021451088969));
#26542=CARTESIAN_POINT('',(0.00615648869261233,0.000272550084496797,-0.00174466668461112));
#26543=CARTESIAN_POINT('',(0.00513608632294611,0.000659302997051941,-0.00390528582067021));
#26544=CARTESIAN_POINT('',(0.00416504445783136,0.000876017056781396,-0.0049280153055378));
#26545=CARTESIAN_POINT('',(0.00180515851002141,0.00130944517624031,-0.00619488218876878));
#26546=CARTESIAN_POINT('',(0.00041631442732619,0.00152615923596978,-0.00643901958713219));
#26547=CARTESIAN_POINT('',(-0.00223416086639727,0.0019595873554287,-0.00605328230123756));
#26548=CARTESIAN_POINT('',(-0.00349579207742551,0.00217630141515817,-0.00542340761697953));
#26549=CARTESIAN_POINT('',(-0.0053968348311399,0.0026097295346171,-0.00353669053043316));
#26550=CARTESIAN_POINT('',(-0.00603624637382603,0.00282644359434656,-0.00227984812814483));
#26551=CARTESIAN_POINT('',(-0.00644195839079822,0.0032598717138055,0.000367630044787666));
#26552=CARTESIAN_POINT('',(-0.00620825886508428,0.00347658577353496,0.00175826581543183));
#26553=CARTESIAN_POINT('',(-0.00495944691313349,0.0039100138929939,0.00412769373228605));
#26554=CARTESIAN_POINT('',(-0.00394433448689665,0.00412672795272337,0.0051064858784961));
#26555=CARTESIAN_POINT('',(-0.00153099633192125,0.0045601560721823,0.00626817563605952));
#26556=CARTESIAN_POINT('',(-0.00013277060318269,0.00477687013191176,0.00645107324741287));
#26557=CARTESIAN_POINT('',(0.00249817189389326,0.00521029825137068,0.00594921097836658));
#26558=CARTESIAN_POINT('',(0.00373088866223065,0.00542701231110014,0.00526445109796691));
#26559=CARTESIAN_POINT('',(0.00554713154375952,0.00586044043055906,0.00329595270112154));
#26560=CARTESIAN_POINT('',(0.00613065765695099,0.00607715449028852,0.00201221418467583));
#26561=CARTESIAN_POINT('',(0.00641956197038218,0.00651058260974742,-0.000650538947363007));
#26562=CARTESIAN_POINT('',(0.00612494017062189,0.00672729666947687,-0.00202955356295614));
#26563=CARTESIAN_POINT('',(0.00477314554290736,0.00716072478893575,-0.00434178067147069));
#26564=CARTESIAN_POINT('',(0.00371597271495313,0.0073774388486652,-0.00527499316439211));
#26565=CARTESIAN_POINT('',(0.00125389401519038,0.00781086696812407,-0.0063294282701656));
#26566=CARTESIAN_POINT('',(-0.000151011856618133,0.0080275810278535,-0.00645065088301767));
#26567=CARTESIAN_POINT('',(-0.002757368454872,0.00846100914731235,-0.00583362752924352));
#26568=CARTESIAN_POINT('',(-0.00395881918131735,0.00867772320704176,-0.00509538156261729));
#26569=CARTESIAN_POINT('',(-0.00568664614082771,0.00911115132650058,-0.00304876792431546));
#26570=CARTESIAN_POINT('',(-0.00621302237389273,0.00932786538622998,-0.00174040025263986));
#26571=CARTESIAN_POINT('',(-0.00636642272067288,0.00971462256610951,0.000644152194973444));
#26572=CARTESIAN_POINT('',(-0.00616271615090465,0.00988466568625963,0.00170965879672342));
#26573=CARTESIAN_POINT('',(-0.00572075964843382,0.0100547088064097,0.00266408015036499));
#26574=CARTESIAN_POINT('',(0.00629970453308949,-6.37791813663305E-5,0.000371043665010978));
#26575=CARTESIAN_POINT('',(0.00635927733355519,0.000106259671459356,-0.000679017518920748));
#26576=CARTESIAN_POINT('',(0.00615645304079433,0.000276298524285046,-0.00174465658136197));
#26577=CARTESIAN_POINT('',(0.00513605658021061,0.00066305143684019,-0.00390526320541885));
#26578=CARTESIAN_POINT('',(0.00416502033833495,0.000879765496569645,-0.00492798676772777));
#26579=CARTESIAN_POINT('',(0.00180514805646811,0.00131319361602856,-0.0061948463146166));
#26580=CARTESIAN_POINT('',(0.000416312016476933,0.00152990767575802,-0.00643898229919651));
#26581=CARTESIAN_POINT('',(-0.00223414792851976,0.00196333579521695,-0.00605324724708094));
#26582=CARTESIAN_POINT('',(-0.00349577183352528,0.00218004985494641,-0.00542337621038546));
#26583=CARTESIAN_POINT('',(-0.00539680357842707,0.00261347797440534,-0.0035366700496927));
#26584=CARTESIAN_POINT('',(-0.00603621141832334,0.00283019203413481,-0.00227983492569542));
#26585=CARTESIAN_POINT('',(-0.00644192108584413,0.00326362015359374,0.000367627915866442));
#26586=CARTESIAN_POINT('',(-0.00620822291346865,0.00348033421332321,0.00175825563343103));
#26587=CARTESIAN_POINT('',(-0.00495941819330511,0.00391376233278214,0.00412766982908521));
#26588=CARTESIAN_POINT('',(-0.00394431164551705,0.00413047639251162,0.00510645630717482));
#26589=CARTESIAN_POINT('',(-0.00153098746602296,0.00456390451197054,0.00626813933746984));
#26590=CARTESIAN_POINT('',(-0.000132769834316927,0.0047806185717,0.00645103588967525));
#26591=CARTESIAN_POINT('',(0.00249815742714539,0.00521404669115893,0.00594917652688009));
#26592=CARTESIAN_POINT('',(0.00373086705690167,0.00543076075088839,0.00526442061187951));
#26593=CARTESIAN_POINT('',(0.00554709942068839,0.0058641888703473,0.00329593361447789));
#26594=CARTESIAN_POINT('',(0.00613062215471882,0.00608090293007676,0.00201220253207685));
#26595=CARTESIAN_POINT('',(0.00641952479512427,0.00651433104953567,-0.000650535180135078));
#26596=CARTESIAN_POINT('',(0.0061249047014993,0.00673104510926511,-0.00202954180994597));
#26597=CARTESIAN_POINT('',(0.00477311790193787,0.007164473228724,-0.00434175552850657));
#26598=CARTESIAN_POINT('',(0.00371595119600142,0.00738118728845344,-0.0052749626172563));
#26599=CARTESIAN_POINT('',(0.00125388675397324,0.00781461540791232,-0.00632939161686598));
#26600=CARTESIAN_POINT('',(-0.00015101098211848,0.00803132946764175,-0.00645061352772593));
#26601=CARTESIAN_POINT('',(-0.00275735248713402,0.0084647575871006,-0.00583359374709313));
#26602=CARTESIAN_POINT('',(-0.00395879625605784,0.00868147164683,-0.00509535205560036));
#26603=CARTESIAN_POINT('',(-0.0056866132098368,0.00911489976628883,-0.00304875026910247));
#26604=CARTESIAN_POINT('',(-0.00621298639469194,0.00933161382601823,-0.00174039017409734));
#26605=CARTESIAN_POINT('',(-0.00636638585314085,0.00971837100589775,0.000644148464730775));
#26606=CARTESIAN_POINT('',(-0.00616268046302387,0.00988841412604788,0.00170964889620264));
#26607=CARTESIAN_POINT('',(-0.00572072651989384,0.010058457246198,0.00266406472285341));
#26608=CARTESIAN_POINT('',(0.00629970453308949,6.4870253252478E-5,0.00037104366501098));
#26609=CARTESIAN_POINT('',(0.0063592773335552,0.000234909106078165,-0.000679017518920747));
#26610=CARTESIAN_POINT('',(0.00615645304079433,0.000404947958903854,-0.00174465658136197));
#26611=CARTESIAN_POINT('',(0.00513605658021061,0.000791700871458999,-0.00390526320541886));
#26612=CARTESIAN_POINT('',(0.00416502033833495,0.00100841493118845,-0.00492798676772778));
#26613=CARTESIAN_POINT('',(0.00180514805646811,0.00144184305064737,-0.00619484631461661));
#26614=CARTESIAN_POINT('',(0.000416312016476927,0.00165855711037684,-0.00643898229919652));
#26615=CARTESIAN_POINT('',(-0.00223414792851977,0.00209198522983576,-0.00605324724708094));
#26616=CARTESIAN_POINT('',(-0.00349577183352529,0.00230869928956523,-0.00542337621038546));
#26617=CARTESIAN_POINT('',(-0.00539680357842707,0.00274212740902415,-0.0035366700496927));
#26618=CARTESIAN_POINT('',(-0.00603621141832334,0.00295884146875362,-0.00227983492569542));
#26619=CARTESIAN_POINT('',(-0.00644192108584413,0.00339226958821256,0.000367627915866445));
#26620=CARTESIAN_POINT('',(-0.00620822291346865,0.00360898364794202,0.00175825563343103));
#26621=CARTESIAN_POINT('',(-0.00495941819330511,0.00404241176740095,0.00412766982908522));
#26622=CARTESIAN_POINT('',(-0.00394431164551705,0.00425912582713043,0.00510645630717482));
#26623=CARTESIAN_POINT('',(-0.00153098746602296,0.00469255394658935,0.00626813933746984));
#26624=CARTESIAN_POINT('',(-0.000132769834316927,0.0049092680063188,0.00645103588967525));
#26625=CARTESIAN_POINT('',(0.00249815742714539,0.00534269612577773,0.0059491765268801));
#26626=CARTESIAN_POINT('',(0.00373086705690168,0.0055594101855072,0.00526442061187951));
#26627=CARTESIAN_POINT('',(0.00554709942068839,0.00599283830496611,0.00329593361447789));
#26628=CARTESIAN_POINT('',(0.00613062215471881,0.00620955236469557,0.00201220253207685));
#26629=CARTESIAN_POINT('',(0.00641952479512428,0.00664298048415448,-0.000650535180135079));
#26630=CARTESIAN_POINT('',(0.00612490470149931,0.00685969454388393,-0.00202954180994598));
#26631=CARTESIAN_POINT('',(0.00477311790193787,0.00729312266334281,-0.00434175552850658));
#26632=CARTESIAN_POINT('',(0.0037159511960014,0.00750983672307226,-0.0052749626172563));
#26633=CARTESIAN_POINT('',(0.00125388675397322,0.00794326484253113,-0.00632939161686598));
#26634=CARTESIAN_POINT('',(-0.000151010982118486,0.00815997890226056,-0.00645061352772594));
#26635=CARTESIAN_POINT('',(-0.00275735248713402,0.0085934070217194,-0.00583359374709313));
#26636=CARTESIAN_POINT('',(-0.00395879625605785,0.00881012108144881,-0.00509535205560036));
#26637=CARTESIAN_POINT('',(-0.0056866132098368,0.00924354920090765,-0.00304875026910247));
#26638=CARTESIAN_POINT('',(-0.00621298639469194,0.00946026326063705,-0.00174039017409734));
#26639=CARTESIAN_POINT('',(-0.00636638585314084,0.00984702044051656,0.000644148464730776));
#26640=CARTESIAN_POINT('',(-0.00616268046302386,0.0100170635606667,0.00170964889620264));
#26641=CARTESIAN_POINT('',(-0.00572072651989384,0.0101871066808168,0.00266406472285341));
#26642=CARTESIAN_POINT('',(0.00634020891479936,0.000189771248083037,0.00037342931566486));
#26643=CARTESIAN_POINT('',(0.0064001647426653,0.000359810100908722,-0.000683383308558913));
#26644=CARTESIAN_POINT('',(0.00619603637722438,0.000529848953734411,-0.00175587397032886));
#26645=CARTESIAN_POINT('',(0.00516907920771887,0.000916601866289553,-0.00393037236263709));
#26646=CARTESIAN_POINT('',(0.00419179962182787,0.00113331592601901,-0.0049596715961277));
#26647=CARTESIAN_POINT('',(0.00181675437951675,0.00156674404547792,-0.00623467650322993));
#26648=CARTESIAN_POINT('',(0.000418988723096619,0.00178345810520739,-0.00648038217684154));
#26649=CARTESIAN_POINT('',(-0.00224851253562439,0.00221688622466631,-0.00609216701479261));
#26650=CARTESIAN_POINT('',(-0.00351824813792527,0.00243360028439577,-0.00545824617913206));
#26651=CARTESIAN_POINT('',(-0.00543150269661675,0.0028670284038547,-0.00355940931197431));
#26652=CARTESIAN_POINT('',(-0.00607502165300737,0.00308374246358417,-0.00229449328047711));
#26653=CARTESIAN_POINT('',(-0.00648333985861916,0.0035171705830431,0.000369991604727282));
#26654=CARTESIAN_POINT('',(-0.00624813910784035,0.00373388464277257,0.00176956045843447));
#26655=CARTESIAN_POINT('',(-0.00499130511220827,0.0041673127622315,0.00415420896492109));
#26656=CARTESIAN_POINT('',(-0.003969671867355,0.00438402682196097,0.00513928861770052));
#26657=CARTESIAN_POINT('',(-0.00154083105478036,0.0048174549414199,0.00630844076859283));
#26658=CARTESIAN_POINT('',(-0.00013362348705897,0.00503416900114937,0.00649251326670571));
#26659=CARTESIAN_POINT('',(0.00251421950140125,0.00546759712060829,0.00598742716476928));
#26660=CARTESIAN_POINT('',(0.00375485492214007,0.00568431118033775,0.00529826856471998));
#26661=CARTESIAN_POINT('',(0.0055827648762884,0.00611773929979667,0.00331712504536326));
#26662=CARTESIAN_POINT('',(0.0061700394096979,0.00633445335952612,0.00202514012605585));
#26663=CARTESIAN_POINT('',(0.00646079956941439,0.00676788147898503,-0.000654717840625502));
#26664=CARTESIAN_POINT('',(0.00616428519572137,0.00698459553871448,-0.00204259088799945));
#26665=CARTESIAN_POINT('',(0.00480380699035953,0.00741802365817337,-0.00436967114300784));
#26666=CARTESIAN_POINT('',(0.00373984315869069,0.00763473771790281,-0.00530887835064227));
#26667=CARTESIAN_POINT('',(0.00126194870472618,0.00806816583736168,-0.00637008687371401));
#26668=CARTESIAN_POINT('',(-0.000151981917569498,0.00828487989709111,-0.00649208818915132));
#26669=CARTESIAN_POINT('',(-0.00277508107377819,0.00871830801654996,-0.00587110123758437));
#26670=CARTESIAN_POINT('',(-0.00398424960769119,0.00893502207627938,-0.00512811297058012));
#26671=CARTESIAN_POINT('',(-0.00572317567889829,0.0093684501957382,-0.00306835241774121));
#26672=CARTESIAN_POINT('',(-0.00625293321619238,0.00958516425546761,-0.00175158013190655));
#26673=CARTESIAN_POINT('',(-0.00640731896696443,0.00997192143534712,0.000648290061397133));
#26674=CARTESIAN_POINT('',(-0.00620230383909161,0.0101419645554972,0.0017206412008604));
#26675=CARTESIAN_POINT('',(-0.00575750832281848,0.0103120076756474,0.00268119350942863));
#26676=CARTESIAN_POINT('',(0.00648675514451895,0.000391865302947556,0.00038206068081589));
#26677=CARTESIAN_POINT('',(0.00654809677853758,0.00056190415577324,-0.000699178883857519));
#26678=CARTESIAN_POINT('',(0.00633925023381643,0.000731943008598929,-0.00179645886487608));
#26679=CARTESIAN_POINT('',(0.00528855619644159,0.00111869592115407,-0.00402121814688153));
#26680=CARTESIAN_POINT('',(0.00428868797969965,0.00133540998088352,-0.00507430838220636));
#26681=CARTESIAN_POINT('',(0.00185874645079114,0.00176883810034244,-0.00637878347941126));
#26682=CARTESIAN_POINT('',(0.000428673138624558,0.0019855521600719,-0.00663016834129133));
#26683=CARTESIAN_POINT('',(-0.00230048417236396,0.00241898027953082,-0.00623298005720765));
#26684=CARTESIAN_POINT('',(-0.00359956817118591,0.00263569433926028,-0.00558440691124391));
#26685=CARTESIAN_POINT('',(-0.00555704528560669,0.00306912245871922,-0.0036416807357883));
#26686=CARTESIAN_POINT('',(-0.00621543840120553,0.00328583651844868,-0.00234752770629642));
#26687=CARTESIAN_POINT('',(-0.00663319438629153,0.00371926463790762,0.000378543511364632));
#26688=CARTESIAN_POINT('',(-0.0063925572557787,0.00393597869763708,0.00181046169953381));
#26689=CARTESIAN_POINT('',(-0.00510667306859641,0.00436940681709602,0.00425022846040734));
#26690=CARTESIAN_POINT('',(-0.00406142601192695,0.00458612087682549,0.00525807703311169));
#26691=CARTESIAN_POINT('',(-0.00157644549347588,0.00501954899628442,0.00645425271619107));
#26692=CARTESIAN_POINT('',(-0.000136712031694268,0.00523626305601388,0.0066425798265661));
#26693=CARTESIAN_POINT('',(0.00257233263198876,0.00566969117547281,0.00612581927274375));
#26694=CARTESIAN_POINT('',(0.00384164383389017,0.00588640523520227,0.00542073160854637));
#26695=CARTESIAN_POINT('',(0.00571180370687351,0.00631983335466118,0.00339379636257676));
#26696=CARTESIAN_POINT('',(0.00631265237795545,0.00653654741439063,0.00207194878080453));
#26697=CARTESIAN_POINT('',(0.00661013310567399,0.00696997553384954,-0.00066985084844325));
#26698=CARTESIAN_POINT('',(0.00630676516231059,0.00718668959357899,-0.00208980289591881));
#26699=CARTESIAN_POINT('',(0.00491484115535283,0.00762011771303788,-0.00447067078509022));
#26700=CARTESIAN_POINT('',(0.00382628509175847,0.00783683177276732,-0.00543158662678607));
#26701=CARTESIAN_POINT('',(0.00129111711656598,0.00827025989222619,-0.00651732369617108));
#26702=CARTESIAN_POINT('',(-0.000155494795032157,0.00848697395195563,-0.00664214492386024));
#26703=CARTESIAN_POINT('',(-0.00283922370282928,0.00892040207141447,-0.00600680461301443));
#26704=CARTESIAN_POINT('',(-0.00407634069902827,0.00913711613114389,-0.00524664307447946));
#26705=CARTESIAN_POINT('',(-0.00585545993467536,0.00957054425060272,-0.00313927365776871));
#26706=CARTESIAN_POINT('',(-0.00639746217412347,0.00978725831033213,-0.00179206577959293));
#26707=CARTESIAN_POINT('',(-0.00655541636404353,0.0101740154902116,0.000663274498903706));
#26708=CARTESIAN_POINT('',(-0.00634566256045371,0.0103440586103618,0.0017604117327269));
#26709=CARTESIAN_POINT('',(-0.00589058613596731,0.0105141017305119,0.00274316604144382));
#26710=CARTESIAN_POINT('',(0.00659279699252868,0.000469058362981516,0.000388306395313039));
#26711=CARTESIAN_POINT('',(0.00665514140529975,0.000639097215807201,-0.000710608669517962));
#26712=CARTESIAN_POINT('',(0.00644288075397842,0.00080913606863289,-0.00182582637045641));
#26713=CARTESIAN_POINT('',(0.00537501055765604,0.00119588898118803,-0.00408695477390774));
#26714=CARTESIAN_POINT('',(0.0043587970540785,0.00141260304091748,-0.00515726033988509));
#26715=CARTESIAN_POINT('',(0.00188913219901688,0.0018460311603764,-0.00648306026697927));
#26716=CARTESIAN_POINT('',(0.000435680847532806,0.00206274522010586,-0.0067385546280961));
#26717=CARTESIAN_POINT('',(-0.00233809120199892,0.00249617333956478,-0.00633487333191104));
#26718=CARTESIAN_POINT('',(-0.00365841190004657,0.00271288739929425,-0.00567569767460917));
#26719=CARTESIAN_POINT('',(-0.00564788875640694,0.00314631551875317,-0.00370121289732066));
#26720=CARTESIAN_POINT('',(-0.00631704491471967,0.00336302957848265,-0.00238590377733404));
#26721=CARTESIAN_POINT('',(-0.00674163014118887,0.00379645769794157,0.000384731729141146));
#26722=CARTESIAN_POINT('',(-0.00649705920934535,0.00401317175767105,0.00184005811562972));
#26723=CARTESIAN_POINT('',(-0.00519015410608139,0.00444659987712998,0.00431970882005773));
#26724=CARTESIAN_POINT('',(-0.00412781993466094,0.00466331393685945,0.00534403313799717));
#26725=CARTESIAN_POINT('',(-0.00160221634341401,0.00509674205631838,0.00655976323266633));
#26726=CARTESIAN_POINT('',(-0.000138946923587524,0.00531345611604784,0.00675116900939604));
#26727=CARTESIAN_POINT('',(0.00261438368832041,0.00574688423550677,0.00622596074282903));
#26728=CARTESIAN_POINT('',(0.00390444488040186,0.00596359829523623,0.0055093466995323));
#26729=CARTESIAN_POINT('',(0.00580517708185861,0.00639702641469514,0.00344927624890489));
#26730=CARTESIAN_POINT('',(0.00641584809123392,0.0066137404744246,0.00210581984157422));
#26731=CARTESIAN_POINT('',(0.00671819186764348,0.0070471685938835,-0.000680801195770578));
#26732=CARTESIAN_POINT('',(0.00640986463467774,0.00726388265361295,-0.00212396582578469));
#26733=CARTESIAN_POINT('',(0.00499518623192447,0.00769731077307184,-0.00454375481267135));
#26734=CARTESIAN_POINT('',(0.00388883506213696,0.00791402483280128,-0.0055203791695439));
#26735=CARTESIAN_POINT('',(0.00131222357765282,0.00834745295226015,-0.00662386526178012));
#26736=CARTESIAN_POINT('',(-0.000158036737043802,0.00856416701198959,-0.00675072699714379));
#26737=CARTESIAN_POINT('',(-0.00288563774523621,0.00899759513144844,-0.00610500049795324));
#26738=CARTESIAN_POINT('',(-0.00414297843873199,0.00921430919117785,-0.00533241226339903));
#26739=CARTESIAN_POINT('',(-0.00595118172139095,0.00964773731063668,-0.00319059274915747));
#26740=CARTESIAN_POINT('',(-0.00650204431055414,0.00986445137036608,-0.00182136146947011));
#26741=CARTESIAN_POINT('',(-0.00666258064729905,0.0102512085502456,0.000674117339743923));
#26742=CARTESIAN_POINT('',(-0.00644939790574807,0.0104212516703957,0.00178918995993563));
#26743=CARTESIAN_POINT('',(-0.00598688214619151,0.0105912947905458,0.00278800978688379));
#26744=CARTESIAN_POINT('',(0.00682991377313814,0.000546251423015476,0.000402272237496718));
#26745=CARTESIAN_POINT('',(0.00689450046736609,0.000716290275841162,-0.000736166447222965));
#26746=CARTESIAN_POINT('',(0.00667460564160431,0.000886329128666851,-0.00189149410926364));
#26747=CARTESIAN_POINT('',(0.00556832838628288,0.00127308204122199,-0.00423394634054989));
#26748=CARTESIAN_POINT('',(0.0045155657102292,0.00148979610095144,-0.00534274655612142));
#26749=CARTESIAN_POINT('',(0.00195707679759685,0.00192322422041036,-0.00671623025245665));
#26750=CARTESIAN_POINT('',(0.000451350561018182,0.00213993828013982,-0.00698091373322034));
#26751=CARTESIAN_POINT('',(-0.00242218307669453,0.00257336639959874,-0.00656271362059788));
#26752=CARTESIAN_POINT('',(-0.00378999047782856,0.00279008045932821,-0.00587983002721171));
#26753=CARTESIAN_POINT('',(-0.00585102093242832,0.00322350857878714,-0.00383433085735453));
#26754=CARTESIAN_POINT('',(-0.00654424398589403,0.0034402226385166,-0.00247171528088352));
#26755=CARTESIAN_POINT('',(-0.00698409986033083,0.00387365075797554,0.000398569004749002));
#26756=CARTESIAN_POINT('',(-0.00673073268130192,0.00409036481770501,0.00190623771391051));
#26757=CARTESIAN_POINT('',(-0.00537682338073001,0.00452379293716394,0.00447507162733712));
#26758=CARTESIAN_POINT('',(-0.00427628125918701,0.00474050699689341,0.00553623683160219));
#26759=CARTESIAN_POINT('',(-0.00165984171571361,0.00517393511635234,0.00679569191984611));
#26760=CARTESIAN_POINT('',(-0.000143944293783209,0.0053906491760818,0.00699398180382494));
#26761=CARTESIAN_POINT('',(0.00270841270880366,0.00582407729554073,0.00644988387730647));
#26762=CARTESIAN_POINT('',(0.00404487228946013,0.00604079135527019,0.00570749606680917));
#26763=CARTESIAN_POINT('',(0.00601396629561387,0.0064742194747291,0.00357333304611855));
#26764=CARTESIAN_POINT('',(0.00664660072111115,0.00669093353445856,0.00218155783592524));
#26765=CARTESIAN_POINT('',(0.00695981860497174,0.00712436165391747,-0.000705286916771713));
#26766=CARTESIAN_POINT('',(0.00664040206333504,0.00734107571364691,-0.00220035645927534));
#26767=CARTESIAN_POINT('',(0.00517484328479609,0.0077745038331058,-0.00470717566641223));
#26768=CARTESIAN_POINT('',(0.00402870104789384,0.00799121789283525,-0.00571892533104548));
#26769=CARTESIAN_POINT('',(0.00135941905940744,0.00842464601229412,-0.0068620994449112));
#26770=CARTESIAN_POINT('',(-0.000163720692176703,0.00864136007202355,-0.00699352389414366));
#26771=CARTESIAN_POINT('',(-0.00298942269916865,0.0090747881914824,-0.00632457317178717));
#26772=CARTESIAN_POINT('',(-0.00429198495457645,0.00929150225121182,-0.00552419800019821));
#26773=CARTESIAN_POINT('',(-0.00616522214341475,0.00972493037067064,-0.00330534572604625));
#26774=CARTESIAN_POINT('',(-0.00673589707684525,0.00994164443040004,-0.00188686862348324));
#26775=CARTESIAN_POINT('',(-0.00690220726941841,0.0103284016102796,0.000698362668931858));
#26776=CARTESIAN_POINT('',(-0.00668135718949568,0.0104984447304297,0.00185354003224629));
#26777=CARTESIAN_POINT('',(-0.00620220657101483,0.0106684878505798,0.00288828345005326));
#26778=CARTESIAN_POINT('',(0.00696098870573786,0.000546251423015476,0.000409992365183249));
#26779=CARTESIAN_POINT('',(0.00702681490267023,0.000716290275841162,-0.000750294439267526));
#26780=CARTESIAN_POINT('',(0.0068027000090682,0.00088632912866685,-0.00192779434249054));
#26781=CARTESIAN_POINT('',(0.00567519185369527,0.00127308204122199,-0.00431520128016583));
#26782=CARTESIAN_POINT('',(0.00460222529200104,0.00148979610095144,-0.00544528081467901));
#26783=CARTESIAN_POINT('',(0.00199463564795106,0.00192322422041036,-0.00684512345036601));
#26784=CARTESIAN_POINT('',(0.000460012565595309,0.00213993828013982,-0.00711488655153982));
#26785=CARTESIAN_POINT('',(-0.00246866792175518,0.00257336639959874,-0.00668866063458132));
#26786=CARTESIAN_POINT('',(-0.0038627253267499,0.00279008045932821,-0.00599267161644901));
#26787=CARTESIAN_POINT('',(-0.00596330963764944,0.00322350857878714,-0.00390791665585604));
#26788=CARTESIAN_POINT('',(-0.00666983654355425,0.0034402226385166,-0.00251915071339539));
#26789=CARTESIAN_POINT('',(-0.00711813382457544,0.00387365075797554,0.000406218062580345));
#26790=CARTESIAN_POINT('',(-0.00685990419969183,0.00409036481770501,0.00194282089609541));
#26791=CARTESIAN_POINT('',(-0.00548001161789365,0.00452379293716394,0.00456095407496612));
#26792=CARTESIAN_POINT('',(-0.00435834866097909,0.00474050699689341,0.00564248442032174));
#26793=CARTESIAN_POINT('',(-0.00169169623807508,0.00517393511635234,0.00692611009055063));
#26794=CARTESIAN_POINT('',(-0.000146706772085636,0.0053906491760818,0.00712820541542389));
#26795=CARTESIAN_POINT('',(0.00276039067295526,0.00582407729554073,0.00657366554169863));
#26796=CARTESIAN_POINT('',(0.0041224986520067,0.00604079135527019,0.00581703034310011));
#26797=CARTESIAN_POINT('',(0.00612938213438403,0.0064742194747291,0.00364190995700408));
#26798=CARTESIAN_POINT('',(0.00677415763770992,0.00669093353445856,0.00222342476950659));
#26799=CARTESIAN_POINT('',(0.0070933865803305,0.00712436165391747,-0.000718822290445522));
#26800=CARTESIAN_POINT('',(0.0067678400196252,0.00734107571364692,-0.00224258416290012));
#26801=CARTESIAN_POINT('',(0.00527415526109607,0.0077745038331058,-0.00479751249257198));
#26802=CARTESIAN_POINT('',(0.00410601706327225,0.00799121789283524,-0.00582867894978923));
#26803=CARTESIAN_POINT('',(0.00138550808007523,0.00842464601229412,-0.00699379206243323));
#26804=CARTESIAN_POINT('',(-0.000166862705297958,0.00864136007202355,-0.00712773871785999));
#26805=CARTESIAN_POINT('',(-0.00304679361069417,0.0090747881914824,-0.00644594996068229));
#26806=CARTESIAN_POINT('',(-0.00437435373071718,0.00929150225121181,-0.00563021454807782));
#26807=CARTESIAN_POINT('',(-0.00628354077872295,0.00972493037067064,-0.00336877961154627));
#26808=CARTESIAN_POINT('',(-0.00686516770670571,0.00994164443040004,-0.00192308008761919));
#26809=CARTESIAN_POINT('',(-0.00703466960828227,0.0103284016102796,0.000711765157279578));
#26810=CARTESIAN_POINT('',(-0.00680958112794892,0.0104984447304297,0.00188911187734821));
#26811=CARTESIAN_POINT('',(-0.00632123498561395,0.0106684878505798,0.00294371336778276));
#26812=CARTESIAN_POINT('',(0.00719810548634731,0.000469058362981516,0.000423958207366928));
#26813=CARTESIAN_POINT('',(0.00726617396473655,0.000639097215807201,-0.000775852216972529));
#26814=CARTESIAN_POINT('',(0.00703442489669408,0.00080913606863289,-0.00199346208129777));
#26815=CARTESIAN_POINT('',(0.00586850968232211,0.00119588898118803,-0.00446219284680798));
#26816=CARTESIAN_POINT('',(0.00475899394815174,0.00141260304091748,-0.00563076703091534));
#26817=CARTESIAN_POINT('',(0.00206258024653102,0.0018460311603764,-0.00707829343584338));
#26818=CARTESIAN_POINT('',(0.000475682279080687,0.00206274522010586,-0.00735724565666407));
#26819=CARTESIAN_POINT('',(-0.00255275979645077,0.00249617333956479,-0.00691650092326816));
#26820=CARTESIAN_POINT('',(-0.0039943039045319,0.00271288739929425,-0.00619680396905156));
#26821=CARTESIAN_POINT('',(-0.00616644181367082,0.00314631551875318,-0.00404103461588991));
#26822=CARTESIAN_POINT('',(-0.00689703561472861,0.00336302957848265,-0.00260496221694487));
#26823=CARTESIAN_POINT('',(-0.0073606035437174,0.00379645769794158,0.000420055338188199));
#26824=CARTESIAN_POINT('',(-0.00709357767164839,0.00401317175767105,0.00200900049437622));
#26825=CARTESIAN_POINT('',(-0.00566668089254228,0.00444659987712998,0.0047163168822455));
#26826=CARTESIAN_POINT('',(-0.00450680998550517,0.00466331393685945,0.00583468811392677));
#26827=CARTESIAN_POINT('',(-0.00174932161037469,0.00509674205631838,0.00716203877773041));
#26828=CARTESIAN_POINT('',(-0.000151704142281321,0.00531345611604784,0.00737101820985279));
#26829=CARTESIAN_POINT('',(0.00285441969343851,0.00574688423550677,0.00679758867617607));
#26830=CARTESIAN_POINT('',(0.00426292606106497,0.00596359829523623,0.00601517971037698));
#26831=CARTESIAN_POINT('',(0.00633817134813929,0.00639702641469514,0.00376596675421775));
#26832=CARTESIAN_POINT('',(0.00700491026758715,0.0066137404744246,0.00229916276385761));
#26833=CARTESIAN_POINT('',(0.00733501331765875,0.0070471685938835,-0.000743308011446658));
#26834=CARTESIAN_POINT('',(0.0069983774482825,0.00726388265361295,-0.00231897479639079));
#26835=CARTESIAN_POINT('',(0.00545381231396769,0.00769731077307185,-0.00496093334631286));
#26836=CARTESIAN_POINT('',(0.00424588304902913,0.00791402483280129,-0.00602722511129081));
#26837=CARTESIAN_POINT('',(0.00143270356182986,0.00834745295226016,-0.00723202624556431));
#26838=CARTESIAN_POINT('',(-0.000172546660430858,0.00856416701198959,-0.00737053561485987));
#26839=CARTESIAN_POINT('',(-0.00315057856462661,0.00899759513144844,-0.00666552263451621));
#26840=CARTESIAN_POINT('',(-0.00452336024656164,0.00921430919117786,-0.00582200028487701));
#26841=CARTESIAN_POINT('',(-0.00649758120074675,0.00964773731063668,-0.00348353258843506));
#26842=CARTESIAN_POINT('',(-0.00709902047299683,0.00986445137036609,-0.00198858724163231));
#26843=CARTESIAN_POINT('',(-0.00727429623040165,0.0102512085502456,0.000736010486467512));
#26844=CARTESIAN_POINT('',(-0.00704154041169653,0.0104212516703957,0.00195346194965887));
#26845=CARTESIAN_POINT('',(-0.00653655941043727,0.0105912947905458,0.00304398703095224));
#26846=CARTESIAN_POINT('',(0.00730414733435704,0.000391865302947556,0.000430203921864076));
#26847=CARTESIAN_POINT('',(0.00737321859149873,0.000561904155773241,-0.000787282002632974));
#26848=CARTESIAN_POINT('',(0.00713805541685607,0.000731943008598929,-0.00202282958687811));
#26849=CARTESIAN_POINT('',(0.00595496404353656,0.00111869592115407,-0.00452792947383419));
#26850=CARTESIAN_POINT('',(0.00482910302253058,0.00133540998088352,-0.00571371898859407));
#26851=CARTESIAN_POINT('',(0.00209296599475677,0.00176883810034244,-0.0071825702234114));
#26852=CARTESIAN_POINT('',(0.000482689987988938,0.0019855521600719,-0.00746563194346884));
#26853=CARTESIAN_POINT('',(-0.00259036682608572,0.00241898027953082,-0.00701839419797155));
#26854=CARTESIAN_POINT('',(-0.00405314763339256,0.00263569433926028,-0.00628809473241681));
#26855=CARTESIAN_POINT('',(-0.00625728528447107,0.00306912245871922,-0.00410056677742228));
#26856=CARTESIAN_POINT('',(-0.00699864212824275,0.00328583651844868,-0.00264333828798249));
#26857=CARTESIAN_POINT('',(-0.00746903929861474,0.00371926463790762,0.000426243555964711));
#26858=CARTESIAN_POINT('',(-0.00719807962521505,0.00393597869763709,0.00203859691047211));
#26859=CARTESIAN_POINT('',(-0.00575016193002726,0.00436940681709602,0.00478579724189588));
#26860=CARTESIAN_POINT('',(-0.00457320390823917,0.00458612087682549,0.00592064421881225));
#26861=CARTESIAN_POINT('',(-0.00177509246031282,0.00501954899628442,0.00726754929420567));
#26862=CARTESIAN_POINT('',(-0.000153939034174578,0.00523626305601388,0.00747960739268273));
#26863=CARTESIAN_POINT('',(0.00289647074977017,0.00566969117547281,0.00689773014626135));
#26864=CARTESIAN_POINT('',(0.00432572710757667,0.00588640523520227,0.00610379480136291));
#26865=CARTESIAN_POINT('',(0.00643154472312439,0.00631983335466118,0.00382144664054589));
#26866=CARTESIAN_POINT('',(0.00710810598086562,0.00653654741439064,0.00233303382462729));
#26867=CARTESIAN_POINT('',(0.00744307207962825,0.00696997553384954,-0.000754258358773985));
#26868=CARTESIAN_POINT('',(0.00710147692064965,0.00718668959357899,-0.00235313772625666));
#26869=CARTESIAN_POINT('',(0.00553415739053934,0.00762011771303789,-0.00503401737389399));
#26870=CARTESIAN_POINT('',(0.00430843301940762,0.00783683177276733,-0.00611601765404865));
#26871=CARTESIAN_POINT('',(0.0014538100229167,0.0082702598922262,-0.00733856781117336));
#26872=CARTESIAN_POINT('',(-0.000175088602442502,0.00848697395195563,-0.00747911768814341));
#26873=CARTESIAN_POINT('',(-0.00319699260703353,0.00892040207141448,-0.00676371851945502));
#26874=CARTESIAN_POINT('',(-0.00458999798626536,0.0091371161311439,-0.00590776947379658));
#26875=CARTESIAN_POINT('',(-0.00659330298746234,0.00957054425060272,-0.00353485167982381));
#26876=CARTESIAN_POINT('',(-0.0072036026094275,0.00978725831033213,-0.00201788293150949));
#26877=CARTESIAN_POINT('',(-0.00738146051365716,0.0101740154902116,0.000746853327307728));
#26878=CARTESIAN_POINT('',(-0.00714527575699089,0.0103440586103618,0.0019822401768676));
#26879=CARTESIAN_POINT('',(-0.00663285542066147,0.0105141017305119,0.00308883077639221));
#26880=CARTESIAN_POINT('',(0.00745069356407664,0.000189771248083037,0.000438835287015107));
#26881=CARTESIAN_POINT('',(0.00752115062737102,0.000359810100908722,-0.00080307757793158));
#26882=CARTESIAN_POINT('',(0.00728126927344812,0.000529848953734411,-0.00206341448142532));
#26883=CARTESIAN_POINT('',(0.00607444103225929,0.000916601866289553,-0.00461877525807863));
#26884=CARTESIAN_POINT('',(0.00492599138040236,0.00113331592601901,-0.00582835577467273));
#26885=CARTESIAN_POINT('',(0.00213495806603116,0.00156674404547792,-0.00732667719959273));
#26886=CARTESIAN_POINT('',(0.000492374403516869,0.00178345810520739,-0.00761541810791863));
#26887=CARTESIAN_POINT('',(-0.00264233846282531,0.00221688622466631,-0.0071592072403866));
#26888=CARTESIAN_POINT('',(-0.00413446766665321,0.00243360028439577,-0.00641425546452866));
#26889=CARTESIAN_POINT('',(-0.00638282787346101,0.00286702840385471,-0.00418283820123627));
#26890=CARTESIAN_POINT('',(-0.00713905887644092,0.00308374246358417,-0.0026963727138018));
#26891=CARTESIAN_POINT('',(-0.00761889382628711,0.0035171705830431,0.000434795462602067));
#26892=CARTESIAN_POINT('',(-0.0073424977731534,0.00373388464277257,0.00207949815157147));
#26893=CARTESIAN_POINT('',(-0.00586552988641539,0.0041673127622315,0.00488181673738215));
#26894=CARTESIAN_POINT('',(-0.0046649580528111,0.00438402682196097,0.00603943263422343));
#26895=CARTESIAN_POINT('',(-0.00181070689900835,0.0048174549414199,0.00741336124180392));
#26896=CARTESIAN_POINT('',(-0.000157027578809877,0.00503416900114937,0.00762967395254313));
#26897=CARTESIAN_POINT('',(0.00295458388035767,0.00546759712060829,0.00703612225423582));
#26898=CARTESIAN_POINT('',(0.00441251601932677,0.00568431118033775,0.0062262578451893));
#26899=CARTESIAN_POINT('',(0.00656058355370951,0.00611773929979667,0.00389811795775938));
#26900=CARTESIAN_POINT('',(0.00725071894912317,0.00633445335952612,0.00237984247937596));
#26901=CARTESIAN_POINT('',(0.00759240561588785,0.00676788147898503,-0.000769391366591733));
#26902=CARTESIAN_POINT('',(0.00724395688723887,0.00698459553871448,-0.00240034973417602));
#26903=CARTESIAN_POINT('',(0.00564519155553264,0.00741802365817337,-0.00513501701597638));
#26904=CARTESIAN_POINT('',(0.00439487495247539,0.00763473771790281,-0.00623872593019245));
#26905=CARTESIAN_POINT('',(0.00148297843475648,0.00806816583736168,-0.00748580463363043));
#26906=CARTESIAN_POINT('',(-0.000178601479905164,0.00828487989709111,-0.00762917442285234));
#26907=CARTESIAN_POINT('',(-0.00326113523608462,0.00871830801654996,-0.00689942189488508));
#26908=CARTESIAN_POINT('',(-0.00468208907760243,0.00893502207627938,-0.00602629957769591));
#26909=CARTESIAN_POINT('',(-0.00672558724323942,0.0093684501957382,-0.00360577291985132));
#26910=CARTESIAN_POINT('',(-0.00734813156735859,0.0095851642554676,-0.00205836857919588));
#26911=CARTESIAN_POINT('',(-0.00752955791073626,0.00997192143534712,0.000761837764814304));
#26912=CARTESIAN_POINT('',(-0.007288634478353,0.0101419645554972,0.0020220107087341));
#26913=CARTESIAN_POINT('',(-0.0067659332338103,0.0103120076756474,0.0031508033084074));
#26914=CARTESIAN_POINT('',(0.0074911979457865,6.48702532524772E-5,0.000441220937668989));
#26915=CARTESIAN_POINT('',(0.00756203803648113,0.000234909106078164,-0.000807443367569745));
#26916=CARTESIAN_POINT('',(0.00732085260987818,0.000404947958903854,-0.00207463187039221));
#26917=CARTESIAN_POINT('',(0.00610746365976755,0.000791700871458998,-0.00464388441529687));
#26918=CARTESIAN_POINT('',(0.00495277066389529,0.00100841493118845,-0.00586004060307266));
#26919=CARTESIAN_POINT('',(0.00214656438907979,0.00144184305064737,-0.00736650738820606));
#26920=CARTESIAN_POINT('',(0.000495051110136548,0.00165855711037683,-0.00765681798556365));
#26921=CARTESIAN_POINT('',(-0.00265670306992994,0.00209198522983576,-0.00719812700809825));
#26922=CARTESIAN_POINT('',(-0.0041569439710532,0.00230869928956522,-0.00644912543327526));
#26923=CARTESIAN_POINT('',(-0.0064175269916507,0.00274212740902416,-0.00420557746351788));
#26924=CARTESIAN_POINT('',(-0.00717786911112494,0.00295884146875362,-0.00271103106858349));
#26925=CARTESIAN_POINT('',(-0.00766031259906214,0.00339226958821256,0.000437159151462911));
#26926=CARTESIAN_POINT('',(-0.00738241396752509,0.00360898364794202,0.00209080297657492));
#26927=CARTESIAN_POINT('',(-0.00589741680531854,0.00404241176740095,0.00490835587321803));
#26928=CARTESIAN_POINT('',(-0.00469031827464905,0.00425912582713042,0.00607226494474913));
#26929=CARTESIAN_POINT('',(-0.00182055048776573,0.00469255394658935,0.00745366267292691));
#26930=CARTESIAN_POINT('',(-0.000157881231551919,0.00490926800631881,0.00767115132957359));
#26931=CARTESIAN_POINT('',(0.00297064595461353,0.00534269612577774,0.00707437289212501));
#26932=CARTESIAN_POINT('',(0.00443650388456516,0.0055594101855072,0.00626010579802976));
#26933=CARTESIAN_POINT('',(0.00659624900930952,0.00599283830496612,0.00391930938864474));
#26934=CARTESIAN_POINT('',(0.00729013620410225,0.00620955236469557,0.00239278007335497));
#26935=CARTESIAN_POINT('',(0.00763368039017796,0.00664298048415448,-0.000773574027082155));
#26936=CARTESIAN_POINT('',(0.00728333738146094,0.00685969454388392,-0.00241339881222951));
#26937=CARTESIAN_POINT('',(0.00567588064395429,0.00729312266334281,-0.00516293263047764));
#26938=CARTESIAN_POINT('',(0.00441876691516466,0.00750983672307225,-0.00627264166357842));
#26939=CARTESIAN_POINT('',(0.00149104038550943,0.00794326484253112,-0.00752649989047846));
#26940=CARTESIAN_POINT('',(-0.00017957241535618,0.00815997890226055,-0.00767064908427772));
#26941=CARTESIAN_POINT('',(-0.00327886382272879,0.0085934070217194,-0.00693692938537633));
#26942=CARTESIAN_POINT('',(-0.00470754242923579,0.00881012108144882,-0.00605906049267568));
#26943=CARTESIAN_POINT('',(-0.00676214971230091,0.00924354920090764,-0.00362537506849006));
#26944=CARTESIAN_POINT('',(-0.00738807838885903,0.00946026326063704,-0.00206955853700509));
#26945=CARTESIAN_POINT('',(-0.00757049102455984,0.00984702044051656,0.000765979361480664));
#26946=CARTESIAN_POINT('',(-0.00732825785442074,0.0100170635606667,0.00203300301339187));
#26947=CARTESIAN_POINT('',(-0.00680271503673494,0.0101871066808168,0.00316793209498263));
#26948=CARTESIAN_POINT('',(0.0074911979457865,-6.37794509163898E-5,0.00044122093766899));
#26949=CARTESIAN_POINT('',(0.00756203803648112,0.000106259401909297,-0.000807443367569744));
#26950=CARTESIAN_POINT('',(0.00732085260987817,0.000276298254734986,-0.00207463187039221));
#26951=CARTESIAN_POINT('',(0.00610746365976754,0.00066305116729013,-0.00464388441529687));
#26952=CARTESIAN_POINT('',(0.00495277066389528,0.000879765227019586,-0.00586004060307266));
#26953=CARTESIAN_POINT('',(0.00214656438907979,0.0013131933464785,-0.00736650738820606));
#26954=CARTESIAN_POINT('',(0.000495051110136555,0.00152990740620797,-0.00765681798556366));
#26955=CARTESIAN_POINT('',(-0.00265670306992994,0.00196333552566689,-0.00719812700809826));
#26956=CARTESIAN_POINT('',(-0.0041569439710532,0.00218004958539635,-0.00644912543327526));
#26957=CARTESIAN_POINT('',(-0.0064175269916507,0.00261347770485529,-0.00420557746351788));
#26958=CARTESIAN_POINT('',(-0.00717786911112494,0.00283019176458475,-0.00271103106858349));
#26959=CARTESIAN_POINT('',(-0.00766031259906214,0.00326361988404369,0.000437159151462912));
#26960=CARTESIAN_POINT('',(-0.00738241396752509,0.00348033394377315,0.00209080297657492));
#26961=CARTESIAN_POINT('',(-0.00589741680531855,0.00391376206323209,0.00490835587321803));
#26962=CARTESIAN_POINT('',(-0.00469031827464905,0.00413047612296156,0.00607226494474913));
#26963=CARTESIAN_POINT('',(-0.00182055048776573,0.00456390424242049,0.00745366267292691));
#26964=CARTESIAN_POINT('',(-0.000157881231551919,0.00478061830214995,0.00767115132957359));
#26965=CARTESIAN_POINT('',(0.00297064595461353,0.00521404642160888,0.00707437289212501));
#26966=CARTESIAN_POINT('',(0.00443650388456517,0.00543076048133834,0.00626010579802976));
#26967=CARTESIAN_POINT('',(0.00659624900930953,0.00586418860079725,0.00391930938864474));
#26968=CARTESIAN_POINT('',(0.00729013620410225,0.00608090266052671,0.00239278007335497));
#26969=CARTESIAN_POINT('',(0.00763368039017796,0.00651433077998561,-0.000773574027082154));
#26970=CARTESIAN_POINT('',(0.00728333738146094,0.00673104483971505,-0.00241339881222951));
#26971=CARTESIAN_POINT('',(0.00567588064395429,0.00716447295917395,-0.00516293263047764));
#26972=CARTESIAN_POINT('',(0.00441876691516466,0.00738118701890338,-0.00627264166357842));
#26973=CARTESIAN_POINT('',(0.00149104038550943,0.00781461513836225,-0.00752649989047846));
#26974=CARTESIAN_POINT('',(-0.00017957241535618,0.00803132919809169,-0.00767064908427772));
#26975=CARTESIAN_POINT('',(-0.00327886382272879,0.00846475731755054,-0.00693692938537633));
#26976=CARTESIAN_POINT('',(-0.00470754242923578,0.00868147137727995,-0.00605906049267568));
#26977=CARTESIAN_POINT('',(-0.0067621497123009,0.00911489949673877,-0.00362537506849006));
#26978=CARTESIAN_POINT('',(-0.00738807838885903,0.00933161355646818,-0.00206955853700509));
#26979=CARTESIAN_POINT('',(-0.00757049102455984,0.0097183707363477,0.000765979361480661));
#26980=CARTESIAN_POINT('',(-0.00732825785442074,0.00988841385649782,0.00203300301339187));
#26981=CARTESIAN_POINT('',(-0.00680271503673493,0.0100584569766479,0.00316793209498262));
#26982=CARTESIAN_POINT('',(0.00749116145915708,-6.75281602410481E-5,0.000441218788658249));
#26983=CARTESIAN_POINT('',(0.00756200120481795,0.000102510692584639,-0.000807439434836002));
#26984=CARTESIAN_POINT('',(0.00732081695293276,0.000272549545410328,-0.00207462176569003));
#26985=CARTESIAN_POINT('',(0.00610743391275447,0.000659302457965472,-0.004643861796793));
#26986=CARTESIAN_POINT('',(0.00495274654093002,0.000876016517694927,-0.00586001206115835));
#26987=CARTESIAN_POINT('',(0.00214655393402308,0.00130944463715384,-0.00736647150889449));
#26988=CARTESIAN_POINT('',(0.000495048698940571,0.00152615869688331,-0.00765678069226526));
#26989=CARTESIAN_POINT('',(-0.00265669013019172,0.00195958681634223,-0.00719809194890018));
#26990=CARTESIAN_POINT('',(-0.0041569237242415,0.0021763008760717,-0.00644909402216432));
#26991=CARTESIAN_POINT('',(-0.00641749573444313,0.00260972899553063,-0.00420555697983189));
#26992=CARTESIAN_POINT('',(-0.00717783415059498,0.00282644305526009,-0.00271101786423531));
#26993=CARTESIAN_POINT('',(-0.00766027528874288,0.00325987117471903,0.000437157022235508));
#26994=CARTESIAN_POINT('',(-0.00738237801073893,0.00347658523444849,0.00209079279310975));
#26995=CARTESIAN_POINT('',(-0.00589738808135971,0.00391001335390743,0.00490833196657945));
#26996=CARTESIAN_POINT('',(-0.00469029542998442,0.0041267274136369,0.00607223536917492));
#26997=CARTESIAN_POINT('',(-0.00182054162059236,0.00456015553309583,0.0074536263691168));
#26998=CARTESIAN_POINT('',(-0.000157880462575577,0.00477686959282529,0.00767111396646321));
#26999=CARTESIAN_POINT('',(0.00297063148578507,0.00521029771228422,0.00707433843568374));
#27000=CARTESIAN_POINT('',(0.00443648227612893,0.00542701177201368,0.00626007530755787));
#27001=CARTESIAN_POINT('',(0.00659621688161849,0.00586043989147259,0.00391929029925606));
#27002=CARTESIAN_POINT('',(0.00729010069676417,0.00607715395120205,0.00239276841908012));
#27003=CARTESIAN_POINT('',(0.00763364320957354,0.00651058207066095,-0.000773570259312425));
#27004=CARTESIAN_POINT('',(0.00728330190723721,0.0067272961303904,-0.00241338705752903));
#27005=CARTESIAN_POINT('',(0.0056758529990095,0.00716072424984929,-0.00516290748389749));
#27006=CARTESIAN_POINT('',(0.00441874539311811,0.00737743830957873,-0.00627261111204935));
#27007=CARTESIAN_POINT('',(0.00149103312324799,0.0078108664290376,-0.00752646323190739));
#27008=CARTESIAN_POINT('',(-0.000179571540730757,0.00802758048876703,-0.00767061172361357));
#27009=CARTESIAN_POINT('',(-0.00327884785269434,0.00846100860822588,-0.00693689559836742));
#27010=CARTESIAN_POINT('',(-0.00470751950067918,0.00867772266795529,-0.00605903098141508));
#27011=CARTESIAN_POINT('',(-0.00676211677657388,0.00911115078741411,-0.00362535741073791));
#27012=CARTESIAN_POINT('',(-0.00738804240448374,0.00932786484714353,-0.00206954845701308));
#27013=CARTESIAN_POINT('',(-0.00757045415172555,0.00971462202702305,0.000765975630701511));
#27014=CARTESIAN_POINT('',(-0.00732822216140734,0.00988466514717316,0.0020329931114472));
#27015=CARTESIAN_POINT('',(-0.00680268190343044,0.0100547082673233,0.00316791666525226));
#27016=CARTESIAN_POINT('',(0.00749108869504174,-7.12762246428155E-5,0.000441214502955024));
#27017=CARTESIAN_POINT('',(0.00756192775261285,9.87626281828712E-5,-0.000807431591911178));
#27018=CARTESIAN_POINT('',(0.00732074584342964,0.000268801481008561,-0.0020746016142064));
#27019=CARTESIAN_POINT('',(0.00610737458923994,0.000655554393563705,-0.00464381668943585));
#27020=CARTESIAN_POINT('',(0.00495269843327375,0.00087226845329316,-0.00585995514093365));
#27021=CARTESIAN_POINT('',(0.00214653308383864,0.00130569657275208,-0.00736639995593364));
#27022=CARTESIAN_POINT('',(0.000495043890369721,0.00152241063248154,-0.00765670631943583));
#27023=CARTESIAN_POINT('',(-0.00265666432488661,0.00195583875194046,-0.00719802203146539));
#27024=CARTESIAN_POINT('',(-0.00415688334667402,0.00217255281166993,-0.00644903137999276));
#27025=CARTESIAN_POINT('',(-0.00641743339919614,0.00260598093112886,-0.00420551612987359));
#27026=CARTESIAN_POINT('',(-0.00717776442993084,0.00282269499085832,-0.00271099153122705));
#27027=CARTESIAN_POINT('',(-0.00766020088196928,0.00325612311031726,0.000437152775985556));
#27028=CARTESIAN_POINT('',(-0.007382306303273,0.00347283717004673,0.00209077248455162));
#27029=CARTESIAN_POINT('',(-0.00589733079808942,0.00390626528950566,0.00490828429033655));
#27030=CARTESIAN_POINT('',(-0.00469024987160212,0.00412297934923513,0.00607217638755542));
#27031=CARTESIAN_POINT('',(-0.00182052393707276,0.00455640746869406,0.00745355396959213));
#27032=CARTESIAN_POINT('',(-0.000157878929030712,0.00477312152842352,0.00767103945440996));
#27033=CARTESIAN_POINT('',(0.0029706026310643,0.00520654964788245,0.00707426972030753));
#27034=CARTESIAN_POINT('',(0.00443643918311728,0.00542326370761191,0.00626001450138726));
#27035=CARTESIAN_POINT('',(0.0065961528103942,0.00585669182707082,0.0039192522299002));
#27036=CARTESIAN_POINT('',(0.00729002988561815,0.00607340588680028,0.0023927451773334));
#27037=CARTESIAN_POINT('',(0.00763356906148608,0.00650683400625918,-0.000773562745370043));
#27038=CARTESIAN_POINT('',(0.00728323116213006,0.00672354806598863,-0.0024133636155067));
#27039=CARTESIAN_POINT('',(0.00567579786758234,0.00715697618544752,-0.00516285733487884));
#27040=CARTESIAN_POINT('',(0.00441870247239064,0.00737369024517696,-0.00627255018411434));
#27041=CARTESIAN_POINT('',(0.00149101864035281,0.00780711836463583,-0.00752639012489431));
#27042=CARTESIAN_POINT('',(-0.000179569796493315,0.00802383242436526,-0.00767053721643878));
#27043=CARTESIAN_POINT('',(-0.00327881600416663,0.00845726054382411,-0.00693682821801869));
#27044=CARTESIAN_POINT('',(-0.00470747377499381,0.00867397460355352,-0.00605897212805414));
#27045=CARTESIAN_POINT('',(-0.00676205109390934,0.00910740272301235,-0.00362532219644888));
#27046=CARTESIAN_POINT('',(-0.00738797064199769,0.00932411678274176,-0.00206952835480817));
#27047=CARTESIAN_POINT('',(-0.0075703806174142,0.00971087396262128,0.000765968190528255));
#27048=CARTESIAN_POINT('',(-0.00732815097997499,0.0098809170827714,0.00203297336431639));
#27049=CARTESIAN_POINT('',(-0.00680261582674348,0.0100509602029215,0.00316788589423566));
#27050=CARTESIAN_POINT('',(0.000131278242483219,-1.40404000692663E-7,0.0226185807277614));
#27051=CARTESIAN_POINT('',(-0.0175237463973022,0.0219318294183615,0.0829676293941348));
#27052=CARTESIAN_POINT('',(-0.0175118732224913,0.0219317957695828,0.0829683295255001));
#27053=CARTESIAN_POINT('',(-0.0175,0.0219317957695827,0.0829690291284178));
#27054=CARTESIAN_POINT('',(-0.0152548287001133,0.0219317957695827,0.0831013207950845));
#27055=CARTESIAN_POINT('',(-0.0133104533185637,0.0230543814195261,0.0832336124617511));
#27056=CARTESIAN_POINT('',(-0.0113660779370141,0.0241769670694694,0.0833659041284178));
#27057=CARTESIAN_POINT('',(-0.0102434922870708,0.0261213424510191,0.0834981957950845));
#27058=CARTESIAN_POINT('',(-0.00912090663712744,0.0280657178325686,0.0836304874617511));
#27059=CARTESIAN_POINT('',(-0.00912090663712744,0.0303108891324553,0.0837627791284178));
#27060=CARTESIAN_POINT('',(-0.00912090663712744,0.0325560604323421,0.0838950707950844));
#27061=CARTESIAN_POINT('',(-0.0102434922870708,0.0345004358138917,0.0840273624617511));
#27062=CARTESIAN_POINT('',(-0.0113660779370142,0.0364448111954412,0.0841596541284179));
#27063=CARTESIAN_POINT('',(-0.0133104533185638,0.0375673968453846,0.0842919457950845));
#27064=CARTESIAN_POINT('',(-0.0152548287001134,0.038689982495328,0.0844242374617512));
#27065=CARTESIAN_POINT('',(-0.0175,0.038689982495328,0.0845565291284178));
#27066=CARTESIAN_POINT('',(-0.0197451712998867,0.038689982495328,0.0846888207950845));
#27067=CARTESIAN_POINT('',(-0.0216895466814364,0.0375673968453846,0.0848211124617511));
#27068=CARTESIAN_POINT('',(-0.023633922062986,0.0364448111954412,0.0849534041284178));
#27069=CARTESIAN_POINT('',(-0.0247565077129293,0.0345004358138917,0.0850856957950845));
#27070=CARTESIAN_POINT('',(-0.0258790933628727,0.032556060432342,0.0852179874617511));
#27071=CARTESIAN_POINT('',(-0.0258790933628727,0.0303108891324553,0.0853502791284178));
#27072=CARTESIAN_POINT('',(-0.0258790933628727,0.0280657178325686,0.0854825707950845));
#27073=CARTESIAN_POINT('',(-0.0247565077129293,0.0261213424510191,0.0856148624617511));
#27074=CARTESIAN_POINT('',(-0.023633922062986,0.0241769670694694,0.0857471541284178));
#27075=CARTESIAN_POINT('',(-0.0216895466814364,0.0230543814195261,0.0858794457950845));
#27076=CARTESIAN_POINT('',(-0.0197451712998867,0.0219317957695827,0.0860117374617512));
#27077=CARTESIAN_POINT('',(-0.0175,0.0219317957695827,0.0861440291284178));
#27078=CARTESIAN_POINT('',(-0.0152548287001133,0.0219317957695827,0.0862763207950845));
#27079=CARTESIAN_POINT('',(-0.0133104533185637,0.0230543814195261,0.0864086124617511));
#27080=CARTESIAN_POINT('',(-0.0113660779370141,0.0241769670694694,0.0865409041284178));
#27081=CARTESIAN_POINT('',(-0.0102434922870708,0.0261213424510191,0.0866731957950845));
#27082=CARTESIAN_POINT('',(-0.00912090663712744,0.0280657178325686,0.0868054874617512));
#27083=CARTESIAN_POINT('',(-0.00912090663712744,0.0303108891324553,0.0869377791284178));
#27084=CARTESIAN_POINT('',(-0.00912090663712744,0.0325560604323421,0.0870700707950845));
#27085=CARTESIAN_POINT('',(-0.0102434922870708,0.0345004358138917,0.0872023624617511));
#27086=CARTESIAN_POINT('',(-0.0113660779370142,0.0364448111954412,0.0873346541284179));
#27087=CARTESIAN_POINT('',(-0.0133104533185638,0.0375673968453846,0.0874669457950845));
#27088=CARTESIAN_POINT('',(-0.0152548287001134,0.038689982495328,0.0875992374617512));
#27089=CARTESIAN_POINT('',(-0.0175,0.038689982495328,0.0877315291284178));
#27090=CARTESIAN_POINT('',(-0.0197451712998867,0.038689982495328,0.0878638207950845));
#27091=CARTESIAN_POINT('',(-0.0216895466814364,0.0375673968453846,0.0879961124617511));
#27092=CARTESIAN_POINT('',(-0.023633922062986,0.0364448111954412,0.0881284041284178));
#27093=CARTESIAN_POINT('',(-0.0247565077129293,0.0345004358138917,0.0882606957950845));
#27094=CARTESIAN_POINT('',(-0.0258790933628727,0.032556060432342,0.0883929874617511));
#27095=CARTESIAN_POINT('',(-0.0258790933628727,0.0303108891324553,0.0885252791284178));
#27096=CARTESIAN_POINT('',(-0.0175233864785942,0.0220588289083546,0.0829452358675848));
#27097=CARTESIAN_POINT('',(-0.017511693262776,0.0220587957695827,0.0829459359989501));
#27098=CARTESIAN_POINT('',(-0.0175,0.0220587957695827,0.0829466356018678));
#27099=CARTESIAN_POINT('',(-0.0152888582475521,0.0220587957695827,0.0830789272685345));
#27100=CARTESIAN_POINT('',(-0.0133739533185637,0.0231643666458067,0.0832112189352011));
#27101=CARTESIAN_POINT('',(-0.0114590483895754,0.0242699375220307,0.0833435106018678));
#27102=CARTESIAN_POINT('',(-0.0103534775133514,0.0261848424510191,0.0834758022685346));
#27103=CARTESIAN_POINT('',(-0.00924790663712745,0.0280997473800074,0.0836080939352012));
#27104=CARTESIAN_POINT('',(-0.00924790663712744,0.0303108891324553,0.0837403856018679));
#27105=CARTESIAN_POINT('',(-0.00924790663712745,0.0325220308849033,0.0838726772685345));
#27106=CARTESIAN_POINT('',(-0.0103534775133514,0.0344369358138917,0.0840049689352011));
#27107=CARTESIAN_POINT('',(-0.0114590483895754,0.03635184074288,0.0841372606018679));
#27108=CARTESIAN_POINT('',(-0.0133739533185638,0.037457411619104,0.0842695522685344));
#27109=CARTESIAN_POINT('',(-0.0152888582475521,0.0385629824953279,0.0844018439352012));
#27110=CARTESIAN_POINT('',(-0.0175,0.0385629824953279,0.0845341356018678));
#27111=CARTESIAN_POINT('',(-0.019711141752448,0.0385629824953279,0.0846664272685345));
#27112=CARTESIAN_POINT('',(-0.0216260466814364,0.037457411619104,0.0847987189352012));
#27113=CARTESIAN_POINT('',(-0.0235409516104247,0.03635184074288,0.0849310106018678));
#27114=CARTESIAN_POINT('',(-0.0246465224866487,0.0344369358138917,0.0850633022685345));
#27115=CARTESIAN_POINT('',(-0.0257520933628727,0.0325220308849033,0.0851955939352012));
#27116=CARTESIAN_POINT('',(-0.0257520933628727,0.0303108891324553,0.0853278856018678));
#27117=CARTESIAN_POINT('',(-0.0257520933628727,0.0280997473800074,0.0854601772685345));
#27118=CARTESIAN_POINT('',(-0.0246465224866487,0.026184842451019,0.0855924689352011));
#27119=CARTESIAN_POINT('',(-0.0235409516104247,0.0242699375220307,0.0857247606018678));
#27120=CARTESIAN_POINT('',(-0.0216260466814364,0.0231643666458067,0.0858570522685345));
#27121=CARTESIAN_POINT('',(-0.019711141752448,0.0220587957695827,0.0859893439352011));
#27122=CARTESIAN_POINT('',(-0.0175,0.0220587957695827,0.0861216356018678));
#27123=CARTESIAN_POINT('',(-0.0152888582475521,0.0220587957695827,0.0862539272685345));
#27124=CARTESIAN_POINT('',(-0.0133739533185637,0.0231643666458067,0.0863862189352011));
#27125=CARTESIAN_POINT('',(-0.0114590483895754,0.0242699375220307,0.0865185106018678));
#27126=CARTESIAN_POINT('',(-0.0103534775133514,0.0261848424510191,0.0866508022685344));
#27127=CARTESIAN_POINT('',(-0.00924790663712745,0.0280997473800074,0.0867830939352012));
#27128=CARTESIAN_POINT('',(-0.00924790663712744,0.0303108891324553,0.0869153856018678));
#27129=CARTESIAN_POINT('',(-0.00924790663712745,0.0325220308849033,0.0870476772685344));
#27130=CARTESIAN_POINT('',(-0.0103534775133514,0.0344369358138917,0.0871799689352011));
#27131=CARTESIAN_POINT('',(-0.0114590483895754,0.03635184074288,0.0873122606018678));
#27132=CARTESIAN_POINT('',(-0.0133739533185638,0.037457411619104,0.0874445522685345));
#27133=CARTESIAN_POINT('',(-0.0152888582475521,0.0385629824953279,0.0875768439352012));
#27134=CARTESIAN_POINT('',(-0.0175,0.0385629824953279,0.0877091356018679));
#27135=CARTESIAN_POINT('',(-0.019711141752448,0.0385629824953279,0.0878414272685345));
#27136=CARTESIAN_POINT('',(-0.0216260466814364,0.037457411619104,0.0879737189352012));
#27137=CARTESIAN_POINT('',(-0.0235409516104247,0.03635184074288,0.0881060106018679));
#27138=CARTESIAN_POINT('',(-0.0246465224866487,0.0344369358138917,0.0882383022685345));
#27139=CARTESIAN_POINT('',(-0.0257520933628727,0.0325220308849033,0.0883705939352012));
#27140=CARTESIAN_POINT('',(-0.0257520933628727,0.0303108891324553,0.0885028856018678));
#27141=CARTESIAN_POINT('',(-0.0175231515583417,0.0221417219383439,0.0828464474045792));
#27142=CARTESIAN_POINT('',(-0.0175115758024139,0.0221416891324553,0.0828471475359445));
#27143=CARTESIAN_POINT('',(-0.0175,0.0221416891324553,0.0828478471388622));
#27144=CARTESIAN_POINT('',(-0.0153110694571917,0.0221416891324553,0.0829801388055289));
#27145=CARTESIAN_POINT('',(-0.0134154,0.0232361544038595,0.0831124304721955));
#27146=CARTESIAN_POINT('',(-0.0115197305428084,0.0243306196752637,0.0832447221388622));
#27147=CARTESIAN_POINT('',(-0.0104252652714042,0.0262262891324553,0.0833770138055289));
#27148=CARTESIAN_POINT('',(-0.00933080000000003,0.028121958589647,0.0835093054721956));
#27149=CARTESIAN_POINT('',(-0.00933080000000004,0.0303108891324554,0.0836415971388622));
#27150=CARTESIAN_POINT('',(-0.00933080000000005,0.0324998196752637,0.0837738888055289));
#27151=CARTESIAN_POINT('',(-0.0104252652714042,0.0343954891324554,0.0839061804721955));
#27152=CARTESIAN_POINT('',(-0.0115197305428084,0.0362911585896471,0.0840384721388623));
#27153=CARTESIAN_POINT('',(-0.0134154000000001,0.0373856238610512,0.0841707638055288));
#27154=CARTESIAN_POINT('',(-0.0153110694571917,0.0384800891324554,0.0843030554721955));
#27155=CARTESIAN_POINT('',(-0.0175,0.0384800891324553,0.0844353471388622));
#27156=CARTESIAN_POINT('',(-0.0196889305428084,0.0384800891324554,0.0845676388055289));
#27157=CARTESIAN_POINT('',(-0.0215846,0.0373856238610511,0.0846999304721956));
#27158=CARTESIAN_POINT('',(-0.0234802694571917,0.036291158589647,0.0848322221388622));
#27159=CARTESIAN_POINT('',(-0.0245747347285959,0.0343954891324553,0.0849645138055289));
#27160=CARTESIAN_POINT('',(-0.0256692000000001,0.0324998196752637,0.0850968054721956));
#27161=CARTESIAN_POINT('',(-0.0256692,0.0303108891324553,0.0852290971388622));
#27162=CARTESIAN_POINT('',(-0.0256692000000001,0.028121958589647,0.0853613888055289));
#27163=CARTESIAN_POINT('',(-0.0245747347285959,0.0262262891324553,0.0854936804721955));
#27164=CARTESIAN_POINT('',(-0.0234802694571917,0.0243306196752637,0.0856259721388622));
#27165=CARTESIAN_POINT('',(-0.0215846,0.0232361544038595,0.0857582638055289));
#27166=CARTESIAN_POINT('',(-0.0196889305428084,0.0221416891324553,0.0858905554721955));
#27167=CARTESIAN_POINT('',(-0.0175,0.0221416891324553,0.0860228471388622));
#27168=CARTESIAN_POINT('',(-0.0153110694571917,0.0221416891324553,0.0861551388055289));
#27169=CARTESIAN_POINT('',(-0.0134154,0.0232361544038595,0.0862874304721955));
#27170=CARTESIAN_POINT('',(-0.0115197305428084,0.0243306196752637,0.0864197221388622));
#27171=CARTESIAN_POINT('',(-0.0104252652714042,0.0262262891324553,0.0865520138055288));
#27172=CARTESIAN_POINT('',(-0.00933080000000003,0.028121958589647,0.0866843054721956));
#27173=CARTESIAN_POINT('',(-0.00933080000000004,0.0303108891324554,0.0868165971388622));
#27174=CARTESIAN_POINT('',(-0.00933080000000005,0.0324998196752637,0.086948888805529));
#27175=CARTESIAN_POINT('',(-0.0104252652714042,0.0343954891324554,0.0870811804721955));
#27176=CARTESIAN_POINT('',(-0.0115197305428084,0.0362911585896471,0.0872134721388622));
#27177=CARTESIAN_POINT('',(-0.0134154000000001,0.0373856238610512,0.0873457638055289));
#27178=CARTESIAN_POINT('',(-0.0153110694571917,0.0384800891324554,0.0874780554721955));
#27179=CARTESIAN_POINT('',(-0.0175,0.0384800891324553,0.0876103471388623));
#27180=CARTESIAN_POINT('',(-0.0196889305428084,0.0384800891324554,0.0877426388055289));
#27181=CARTESIAN_POINT('',(-0.0215846,0.0373856238610511,0.0878749304721956));
#27182=CARTESIAN_POINT('',(-0.0234802694571917,0.036291158589647,0.0880072221388623));
#27183=CARTESIAN_POINT('',(-0.0245747347285959,0.0343954891324553,0.0881395138055289));
#27184=CARTESIAN_POINT('',(-0.0256692000000001,0.0324998196752637,0.0882718054721955));
#27185=CARTESIAN_POINT('',(-0.0256692,0.0303108891324553,0.0884040971388622));
#27186=CARTESIAN_POINT('',(-0.0175231515583417,0.0221417219383439,0.0827174882248697));
#27187=CARTESIAN_POINT('',(-0.0175115758024139,0.0221416891324554,0.082718188356235));
#27188=CARTESIAN_POINT('',(-0.0175,0.0221416891324554,0.0827188879591527));
#27189=CARTESIAN_POINT('',(-0.0153110694571917,0.0221416891324553,0.0828511796258194));
#27190=CARTESIAN_POINT('',(-0.0134154,0.0232361544038595,0.082983471292486));
#27191=CARTESIAN_POINT('',(-0.0115197305428084,0.0243306196752637,0.0831157629591527));
#27192=CARTESIAN_POINT('',(-0.0104252652714042,0.0262262891324554,0.0832480546258194));
#27193=CARTESIAN_POINT('',(-0.00933080000000004,0.028121958589647,0.083380346292486));
#27194=CARTESIAN_POINT('',(-0.0093308,0.0303108891324553,0.0835126379591527));
#27195=CARTESIAN_POINT('',(-0.00933080000000005,0.0324998196752637,0.0836449296258193));
#27196=CARTESIAN_POINT('',(-0.0104252652714042,0.0343954891324554,0.083777221292486));
#27197=CARTESIAN_POINT('',(-0.0115197305428084,0.0362911585896471,0.0839095129591528));
#27198=CARTESIAN_POINT('',(-0.0134154,0.0373856238610512,0.0840418046258194));
#27199=CARTESIAN_POINT('',(-0.0153110694571917,0.0384800891324554,0.0841740962924861));
#27200=CARTESIAN_POINT('',(-0.0175,0.0384800891324554,0.0843063879591527));
#27201=CARTESIAN_POINT('',(-0.0196889305428084,0.0384800891324553,0.0844386796258194));
#27202=CARTESIAN_POINT('',(-0.0215846,0.0373856238610511,0.084570971292486));
#27203=CARTESIAN_POINT('',(-0.0234802694571917,0.036291158589647,0.0847032629591527));
#27204=CARTESIAN_POINT('',(-0.0245747347285959,0.0343954891324554,0.0848355546258194));
#27205=CARTESIAN_POINT('',(-0.0256692000000001,0.0324998196752637,0.084967846292486));
#27206=CARTESIAN_POINT('',(-0.0256692,0.0303108891324553,0.0851001379591527));
#27207=CARTESIAN_POINT('',(-0.0256692000000001,0.028121958589647,0.0852324296258194));
#27208=CARTESIAN_POINT('',(-0.0245747347285959,0.0262262891324553,0.085364721292486));
#27209=CARTESIAN_POINT('',(-0.0234802694571917,0.0243306196752637,0.0854970129591527));
#27210=CARTESIAN_POINT('',(-0.0215846,0.0232361544038595,0.0856293046258194));
#27211=CARTESIAN_POINT('',(-0.0196889305428084,0.0221416891324553,0.0857615962924861));
#27212=CARTESIAN_POINT('',(-0.0175,0.0221416891324554,0.0858938879591527));
#27213=CARTESIAN_POINT('',(-0.0153110694571917,0.0221416891324553,0.0860261796258194));
#27214=CARTESIAN_POINT('',(-0.0134154,0.0232361544038595,0.086158471292486));
#27215=CARTESIAN_POINT('',(-0.0115197305428084,0.0243306196752637,0.0862907629591527));
#27216=CARTESIAN_POINT('',(-0.0104252652714042,0.0262262891324554,0.0864230546258194));
#27217=CARTESIAN_POINT('',(-0.00933080000000004,0.028121958589647,0.086555346292486));
#27218=CARTESIAN_POINT('',(-0.0093308,0.0303108891324553,0.0866876379591527));
#27219=CARTESIAN_POINT('',(-0.00933080000000005,0.0324998196752637,0.0868199296258194));
#27220=CARTESIAN_POINT('',(-0.0104252652714042,0.0343954891324554,0.086952221292486));
#27221=CARTESIAN_POINT('',(-0.0115197305428084,0.0362911585896471,0.0870845129591527));
#27222=CARTESIAN_POINT('',(-0.0134154,0.0373856238610512,0.0872168046258194));
#27223=CARTESIAN_POINT('',(-0.0153110694571917,0.0384800891324554,0.0873490962924861));
#27224=CARTESIAN_POINT('',(-0.0175,0.0384800891324554,0.0874813879591527));
#27225=CARTESIAN_POINT('',(-0.0196889305428084,0.0384800891324553,0.0876136796258194));
#27226=CARTESIAN_POINT('',(-0.0215846,0.0373856238610511,0.087745971292486));
#27227=CARTESIAN_POINT('',(-0.0234802694571917,0.036291158589647,0.0878782629591527));
#27228=CARTESIAN_POINT('',(-0.0245747347285959,0.0343954891324554,0.0880105546258194));
#27229=CARTESIAN_POINT('',(-0.0256692000000001,0.0324998196752637,0.088142846292486));
#27230=CARTESIAN_POINT('',(-0.0256692,0.0303108891324553,0.0882751379591527));
#27231=CARTESIAN_POINT('',(-0.0169787305804826,0.0219480257606184,0.0830000000000001));
#27232=CARTESIAN_POINT('',(-0.0150146757293008,0.022070448151928,0.083117660354341));
#27233=CARTESIAN_POINT('',(-0.0133104533185637,0.0230543814195261,0.0832336124617511));
#27234=CARTESIAN_POINT('',(-0.0113660779370141,0.0241769670694694,0.0833659041284178));
#27235=CARTESIAN_POINT('',(-0.0102434922870708,0.0261213424510191,0.0834981957950845));
#27236=CARTESIAN_POINT('',(-0.00912090663712744,0.0280657178325686,0.0836304874617511));
#27237=CARTESIAN_POINT('',(-0.00912090663712744,0.0303108891324553,0.0837627791284178));
#27238=CARTESIAN_POINT('',(-0.00912090663712745,0.0325560604323421,0.0838950707950844));
#27239=CARTESIAN_POINT('',(-0.0102434922870708,0.0345004358138917,0.0840273624617511));
#27240=CARTESIAN_POINT('',(-0.0113660779370142,0.0364448111954413,0.0841596541284179));
#27241=CARTESIAN_POINT('',(-0.0133104533185638,0.0375673968453846,0.0842919457950845));
#27242=CARTESIAN_POINT('',(-0.0152548287001134,0.038689982495328,0.0844242374617512));
#27243=CARTESIAN_POINT('',(-0.0175,0.038689982495328,0.0845565291284178));
#27244=CARTESIAN_POINT('',(-0.0197451712998867,0.038689982495328,0.0846888207950845));
#27245=CARTESIAN_POINT('',(-0.0216895466814364,0.0375673968453846,0.0848211124617511));
#27246=CARTESIAN_POINT('',(-0.023633922062986,0.0364448111954412,0.0849534041284178));
#27247=CARTESIAN_POINT('',(-0.0247565077129293,0.0345004358138917,0.0850856957950845));
#27248=CARTESIAN_POINT('',(-0.0258790933628727,0.032556060432342,0.0852179874617511));
#27249=CARTESIAN_POINT('',(-0.0258790933628727,0.0303108891324553,0.0853502791284178));
#27250=CARTESIAN_POINT('',(-0.0258790933628727,0.0280657178325686,0.0854825707950845));
#27251=CARTESIAN_POINT('',(-0.0247565077129293,0.026121342451019,0.0856148624617511));
#27252=CARTESIAN_POINT('',(-0.023633922062986,0.0241769670694694,0.0857471541284178));
#27253=CARTESIAN_POINT('',(-0.0216895466814364,0.0230543814195261,0.0858794457950845));
#27254=CARTESIAN_POINT('',(-0.0197451712998867,0.0219317957695827,0.0860117374617512));
#27255=CARTESIAN_POINT('',(-0.0175,0.0219317957695827,0.0861440291284178));
#27256=CARTESIAN_POINT('',(-0.0152548287001133,0.0219317957695827,0.0862763207950845));
#27257=CARTESIAN_POINT('',(-0.0133104533185637,0.0230543814195261,0.0864086124617511));
#27258=CARTESIAN_POINT('',(-0.0113660779370141,0.0241769670694694,0.0865409041284178));
#27259=CARTESIAN_POINT('',(-0.0102434922870708,0.0261213424510191,0.0866731957950845));
#27260=CARTESIAN_POINT('',(-0.00912090663712744,0.0280657178325686,0.0868054874617512));
#27261=CARTESIAN_POINT('',(-0.00912090663712744,0.0303108891324553,0.0869377791284178));
#27262=CARTESIAN_POINT('',(-0.00912090663712745,0.0325560604323421,0.0870700707950845));
#27263=CARTESIAN_POINT('',(-0.0102434922870708,0.0345004358138917,0.0872023624617511));
#27264=CARTESIAN_POINT('',(-0.0113660779370142,0.0364448111954413,0.0873346541284178));
#27265=CARTESIAN_POINT('',(-0.0133104533185638,0.0375673968453846,0.0874669457950845));
#27266=CARTESIAN_POINT('',(-0.0152548287001134,0.038689982495328,0.0875992374617512));
#27267=CARTESIAN_POINT('',(-0.0175,0.038689982495328,0.0877315291284178));
#27268=CARTESIAN_POINT('',(-0.0197451712998867,0.038689982495328,0.0878638207950845));
#27269=CARTESIAN_POINT('',(-0.0216895466814364,0.0375673968453846,0.0879961124617511));
#27270=CARTESIAN_POINT('',(-0.023633922062986,0.0364448111954412,0.0881284041284178));
#27271=CARTESIAN_POINT('',(-0.0247565077129293,0.0345004358138917,0.0882606957950845));
#27272=CARTESIAN_POINT('',(-0.0258790933628727,0.032556060432342,0.0883929874617511));
#27273=CARTESIAN_POINT('',(-0.0258790933628727,0.0303108891324553,0.0885252791284178));
#27274=CARTESIAN_POINT('',(-0.0169787305804826,0.0219480257606184,0.083));
#27275=CARTESIAN_POINT('',(-0.0258790933628727,0.0303108891324553,0.0885252791284178));
#27276=CARTESIAN_POINT('',(-0.0169787305804826,0.0219480257606184,0.083));
#27277=CARTESIAN_POINT('',(-0.0168200873191828,0.0220130837286955,0.083));
#27278=CARTESIAN_POINT('',(-0.0164839350506513,0.0220712803175494,0.0829999999999999));
#27279=CARTESIAN_POINT('',(-0.0158244416844979,0.0222361631417369,0.0830000000000002));
#27280=CARTESIAN_POINT('',(-0.0150115364146986,0.0224757860232567,0.0829999999999978));
#27281=CARTESIAN_POINT('',(-0.0140666789792818,0.0228698014663725,0.0830000000000006));
#27282=CARTESIAN_POINT('',(-0.0134711325811131,0.0231961039553641,0.083));
#27283=CARTESIAN_POINT('',(-0.0131818748312345,0.0233762208875518,0.083));
#27284=CARTESIAN_POINT('',(-0.0131818748312345,0.0233762208875518,0.083));
#27285=CARTESIAN_POINT('',(-0.0131818748312345,0.0233762208875518,0.083));
#27286=CARTESIAN_POINT('',(-0.0114470797111507,0.0244564546069068,0.0831245445074173));
#27287=CARTESIAN_POINT('',(-0.0104252652714042,0.0262262891324554,0.0832480546258194));
#27288=CARTESIAN_POINT('',(-0.00933080000000005,0.028121958589647,0.0833803462924859));
#27289=CARTESIAN_POINT('',(-0.0093308,0.0303108891324553,0.0835126379591527));
#27290=CARTESIAN_POINT('',(-0.0093308,0.0303108891324553,0.0835126379591527));
#27291=CARTESIAN_POINT('',(-0.0093308,0.0303108891324553,0.0835126379591527));
#27292=CARTESIAN_POINT('',(-0.00933080000000004,0.0324998196752637,0.0836449296258193));
#27293=CARTESIAN_POINT('',(-0.0104252652714042,0.0343954891324554,0.083777221292486));
#27294=CARTESIAN_POINT('',(-0.0115197305428084,0.0362911585896471,0.0839095129591528));
#27295=CARTESIAN_POINT('',(-0.0134154,0.0373856238610512,0.0840418046258194));
#27296=CARTESIAN_POINT('',(-0.0153110694571917,0.0384800891324554,0.0841740962924861));
#27297=CARTESIAN_POINT('',(-0.0175,0.0384800891324554,0.0843063879591527));
#27298=CARTESIAN_POINT('',(-0.0196889305428084,0.0384800891324553,0.0844386796258194));
#27299=CARTESIAN_POINT('',(-0.0215846,0.0373856238610511,0.084570971292486));
#27300=CARTESIAN_POINT('',(-0.0234802694571917,0.036291158589647,0.0847032629591527));
#27301=CARTESIAN_POINT('',(-0.0245747347285959,0.0343954891324554,0.0848355546258194));
#27302=CARTESIAN_POINT('',(-0.0256692000000001,0.0324998196752637,0.084967846292486));
#27303=CARTESIAN_POINT('',(-0.0256692,0.0303108891324553,0.0851001379591527));
#27304=CARTESIAN_POINT('',(-0.0256692,0.0303108891324553,0.0851001379591527));
#27305=CARTESIAN_POINT('',(-0.0256692,0.0303108891324553,0.0851001379591527));
#27306=CARTESIAN_POINT('',(-0.0256692,0.028121958589647,0.0852324296258194));
#27307=CARTESIAN_POINT('',(-0.0245747347285959,0.0262262891324553,0.085364721292486));
#27308=CARTESIAN_POINT('',(-0.0234802694571917,0.0243306196752637,0.0854970129591527));
#27309=CARTESIAN_POINT('',(-0.0215846,0.0232361544038595,0.0856293046258194));
#27310=CARTESIAN_POINT('',(-0.0196889305428084,0.0221416891324553,0.0857615962924861));
#27311=CARTESIAN_POINT('',(-0.0175,0.0221416891324554,0.0858938879591527));
#27312=CARTESIAN_POINT('',(-0.0153110694571917,0.0221416891324553,0.0860261796258194));
#27313=CARTESIAN_POINT('',(-0.0134154,0.0232361544038595,0.086158471292486));
#27314=CARTESIAN_POINT('',(-0.0115197305428084,0.0243306196752637,0.0862907629591527));
#27315=CARTESIAN_POINT('',(-0.0104252652714042,0.0262262891324554,0.0864230546258194));
#27316=CARTESIAN_POINT('',(-0.00933080000000006,0.028121958589647,0.0865553462924861));
#27317=CARTESIAN_POINT('',(-0.0093308,0.0303108891324553,0.0866876379591526));
#27318=CARTESIAN_POINT('',(-0.0093308,0.0303108891324553,0.0866876379591527));
#27319=CARTESIAN_POINT('',(-0.0093308,0.0303108891324553,0.0866876379591527));
#27320=CARTESIAN_POINT('',(-0.00933080000000003,0.0324998196752637,0.0868199296258194));
#27321=CARTESIAN_POINT('',(-0.0104252652714042,0.0343954891324554,0.086952221292486));
#27322=CARTESIAN_POINT('',(-0.0115197305428084,0.0362911585896471,0.0870845129591527));
#27323=CARTESIAN_POINT('',(-0.0134154,0.0373856238610512,0.0872168046258194));
#27324=CARTESIAN_POINT('',(-0.0153110694571917,0.0384800891324554,0.0873490962924861));
#27325=CARTESIAN_POINT('',(-0.0175,0.0384800891324554,0.0874813879591527));
#27326=CARTESIAN_POINT('',(-0.0196889305428084,0.0384800891324553,0.0876136796258194));
#27327=CARTESIAN_POINT('',(-0.0215846,0.0373856238610511,0.087745971292486));
#27328=CARTESIAN_POINT('',(-0.0234802694571917,0.036291158589647,0.0878782629591527));
#27329=CARTESIAN_POINT('',(-0.0245747347285959,0.0343954891324554,0.0880105546258194));
#27330=CARTESIAN_POINT('',(-0.0256692000000001,0.0324998196752637,0.088142846292486));
#27331=CARTESIAN_POINT('',(-0.0256692,0.0303108891324553,0.0882751379591527));
#27332=CARTESIAN_POINT('',(-0.0256692,0.0303108891324553,0.0882751379591527));
#27333=CARTESIAN_POINT('',(-0.0259232,0.0303108891324553,0.0882751379591527));
#27334=CARTESIAN_POINT('',(-0.019581657813752,0.0215281047350537,0.0829656841085059));
#27335=CARTESIAN_POINT('',(-0.0185550497149152,0.0212847824953279,0.0830254048361197));
#27336=CARTESIAN_POINT('',(-0.0175,0.021284782495328,0.0830831150255454));
#27337=CARTESIAN_POINT('',(-0.0150814620157846,0.021284782495328,0.0832154066922121));
#27338=CARTESIAN_POINT('',(-0.0129869466814363,0.0224940514874357,0.0833476983588788));
#27339=CARTESIAN_POINT('',(-0.0108924313470881,0.0237033204795435,0.0834799900255455));
#27340=CARTESIAN_POINT('',(-0.00968316235498038,0.0257978358138917,0.0836122816922121));
#27341=CARTESIAN_POINT('',(-0.00847389336287265,0.0278923511482399,0.0837445733588788));
#27342=CARTESIAN_POINT('',(-0.00847389336287264,0.0303108891324553,0.0838768650255454));
#27343=CARTESIAN_POINT('',(-0.00847389336287266,0.0327294271166709,0.0840091566922122));
#27344=CARTESIAN_POINT('',(-0.00968316235498039,0.0348239424510191,0.0841414483588788));
#27345=CARTESIAN_POINT('',(-0.0108924313470881,0.0369184577853673,0.0842737400255455));
#27346=CARTESIAN_POINT('',(-0.0129869466814364,0.038127726777475,0.0844060316922121));
#27347=CARTESIAN_POINT('',(-0.0150814620157846,0.0393369957695828,0.0845383233588788));
#27348=CARTESIAN_POINT('',(-0.0175,0.0393369957695828,0.0846706150255454));
#27349=CARTESIAN_POINT('',(-0.0199185379842156,0.0393369957695828,0.0848029066922121));
#27350=CARTESIAN_POINT('',(-0.0220130533185638,0.038127726777475,0.0849351983588788));
#27351=CARTESIAN_POINT('',(-0.024107568652912,0.0369184577853673,0.0850674900255454));
#27352=CARTESIAN_POINT('',(-0.0253168376450197,0.0348239424510191,0.0851997816922121));
#27353=CARTESIAN_POINT('',(-0.0265261066371274,0.0327294271166708,0.0853320733588788));
#27354=CARTESIAN_POINT('',(-0.0265261066371274,0.0303108891324553,0.0854643650255454));
#27355=CARTESIAN_POINT('',(-0.0265261066371274,0.0278923511482398,0.0855966566922121));
#27356=CARTESIAN_POINT('',(-0.0253168376450197,0.0257978358138916,0.0857289483588788));
#27357=CARTESIAN_POINT('',(-0.024107568652912,0.0237033204795434,0.0858612400255455));
#27358=CARTESIAN_POINT('',(-0.0220130533185638,0.0224940514874356,0.0859935316922121));
#27359=CARTESIAN_POINT('',(-0.0199185379842155,0.0212847824953279,0.0861258233588788));
#27360=CARTESIAN_POINT('',(-0.0175,0.021284782495328,0.0862581150255454));
#27361=CARTESIAN_POINT('',(-0.0150814620157846,0.021284782495328,0.0863904066922121));
#27362=CARTESIAN_POINT('',(-0.0129869466814363,0.0224940514874357,0.0865226983588788));
#27363=CARTESIAN_POINT('',(-0.0108924313470881,0.0237033204795435,0.0866549900255455));
#27364=CARTESIAN_POINT('',(-0.00968316235498038,0.0257978358138917,0.0867872816922121));
#27365=CARTESIAN_POINT('',(-0.00847389336287265,0.0278923511482399,0.0869195733588788));
#27366=CARTESIAN_POINT('',(-0.00847389336287264,0.0303108891324553,0.0870518650255454));
#27367=CARTESIAN_POINT('',(-0.00847389336287266,0.0327294271166709,0.0871841566922122));
#27368=CARTESIAN_POINT('',(-0.00968316235498039,0.0348239424510191,0.0873164483588788));
#27369=CARTESIAN_POINT('',(-0.0108924313470881,0.0369184577853673,0.0874487400255455));
#27370=CARTESIAN_POINT('',(-0.0129869466814364,0.038127726777475,0.0875810316922121));
#27371=CARTESIAN_POINT('',(-0.0150814620157846,0.0393369957695828,0.0877133233588788));
#27372=CARTESIAN_POINT('',(-0.0175,0.0393369957695828,0.0878456150255454));
#27373=CARTESIAN_POINT('',(-0.0199185379842156,0.0393369957695828,0.0879779066922121));
#27374=CARTESIAN_POINT('',(-0.0220130533185638,0.038127726777475,0.0881101983588788));
#27375=CARTESIAN_POINT('',(-0.024107568652912,0.0369184577853673,0.0882424900255454));
#27376=CARTESIAN_POINT('',(-0.0253168376450197,0.0348239424510191,0.0883747816922121));
#27377=CARTESIAN_POINT('',(-0.0265261066371274,0.0327294271166708,0.0885070733588787));
#27378=CARTESIAN_POINT('',(-0.0265261066371274,0.0303108891324553,0.0886393650255454));
#27379=CARTESIAN_POINT('',(-0.0194324395192978,0.0221576760794319,0.0828515982113783));
#27380=CARTESIAN_POINT('',(-0.0184794211855844,0.0219317957695827,0.0829113189389921));
#27381=CARTESIAN_POINT('',(-0.0175,0.0219317957695827,0.0829690291284178));
#27382=CARTESIAN_POINT('',(-0.0152548287001133,0.0219317957695827,0.0831013207950845));
#27383=CARTESIAN_POINT('',(-0.0133104533185637,0.0230543814195261,0.0832336124617511));
#27384=CARTESIAN_POINT('',(-0.0113660779370141,0.0241769670694694,0.0833659041284178));
#27385=CARTESIAN_POINT('',(-0.0102434922870708,0.0261213424510191,0.0834981957950845));
#27386=CARTESIAN_POINT('',(-0.00912090663712744,0.0280657178325686,0.0836304874617511));
#27387=CARTESIAN_POINT('',(-0.00912090663712744,0.0303108891324553,0.0837627791284178));
#27388=CARTESIAN_POINT('',(-0.00912090663712745,0.0325560604323421,0.0838950707950844));
#27389=CARTESIAN_POINT('',(-0.0102434922870708,0.0345004358138917,0.0840273624617511));
#27390=CARTESIAN_POINT('',(-0.0113660779370142,0.0364448111954413,0.0841596541284179));
#27391=CARTESIAN_POINT('',(-0.0133104533185638,0.0375673968453846,0.0842919457950845));
#27392=CARTESIAN_POINT('',(-0.0152548287001134,0.038689982495328,0.0844242374617512));
#27393=CARTESIAN_POINT('',(-0.0175,0.038689982495328,0.0845565291284178));
#27394=CARTESIAN_POINT('',(-0.0197451712998867,0.038689982495328,0.0846888207950845));
#27395=CARTESIAN_POINT('',(-0.0216895466814364,0.0375673968453846,0.0848211124617511));
#27396=CARTESIAN_POINT('',(-0.023633922062986,0.0364448111954412,0.0849534041284178));
#27397=CARTESIAN_POINT('',(-0.0247565077129293,0.0345004358138917,0.0850856957950845));
#27398=CARTESIAN_POINT('',(-0.0258790933628727,0.032556060432342,0.0852179874617511));
#27399=CARTESIAN_POINT('',(-0.0258790933628727,0.0303108891324553,0.0853502791284178));
#27400=CARTESIAN_POINT('',(-0.0258790933628727,0.0280657178325686,0.0854825707950845));
#27401=CARTESIAN_POINT('',(-0.0247565077129293,0.026121342451019,0.0856148624617511));
#27402=CARTESIAN_POINT('',(-0.023633922062986,0.0241769670694694,0.0857471541284178));
#27403=CARTESIAN_POINT('',(-0.0216895466814364,0.0230543814195261,0.0858794457950845));
#27404=CARTESIAN_POINT('',(-0.0197451712998867,0.0219317957695827,0.0860117374617512));
#27405=CARTESIAN_POINT('',(-0.0175,0.0219317957695827,0.0861440291284178));
#27406=CARTESIAN_POINT('',(-0.0152548287001133,0.0219317957695827,0.0862763207950845));
#27407=CARTESIAN_POINT('',(-0.0133104533185637,0.0230543814195261,0.0864086124617511));
#27408=CARTESIAN_POINT('',(-0.0113660779370141,0.0241769670694694,0.0865409041284178));
#27409=CARTESIAN_POINT('',(-0.0102434922870708,0.0261213424510191,0.0866731957950845));
#27410=CARTESIAN_POINT('',(-0.00912090663712744,0.0280657178325686,0.0868054874617512));
#27411=CARTESIAN_POINT('',(-0.00912090663712744,0.0303108891324553,0.0869377791284178));
#27412=CARTESIAN_POINT('',(-0.00912090663712745,0.0325560604323421,0.0870700707950845));
#27413=CARTESIAN_POINT('',(-0.0102434922870708,0.0345004358138917,0.0872023624617511));
#27414=CARTESIAN_POINT('',(-0.0113660779370142,0.0364448111954413,0.0873346541284179));
#27415=CARTESIAN_POINT('',(-0.0133104533185638,0.0375673968453846,0.0874669457950845));
#27416=CARTESIAN_POINT('',(-0.0152548287001134,0.038689982495328,0.0875992374617512));
#27417=CARTESIAN_POINT('',(-0.0175,0.038689982495328,0.0877315291284178));
#27418=CARTESIAN_POINT('',(-0.0197451712998867,0.038689982495328,0.0878638207950845));
#27419=CARTESIAN_POINT('',(-0.0216895466814364,0.0375673968453846,0.0879961124617511));
#27420=CARTESIAN_POINT('',(-0.023633922062986,0.0364448111954412,0.0881284041284178));
#27421=CARTESIAN_POINT('',(-0.0247565077129293,0.0345004358138917,0.0882606957950845));
#27422=CARTESIAN_POINT('',(-0.0258790933628727,0.032556060432342,0.0883929874617511));
#27423=CARTESIAN_POINT('',(-0.0258790933628727,0.0303108891324553,0.0885252791284178));
#27424=CARTESIAN_POINT('',(-0.0189864747528493,0.0214080247712547,0.083));
#27425=CARTESIAN_POINT('',(-0.0182483463291824,0.0212847824953279,0.0830421812119037));
#27426=CARTESIAN_POINT('',(-0.0175,0.021284782495328,0.0830831150255454));
#27427=CARTESIAN_POINT('',(-0.0150814620157846,0.021284782495328,0.0832154066922121));
#27428=CARTESIAN_POINT('',(-0.0129869466814363,0.0224940514874357,0.0833476983588788));
#27429=CARTESIAN_POINT('',(-0.0108924313470881,0.0237033204795435,0.0834799900255455));
#27430=CARTESIAN_POINT('',(-0.00968316235498038,0.0257978358138917,0.0836122816922121));
#27431=CARTESIAN_POINT('',(-0.00847389336287265,0.0278923511482399,0.0837445733588788));
#27432=CARTESIAN_POINT('',(-0.00847389336287265,0.0303108891324553,0.0838768650255454));
#27433=CARTESIAN_POINT('',(-0.00847389336287266,0.0327294271166709,0.0840091566922122));
#27434=CARTESIAN_POINT('',(-0.00968316235498039,0.0348239424510191,0.0841414483588788));
#27435=CARTESIAN_POINT('',(-0.0108924313470881,0.0369184577853673,0.0842737400255455));
#27436=CARTESIAN_POINT('',(-0.0129869466814364,0.038127726777475,0.0844060316922121));
#27437=CARTESIAN_POINT('',(-0.0150814620157846,0.0393369957695828,0.0845383233588788));
#27438=CARTESIAN_POINT('',(-0.0175,0.0393369957695828,0.0846706150255454));
#27439=CARTESIAN_POINT('',(-0.0199185379842156,0.0393369957695828,0.0848029066922121));
#27440=CARTESIAN_POINT('',(-0.0220130533185638,0.038127726777475,0.0849351983588788));
#27441=CARTESIAN_POINT('',(-0.024107568652912,0.0369184577853673,0.0850674900255454));
#27442=CARTESIAN_POINT('',(-0.0253168376450197,0.0348239424510191,0.0851997816922121));
#27443=CARTESIAN_POINT('',(-0.0265261066371274,0.0327294271166708,0.0853320733588788));
#27444=CARTESIAN_POINT('',(-0.0265261066371274,0.0303108891324553,0.0854643650255454));
#27445=CARTESIAN_POINT('',(-0.0265261066371274,0.0278923511482398,0.0855966566922121));
#27446=CARTESIAN_POINT('',(-0.0253168376450197,0.0257978358138916,0.0857289483588788));
#27447=CARTESIAN_POINT('',(-0.0241075686529119,0.0237033204795434,0.0858612400255455));
#27448=CARTESIAN_POINT('',(-0.0220130533185638,0.0224940514874356,0.0859935316922121));
#27449=CARTESIAN_POINT('',(-0.0199185379842155,0.021284782495328,0.0861258233588788));
#27450=CARTESIAN_POINT('',(-0.0175,0.021284782495328,0.0862581150255454));
#27451=CARTESIAN_POINT('',(-0.0150814620157846,0.021284782495328,0.0863904066922121));
#27452=CARTESIAN_POINT('',(-0.0129869466814363,0.0224940514874357,0.0865226983588788));
#27453=CARTESIAN_POINT('',(-0.0108924313470881,0.0237033204795435,0.0866549900255454));
#27454=CARTESIAN_POINT('',(-0.00968316235498038,0.0257978358138917,0.0867872816922121));
#27455=CARTESIAN_POINT('',(-0.00847389336287265,0.0278923511482399,0.0869195733588788));
#27456=CARTESIAN_POINT('',(-0.00847389336287265,0.0303108891324553,0.0870518650255454));
#27457=CARTESIAN_POINT('',(-0.00847389336287266,0.0327294271166709,0.0871841566922122));
#27458=CARTESIAN_POINT('',(-0.00968316235498039,0.0348239424510191,0.0873164483588788));
#27459=CARTESIAN_POINT('',(-0.0108924313470881,0.0369184577853673,0.0874487400255455));
#27460=CARTESIAN_POINT('',(-0.0129869466814364,0.038127726777475,0.0875810316922121));
#27461=CARTESIAN_POINT('',(-0.0150814620157846,0.0393369957695828,0.0877133233588788));
#27462=CARTESIAN_POINT('',(-0.0175,0.0393369957695828,0.0878456150255454));
#27463=CARTESIAN_POINT('',(-0.0199185379842156,0.0393369957695828,0.0879779066922121));
#27464=CARTESIAN_POINT('',(-0.0220130533185638,0.038127726777475,0.0881101983588788));
#27465=CARTESIAN_POINT('',(-0.024107568652912,0.0369184577853673,0.0882424900255454));
#27466=CARTESIAN_POINT('',(-0.0253168376450197,0.0348239424510191,0.0883747816922121));
#27467=CARTESIAN_POINT('',(-0.0265261066371274,0.0327294271166708,0.0885070733588787));
#27468=CARTESIAN_POINT('',(-0.0265261066371274,0.0303108891324553,0.0886393650255454));
#27469=CARTESIAN_POINT('',(-0.0189864747528493,0.0214080247712546,0.083));
#27470=CARTESIAN_POINT('',(-0.0265261066371274,0.0303108891324553,0.0886393650255454));
#27471=CARTESIAN_POINT('',(-0.0189864747528493,0.0214080247712546,0.083));
#27472=CARTESIAN_POINT('',(-0.0182985666809634,0.0215077465167656,0.083));
#27473=CARTESIAN_POINT('',(-0.0176219168655072,0.0216842616873385,0.083));
#27474=CARTESIAN_POINT('',(-0.0169787305804826,0.0219480257606184,0.083));
#27475=CARTESIAN_POINT('',(-0.0262026,0.0303108891324553,0.0885823220769816));
#27476=CARTESIAN_POINT('',(-0.0236647323997788,0.023433406276125,0.0829642728854406));
#27477=CARTESIAN_POINT('',(-0.0229496504750082,0.0227924321287199,0.0830173387180816));
#27478=CARTESIAN_POINT('',(-0.022118,0.0223122785031023,0.0830686728614772));
#27479=CARTESIAN_POINT('',(-0.0199747787412939,0.0210748891324553,0.0832009645281439));
#27480=CARTESIAN_POINT('',(-0.0175,0.0210748891324553,0.0833332561948105));
#27481=CARTESIAN_POINT('',(-0.0150252212587062,0.0210748891324553,0.0834655478614772));
#27482=CARTESIAN_POINT('',(-0.012882,0.0223122785031023,0.0835978395281439));
#27483=CARTESIAN_POINT('',(-0.0107387787412939,0.0235496678737492,0.0837301311948106));
#27484=CARTESIAN_POINT('',(-0.00950138937064696,0.0256928891324554,0.0838624228614772));
#27485=CARTESIAN_POINT('',(-0.00826400000000004,0.0278361103911615,0.0839947145281439));
#27486=CARTESIAN_POINT('',(-0.008264,0.0303108891324553,0.0841270061948105));
#27487=CARTESIAN_POINT('',(-0.00826400000000004,0.0327856678737492,0.0842592978614772));
#27488=CARTESIAN_POINT('',(-0.00950138937064697,0.0349288891324553,0.0843915895281439));
#27489=CARTESIAN_POINT('',(-0.0107387787412939,0.0370721103911615,0.0845238811948106));
#27490=CARTESIAN_POINT('',(-0.012882,0.0383094997618084,0.0846561728614772));
#27491=CARTESIAN_POINT('',(-0.0150252212587062,0.0395468891324554,0.0847884645281439));
#27492=CARTESIAN_POINT('',(-0.0175,0.0395468891324554,0.0849207561948105));
#27493=CARTESIAN_POINT('',(-0.0199747787412939,0.0395468891324554,0.0850530478614772));
#27494=CARTESIAN_POINT('',(-0.022118,0.0383094997618084,0.0851853395281439));
#27495=CARTESIAN_POINT('',(-0.0242612212587062,0.0370721103911615,0.0853176311948106));
#27496=CARTESIAN_POINT('',(-0.0254986106293531,0.0349288891324553,0.0854499228614772));
#27497=CARTESIAN_POINT('',(-0.0267360000000001,0.0327856678737492,0.0855822145281439));
#27498=CARTESIAN_POINT('',(-0.026736,0.0303108891324553,0.0857145061948105));
#27499=CARTESIAN_POINT('',(-0.0267360000000001,0.0278361103911615,0.0858467978614772));
#27500=CARTESIAN_POINT('',(-0.0254986106293531,0.0256928891324553,0.0859790895281439));
#27501=CARTESIAN_POINT('',(-0.0242612212587062,0.0235496678737492,0.0861113811948106));
#27502=CARTESIAN_POINT('',(-0.022118,0.0223122785031023,0.0862436728614772));
#27503=CARTESIAN_POINT('',(-0.0199747787412939,0.0210748891324553,0.0863759645281439));
#27504=CARTESIAN_POINT('',(-0.0175,0.0210748891324553,0.0865082561948105));
#27505=CARTESIAN_POINT('',(-0.0150252212587062,0.0210748891324553,0.0866405478614773));
#27506=CARTESIAN_POINT('',(-0.012882,0.0223122785031023,0.0867728395281439));
#27507=CARTESIAN_POINT('',(-0.0107387787412939,0.0235496678737492,0.0869051311948106));
#27508=CARTESIAN_POINT('',(-0.00950138937064696,0.0256928891324554,0.0870374228614772));
#27509=CARTESIAN_POINT('',(-0.00826400000000004,0.0278361103911615,0.0871697145281439));
#27510=CARTESIAN_POINT('',(-0.008264,0.0303108891324553,0.0873020061948105));
#27511=CARTESIAN_POINT('',(-0.00826400000000004,0.0327856678737492,0.0874342978614772));
#27512=CARTESIAN_POINT('',(-0.00950138937064697,0.0349288891324553,0.0875665895281439));
#27513=CARTESIAN_POINT('',(-0.0107387787412939,0.0370721103911615,0.0876988811948106));
#27514=CARTESIAN_POINT('',(-0.012882,0.0383094997618084,0.0878311728614772));
#27515=CARTESIAN_POINT('',(-0.0150252212587062,0.0395468891324554,0.0879634645281439));
#27516=CARTESIAN_POINT('',(-0.0175,0.0395468891324554,0.0880957561948105));
#27517=CARTESIAN_POINT('',(-0.0199747787412939,0.0395468891324554,0.0882280478614772));
#27518=CARTESIAN_POINT('',(-0.022118,0.0383094997618084,0.0883603395281439));
#27519=CARTESIAN_POINT('',(-0.0242612212587062,0.0370721103911615,0.0884926311948105));
#27520=CARTESIAN_POINT('',(-0.0254986106293531,0.0349288891324553,0.0886249228614772));
#27521=CARTESIAN_POINT('',(-0.0267360000000001,0.0327856678737492,0.0887572145281438));
#27522=CARTESIAN_POINT('',(-0.026736,0.0303108891324553,0.0888895061948105));
#27523=CARTESIAN_POINT('',(-0.0236647323997788,0.023433406276125,0.0828353137057312));
#27524=CARTESIAN_POINT('',(-0.0229496504750083,0.0227924321287199,0.0828883795383722));
#27525=CARTESIAN_POINT('',(-0.022118,0.0223122785031023,0.0829397136817678));
#27526=CARTESIAN_POINT('',(-0.0199747787412939,0.0210748891324553,0.0830720053484343));
#27527=CARTESIAN_POINT('',(-0.0175,0.0210748891324553,0.083204297015101));
#27528=CARTESIAN_POINT('',(-0.0150252212587062,0.0210748891324553,0.0833365886817677));
#27529=CARTESIAN_POINT('',(-0.012882,0.0223122785031023,0.0834688803484343));
#27530=CARTESIAN_POINT('',(-0.0107387787412939,0.0235496678737492,0.0836011720151011));
#27531=CARTESIAN_POINT('',(-0.00950138937064695,0.0256928891324553,0.0837334636817677));
#27532=CARTESIAN_POINT('',(-0.00826400000000004,0.0278361103911615,0.0838657553484344));
#27533=CARTESIAN_POINT('',(-0.00826400000000004,0.0303108891324553,0.0839980470151011));
#27534=CARTESIAN_POINT('',(-0.00826400000000004,0.0327856678737492,0.0841303386817678));
#27535=CARTESIAN_POINT('',(-0.00950138937064697,0.0349288891324553,0.0842626303484344));
#27536=CARTESIAN_POINT('',(-0.0107387787412939,0.0370721103911615,0.084394922015101));
#27537=CARTESIAN_POINT('',(-0.0128820000000001,0.0383094997618084,0.0845272136817677));
#27538=CARTESIAN_POINT('',(-0.0150252212587062,0.0395468891324554,0.0846595053484344));
#27539=CARTESIAN_POINT('',(-0.0175000000000001,0.0395468891324553,0.084791797015101));
#27540=CARTESIAN_POINT('',(-0.0199747787412939,0.0395468891324554,0.0849240886817677));
#27541=CARTESIAN_POINT('',(-0.0221180000000001,0.0383094997618084,0.0850563803484344));
#27542=CARTESIAN_POINT('',(-0.0242612212587062,0.0370721103911615,0.0851886720151011));
#27543=CARTESIAN_POINT('',(-0.0254986106293532,0.0349288891324553,0.0853209636817677));
#27544=CARTESIAN_POINT('',(-0.0267360000000001,0.0327856678737492,0.0854532553484344));
#27545=CARTESIAN_POINT('',(-0.0267360000000001,0.0303108891324553,0.085585547015101));
#27546=CARTESIAN_POINT('',(-0.0267360000000001,0.0278361103911615,0.0857178386817677));
#27547=CARTESIAN_POINT('',(-0.0254986106293531,0.0256928891324553,0.0858501303484343));
#27548=CARTESIAN_POINT('',(-0.0242612212587062,0.0235496678737492,0.085982422015101));
#27549=CARTESIAN_POINT('',(-0.022118,0.0223122785031023,0.0861147136817677));
#27550=CARTESIAN_POINT('',(-0.0199747787412939,0.0210748891324553,0.0862470053484344));
#27551=CARTESIAN_POINT('',(-0.0175,0.0210748891324553,0.086379297015101));
#27552=CARTESIAN_POINT('',(-0.0150252212587062,0.0210748891324553,0.0865115886817677));
#27553=CARTESIAN_POINT('',(-0.012882,0.0223122785031023,0.0866438803484343));
#27554=CARTESIAN_POINT('',(-0.0107387787412939,0.0235496678737492,0.0867761720151011));
#27555=CARTESIAN_POINT('',(-0.00950138937064695,0.0256928891324553,0.0869084636817677));
#27556=CARTESIAN_POINT('',(-0.00826400000000004,0.0278361103911615,0.0870407553484343));
#27557=CARTESIAN_POINT('',(-0.00826400000000004,0.0303108891324553,0.0871730470151011));
#27558=CARTESIAN_POINT('',(-0.00826400000000004,0.0327856678737492,0.0873053386817677));
#27559=CARTESIAN_POINT('',(-0.00950138937064697,0.0349288891324553,0.0874376303484344));
#27560=CARTESIAN_POINT('',(-0.0107387787412939,0.0370721103911615,0.0875699220151011));
#27561=CARTESIAN_POINT('',(-0.0128820000000001,0.0383094997618084,0.0877022136817677));
#27562=CARTESIAN_POINT('',(-0.0150252212587062,0.0395468891324554,0.0878345053484344));
#27563=CARTESIAN_POINT('',(-0.0175000000000001,0.0395468891324553,0.087966797015101));
#27564=CARTESIAN_POINT('',(-0.0199747787412939,0.0395468891324554,0.0880990886817678));
#27565=CARTESIAN_POINT('',(-0.0221180000000001,0.0383094997618084,0.0882313803484344));
#27566=CARTESIAN_POINT('',(-0.0242612212587062,0.0370721103911615,0.088363672015101));
#27567=CARTESIAN_POINT('',(-0.0254986106293532,0.0349288891324553,0.0884959636817677));
#27568=CARTESIAN_POINT('',(-0.0267360000000001,0.0327856678737492,0.0886282553484344));
#27569=CARTESIAN_POINT('',(-0.0267360000000001,0.0303108891324553,0.088760547015101));
#27570=CARTESIAN_POINT('',(-0.0236094037510318,0.0234951318805056,0.0827365252427255));
#27571=CARTESIAN_POINT('',(-0.0229007397068886,0.0228599104943168,0.0827895910753664));
#27572=CARTESIAN_POINT('',(-0.0220765533185638,0.022384066261155,0.0828409252187621));
#27573=CARTESIAN_POINT('',(-0.0199525675316543,0.0211577824953279,0.0829732168854288));
#27574=CARTESIAN_POINT('',(-0.0175,0.0211577824953279,0.0831055085520954));
#27575=CARTESIAN_POINT('',(-0.0150474324683458,0.0211577824953279,0.0832378002187621));
#27576=CARTESIAN_POINT('',(-0.0129234466814363,0.022384066261155,0.0833700918854287));
#27577=CARTESIAN_POINT('',(-0.0107994608945269,0.0236103500269822,0.0835023835520955));
#27578=CARTESIAN_POINT('',(-0.00957317712869975,0.0257343358138917,0.083634675218762));
#27579=CARTESIAN_POINT('',(-0.00834689336287264,0.0278583216008011,0.0837669668854288));
#27580=CARTESIAN_POINT('',(-0.00834689336287264,0.0303108891324553,0.0838992585520953));
#27581=CARTESIAN_POINT('',(-0.00834689336287265,0.0327634566641096,0.0840315502187621));
#27582=CARTESIAN_POINT('',(-0.00957317712869976,0.034887442451019,0.0841638418854287));
#27583=CARTESIAN_POINT('',(-0.0107994608945269,0.0370114282379285,0.0842961335520954));
#27584=CARTESIAN_POINT('',(-0.0129234466814364,0.0382377120037556,0.084428425218762));
#27585=CARTESIAN_POINT('',(-0.0150474324683458,0.0394639957695827,0.0845607168854288));
#27586=CARTESIAN_POINT('',(-0.0175000000000001,0.0394639957695828,0.0846930085520954));
#27587=CARTESIAN_POINT('',(-0.0199525675316543,0.0394639957695827,0.0848253002187621));
#27588=CARTESIAN_POINT('',(-0.0220765533185638,0.0382377120037556,0.0849575918854288));
#27589=CARTESIAN_POINT('',(-0.0242005391054732,0.0370114282379285,0.0850898835520954));
#27590=CARTESIAN_POINT('',(-0.0254268228713003,0.034887442451019,0.0852221752187621));
#27591=CARTESIAN_POINT('',(-0.0266531066371274,0.0327634566641096,0.0853544668854287));
#27592=CARTESIAN_POINT('',(-0.0266531066371274,0.0303108891324553,0.0854867585520954));
#27593=CARTESIAN_POINT('',(-0.0266531066371274,0.0278583216008011,0.0856190502187621));
#27594=CARTESIAN_POINT('',(-0.0254268228713003,0.0257343358138917,0.0857513418854287));
#27595=CARTESIAN_POINT('',(-0.0242005391054732,0.0236103500269822,0.0858836335520954));
#27596=CARTESIAN_POINT('',(-0.0220765533185638,0.022384066261155,0.0860159252187621));
#27597=CARTESIAN_POINT('',(-0.0199525675316543,0.0211577824953279,0.0861482168854288));
#27598=CARTESIAN_POINT('',(-0.0175,0.0211577824953279,0.0862805085520954));
#27599=CARTESIAN_POINT('',(-0.0150474324683458,0.0211577824953279,0.0864128002187622));
#27600=CARTESIAN_POINT('',(-0.0129234466814363,0.022384066261155,0.0865450918854287));
#27601=CARTESIAN_POINT('',(-0.0107994608945269,0.0236103500269822,0.0866773835520954));
#27602=CARTESIAN_POINT('',(-0.00957317712869975,0.0257343358138917,0.086809675218762));
#27603=CARTESIAN_POINT('',(-0.00834689336287264,0.0278583216008011,0.0869419668854288));
#27604=CARTESIAN_POINT('',(-0.00834689336287264,0.0303108891324553,0.0870742585520954));
#27605=CARTESIAN_POINT('',(-0.00834689336287265,0.0327634566641096,0.0872065502187621));
#27606=CARTESIAN_POINT('',(-0.00957317712869976,0.034887442451019,0.0873388418854287));
#27607=CARTESIAN_POINT('',(-0.0107994608945269,0.0370114282379285,0.0874711335520955));
#27608=CARTESIAN_POINT('',(-0.0129234466814364,0.0382377120037556,0.0876034252187621));
#27609=CARTESIAN_POINT('',(-0.0150474324683458,0.0394639957695827,0.0877357168854287));
#27610=CARTESIAN_POINT('',(-0.0175000000000001,0.0394639957695828,0.0878680085520955));
#27611=CARTESIAN_POINT('',(-0.0199525675316543,0.0394639957695827,0.0880003002187621));
#27612=CARTESIAN_POINT('',(-0.0220765533185638,0.0382377120037556,0.0881325918854288));
#27613=CARTESIAN_POINT('',(-0.0242005391054732,0.0370114282379285,0.0882648835520954));
#27614=CARTESIAN_POINT('',(-0.0254268228713003,0.034887442451019,0.0883971752187621));
#27615=CARTESIAN_POINT('',(-0.0266531066371274,0.0327634566641096,0.0885294668854288));
#27616=CARTESIAN_POINT('',(-0.0266531066371274,0.0303108891324553,0.0886617585520954));
#27617=CARTESIAN_POINT('',(-0.023524635343196,0.0235897009929736,0.0827141317161755));
#27618=CARTESIAN_POINT('',(-0.022825804062635,0.0229632933483092,0.0827671975488165));
#27619=CARTESIAN_POINT('',(-0.0220130533185638,0.0224940514874356,0.0828185316922121));
#27620=CARTESIAN_POINT('',(-0.0199185379842155,0.021284782495328,0.0829508233588788));
#27621=CARTESIAN_POINT('',(-0.0175,0.021284782495328,0.0830831150255454));
#27622=CARTESIAN_POINT('',(-0.0150814620157846,0.021284782495328,0.0832154066922121));
#27623=CARTESIAN_POINT('',(-0.0129869466814363,0.0224940514874357,0.0833476983588788));
#27624=CARTESIAN_POINT('',(-0.0108924313470881,0.0237033204795435,0.0834799900255455));
#27625=CARTESIAN_POINT('',(-0.00968316235498038,0.0257978358138917,0.0836122816922121));
#27626=CARTESIAN_POINT('',(-0.00847389336287265,0.0278923511482399,0.0837445733588788));
#27627=CARTESIAN_POINT('',(-0.00847389336287265,0.0303108891324553,0.0838768650255454));
#27628=CARTESIAN_POINT('',(-0.00847389336287266,0.0327294271166709,0.0840091566922122));
#27629=CARTESIAN_POINT('',(-0.00968316235498039,0.0348239424510191,0.0841414483588788));
#27630=CARTESIAN_POINT('',(-0.0108924313470881,0.0369184577853673,0.0842737400255455));
#27631=CARTESIAN_POINT('',(-0.0129869466814364,0.038127726777475,0.0844060316922121));
#27632=CARTESIAN_POINT('',(-0.0150814620157846,0.0393369957695828,0.0845383233588788));
#27633=CARTESIAN_POINT('',(-0.0175,0.0393369957695828,0.0846706150255454));
#27634=CARTESIAN_POINT('',(-0.0199185379842156,0.0393369957695828,0.0848029066922121));
#27635=CARTESIAN_POINT('',(-0.0220130533185638,0.038127726777475,0.0849351983588788));
#27636=CARTESIAN_POINT('',(-0.024107568652912,0.0369184577853673,0.0850674900255454));
#27637=CARTESIAN_POINT('',(-0.0253168376450197,0.0348239424510191,0.0851997816922121));
#27638=CARTESIAN_POINT('',(-0.0265261066371274,0.0327294271166708,0.0853320733588788));
#27639=CARTESIAN_POINT('',(-0.0265261066371274,0.0303108891324553,0.0854643650255454));
#27640=CARTESIAN_POINT('',(-0.0265261066371274,0.0278923511482398,0.0855966566922121));
#27641=CARTESIAN_POINT('',(-0.0253168376450197,0.0257978358138916,0.0857289483588788));
#27642=CARTESIAN_POINT('',(-0.0241075686529119,0.0237033204795434,0.0858612400255455));
#27643=CARTESIAN_POINT('',(-0.0220130533185638,0.0224940514874356,0.0859935316922121));
#27644=CARTESIAN_POINT('',(-0.0199185379842155,0.021284782495328,0.0861258233588788));
#27645=CARTESIAN_POINT('',(-0.0175,0.021284782495328,0.0862581150255454));
#27646=CARTESIAN_POINT('',(-0.0150814620157846,0.021284782495328,0.0863904066922121));
#27647=CARTESIAN_POINT('',(-0.0129869466814363,0.0224940514874357,0.0865226983588788));
#27648=CARTESIAN_POINT('',(-0.0108924313470881,0.0237033204795435,0.0866549900255455));
#27649=CARTESIAN_POINT('',(-0.00968316235498038,0.0257978358138917,0.0867872816922121));
#27650=CARTESIAN_POINT('',(-0.00847389336287265,0.0278923511482399,0.0869195733588788));
#27651=CARTESIAN_POINT('',(-0.00847389336287265,0.0303108891324553,0.0870518650255454));
#27652=CARTESIAN_POINT('',(-0.00847389336287266,0.0327294271166709,0.0871841566922122));
#27653=CARTESIAN_POINT('',(-0.00968316235498039,0.0348239424510191,0.0873164483588788));
#27654=CARTESIAN_POINT('',(-0.0108924313470881,0.0369184577853673,0.0874487400255455));
#27655=CARTESIAN_POINT('',(-0.0129869466814364,0.038127726777475,0.0875810316922121));
#27656=CARTESIAN_POINT('',(-0.0150814620157846,0.0393369957695828,0.0877133233588788));
#27657=CARTESIAN_POINT('',(-0.0175,0.0393369957695828,0.0878456150255454));
#27658=CARTESIAN_POINT('',(-0.0199185379842156,0.0393369957695828,0.0879779066922121));
#27659=CARTESIAN_POINT('',(-0.0220130533185638,0.038127726777475,0.0881101983588788));
#27660=CARTESIAN_POINT('',(-0.024107568652912,0.0369184577853673,0.0882424900255454));
#27661=CARTESIAN_POINT('',(-0.0253168376450197,0.0348239424510191,0.0883747816922121));
#27662=CARTESIAN_POINT('',(-0.0265261066371274,0.0327294271166708,0.0885070733588787));
#27663=CARTESIAN_POINT('',(-0.0265261066371274,0.0303108891324553,0.0886393650255454));
#27664=CARTESIAN_POINT('',(-0.0231671894155392,0.0230179706406304,0.083));
#27665=CARTESIAN_POINT('',(-0.0226668043442114,0.0226291308389651,0.0830347975716187));
#27666=CARTESIAN_POINT('',(-0.022118,0.0223122785031023,0.0830686728614772));
#27667=CARTESIAN_POINT('',(-0.0199747787412939,0.0210748891324553,0.0832009645281439));
#27668=CARTESIAN_POINT('',(-0.0175,0.0210748891324553,0.0833332561948105));
#27669=CARTESIAN_POINT('',(-0.0150252212587062,0.0210748891324553,0.0834655478614772));
#27670=CARTESIAN_POINT('',(-0.012882,0.0223122785031023,0.0835978395281439));
#27671=CARTESIAN_POINT('',(-0.0107387787412939,0.0235496678737492,0.0837301311948106));
#27672=CARTESIAN_POINT('',(-0.00950138937064696,0.0256928891324554,0.0838624228614772));
#27673=CARTESIAN_POINT('',(-0.00826400000000004,0.0278361103911615,0.0839947145281439));
#27674=CARTESIAN_POINT('',(-0.008264,0.0303108891324553,0.0841270061948105));
#27675=CARTESIAN_POINT('',(-0.00826400000000005,0.0327856678737492,0.0842592978614772));
#27676=CARTESIAN_POINT('',(-0.00950138937064697,0.0349288891324553,0.0843915895281439));
#27677=CARTESIAN_POINT('',(-0.0107387787412939,0.0370721103911615,0.0845238811948106));
#27678=CARTESIAN_POINT('',(-0.012882,0.0383094997618084,0.0846561728614772));
#27679=CARTESIAN_POINT('',(-0.0150252212587062,0.0395468891324554,0.0847884645281439));
#27680=CARTESIAN_POINT('',(-0.0175,0.0395468891324554,0.0849207561948105));
#27681=CARTESIAN_POINT('',(-0.0199747787412939,0.0395468891324554,0.0850530478614772));
#27682=CARTESIAN_POINT('',(-0.022118,0.0383094997618084,0.0851853395281439));
#27683=CARTESIAN_POINT('',(-0.0242612212587062,0.0370721103911615,0.0853176311948106));
#27684=CARTESIAN_POINT('',(-0.0254986106293531,0.0349288891324553,0.0854499228614772));
#27685=CARTESIAN_POINT('',(-0.0267360000000001,0.0327856678737492,0.0855822145281439));
#27686=CARTESIAN_POINT('',(-0.026736,0.0303108891324553,0.0857145061948105));
#27687=CARTESIAN_POINT('',(-0.0267360000000001,0.0278361103911615,0.0858467978614772));
#27688=CARTESIAN_POINT('',(-0.0254986106293531,0.0256928891324554,0.0859790895281439));
#27689=CARTESIAN_POINT('',(-0.0242612212587062,0.0235496678737492,0.0861113811948106));
#27690=CARTESIAN_POINT('',(-0.022118,0.0223122785031023,0.0862436728614772));
#27691=CARTESIAN_POINT('',(-0.0199747787412939,0.0210748891324553,0.0863759645281439));
#27692=CARTESIAN_POINT('',(-0.0175,0.0210748891324553,0.0865082561948105));
#27693=CARTESIAN_POINT('',(-0.0150252212587062,0.0210748891324553,0.0866405478614773));
#27694=CARTESIAN_POINT('',(-0.012882,0.0223122785031023,0.0867728395281439));
#27695=CARTESIAN_POINT('',(-0.0107387787412939,0.0235496678737492,0.0869051311948106));
#27696=CARTESIAN_POINT('',(-0.00950138937064696,0.0256928891324554,0.0870374228614772));
#27697=CARTESIAN_POINT('',(-0.00826400000000004,0.0278361103911615,0.0871697145281439));
#27698=CARTESIAN_POINT('',(-0.008264,0.0303108891324553,0.0873020061948105));
#27699=CARTESIAN_POINT('',(-0.00826400000000005,0.0327856678737492,0.0874342978614772));
#27700=CARTESIAN_POINT('',(-0.00950138937064697,0.0349288891324553,0.0875665895281439));
#27701=CARTESIAN_POINT('',(-0.0107387787412939,0.0370721103911615,0.0876988811948106));
#27702=CARTESIAN_POINT('',(-0.012882,0.0383094997618084,0.0878311728614772));
#27703=CARTESIAN_POINT('',(-0.0150252212587062,0.0395468891324554,0.0879634645281439));
#27704=CARTESIAN_POINT('',(-0.0175,0.0395468891324554,0.0880957561948105));
#27705=CARTESIAN_POINT('',(-0.0199747787412939,0.0395468891324554,0.0882280478614772));
#27706=CARTESIAN_POINT('',(-0.022118,0.0383094997618084,0.0883603395281439));
#27707=CARTESIAN_POINT('',(-0.0242612212587062,0.0370721103911615,0.0884926311948105));
#27708=CARTESIAN_POINT('',(-0.0254986106293531,0.0349288891324553,0.0886249228614772));
#27709=CARTESIAN_POINT('',(-0.0267360000000001,0.0327856678737492,0.0887572145281438));
#27710=CARTESIAN_POINT('',(-0.026736,0.0303108891324553,0.0888895061948105));
#27711=CARTESIAN_POINT('',(-0.0231671894155392,0.0230179706406305,0.083));
#27712=CARTESIAN_POINT('',(-0.026736,0.0303108891324553,0.0888895061948106));
#27713=CARTESIAN_POINT('',(-0.0231671894155392,0.0230179706406305,0.083));
#27714=CARTESIAN_POINT('',(-0.022866367542065,0.0227842076362548,0.083));
#27715=CARTESIAN_POINT('',(-0.022233243984053,0.0223583930718137,0.0830000000000008));
#27716=CARTESIAN_POINT('',(-0.0212143894591252,0.021861314846878,0.0829999999999974));
#27717=CARTESIAN_POINT('',(-0.0203050731606182,0.0215625176281714,0.0830000000000078));
#27718=CARTESIAN_POINT('',(-0.0195554495157663,0.021430163182606,0.0829999999999866));
#27719=CARTESIAN_POINT('',(-0.0191798302521447,0.0213799952297573,0.0830000000000297));
#27720=CARTESIAN_POINT('',(-0.0189864747528848,0.0214080247710879,0.0830000000000297));
#27721=CARTESIAN_POINT('',(-0.026482,0.0303108891324553,0.0888895061948105));
#27722=CARTESIAN_POINT('',(-0.0175,0.0303108891324553,0.0828194520637169));
#27723=CARTESIAN_POINT('',(-0.0265148517458493,0.0283018734529848,0.083));
#27724=CARTESIAN_POINT('',(-0.0262067727498258,0.0269194619051097,0.0830783108961613));
#27725=CARTESIAN_POINT('',(-0.0254986106293531,0.0256928891324554,0.0831540218642768));
#27726=CARTESIAN_POINT('',(-0.0242612212587062,0.0235496678737492,0.0832863135309434));
#27727=CARTESIAN_POINT('',(-0.022118,0.0223122785031023,0.0834186051976101));
#27728=CARTESIAN_POINT('',(-0.0199747787412939,0.0210748891324553,0.0835508968642768));
#27729=CARTESIAN_POINT('',(-0.0175,0.0210748891324553,0.0836831885309434));
#27730=CARTESIAN_POINT('',(-0.0150252212587062,0.0210748891324553,0.0838154801976102));
#27731=CARTESIAN_POINT('',(-0.012882,0.0223122785031023,0.0839477718642768));
#27732=CARTESIAN_POINT('',(-0.0107387787412939,0.0235496678737492,0.0840800635309435));
#27733=CARTESIAN_POINT('',(-0.00950138937064697,0.0256928891324554,0.0842123551976101));
#27734=CARTESIAN_POINT('',(-0.00826400000000004,0.0278361103911615,0.0843446468642768));
#27735=CARTESIAN_POINT('',(-0.008264,0.0303108891324553,0.0844769385309434));
#27736=CARTESIAN_POINT('',(-0.00826400000000005,0.0327856678737492,0.0846092301976101));
#27737=CARTESIAN_POINT('',(-0.00950138937064697,0.0349288891324553,0.0847415218642768));
#27738=CARTESIAN_POINT('',(-0.0107387787412939,0.0370721103911615,0.0848738135309434));
#27739=CARTESIAN_POINT('',(-0.012882,0.0383094997618084,0.0850061051976101));
#27740=CARTESIAN_POINT('',(-0.0150252212587062,0.0395468891324554,0.0851383968642767));
#27741=CARTESIAN_POINT('',(-0.0175,0.0395468891324554,0.0852706885309434));
#27742=CARTESIAN_POINT('',(-0.0199747787412939,0.0395468891324554,0.0854029801976102));
#27743=CARTESIAN_POINT('',(-0.022118,0.0383094997618084,0.0855352718642768));
#27744=CARTESIAN_POINT('',(-0.0242612212587062,0.0370721103911615,0.0856675635309435));
#27745=CARTESIAN_POINT('',(-0.0254986106293531,0.0349288891324553,0.0857998551976101));
#27746=CARTESIAN_POINT('',(-0.0267360000000001,0.0327856678737492,0.0859321468642768));
#27747=CARTESIAN_POINT('',(-0.026736,0.0303108891324553,0.0860644385309434));
#27748=CARTESIAN_POINT('',(-0.0267360000000001,0.0278361103911615,0.0861967301976101));
#27749=CARTESIAN_POINT('',(-0.0254986106293531,0.0256928891324554,0.0863290218642768));
#27750=CARTESIAN_POINT('',(-0.0242612212587062,0.0235496678737492,0.0864613135309434));
#27751=CARTESIAN_POINT('',(-0.022118,0.0223122785031023,0.0865936051976101));
#27752=CARTESIAN_POINT('',(-0.0199747787412939,0.0210748891324553,0.0867258968642769));
#27753=CARTESIAN_POINT('',(-0.0175,0.0210748891324553,0.0868581885309434));
#27754=CARTESIAN_POINT('',(-0.0150252212587062,0.0210748891324553,0.0869904801976102));
#27755=CARTESIAN_POINT('',(-0.012882,0.0223122785031023,0.0871227718642768));
#27756=CARTESIAN_POINT('',(-0.0107387787412939,0.0235496678737492,0.0872550635309435));
#27757=CARTESIAN_POINT('',(-0.00950138937064697,0.0256928891324554,0.0873873551976101));
#27758=CARTESIAN_POINT('',(-0.00826400000000004,0.0278361103911615,0.0875196468642768));
#27759=CARTESIAN_POINT('',(-0.008264,0.0303108891324553,0.0876519385309434));
#27760=CARTESIAN_POINT('',(-0.00826400000000005,0.0327856678737492,0.0877842301976101));
#27761=CARTESIAN_POINT('',(-0.00950138937064697,0.0349288891324553,0.0879165218642768));
#27762=CARTESIAN_POINT('',(-0.0107387787412939,0.0370721103911615,0.0880488135309434));
#27763=CARTESIAN_POINT('',(-0.012882,0.0383094997618084,0.0881811051976101));
#27764=CARTESIAN_POINT('',(-0.0150252212587062,0.0395468891324554,0.0883133968642768));
#27765=CARTESIAN_POINT('',(-0.0175,0.0395468891324554,0.0884456885309434));
#27766=CARTESIAN_POINT('',(-0.0199747787412939,0.0395468891324554,0.0885779801976102));
#27767=CARTESIAN_POINT('',(-0.022118,0.0383094997618084,0.0887102718642768));
#27768=CARTESIAN_POINT('',(-0.0242612212587062,0.0370721103911615,0.0888425635309435));
#27769=CARTESIAN_POINT('',(-0.0254986106293531,0.0349288891324553,0.0889748551976101));
#27770=CARTESIAN_POINT('',(-0.0267360000000001,0.0327856678737492,0.0891071468642768));
#27771=CARTESIAN_POINT('',(-0.026736,0.0303108891324553,0.0892394385309434));
#27772=CARTESIAN_POINT('',(-0.0265148517458494,0.0283018734529848,0.083));
#27773=CARTESIAN_POINT('',(-0.026736,0.0303108891324553,0.0892394385309435));
#27774=CARTESIAN_POINT('',(-0.0175,0.0303108891324553,0.083));
#27775=CARTESIAN_POINT('',(-0.026736,0.0303108891324553,0.089064472362877));
#27776=CARTESIAN_POINT('',(-0.0229058748693024,0.0375225018329433,0.082958966074661));
#27777=CARTESIAN_POINT('',(-0.0243825679779275,0.0364155624426667,0.0830625736532481));
#27778=CARTESIAN_POINT('',(-0.0253053270676696,0.0348172968160874,0.0831636705648742));
#27779=CARTESIAN_POINT('',(-0.0265128153672642,0.0327258657316446,0.083295962231541));
#27780=CARTESIAN_POINT('',(-0.0265128153672642,0.0303108891324553,0.0834282538982076));
#27781=CARTESIAN_POINT('',(-0.0265128153672642,0.0278959125332661,0.0835605455648743));
#27782=CARTESIAN_POINT('',(-0.0253053270676696,0.0258044814488233,0.0836928372315409));
#27783=CARTESIAN_POINT('',(-0.024097838768075,0.0237130503643804,0.0838251288982076));
#27784=CARTESIAN_POINT('',(-0.0220064076836321,0.0225055620647858,0.0839574205648743));
#27785=CARTESIAN_POINT('',(-0.0199149765991893,0.0212980737651912,0.0840897122315409));
#27786=CARTESIAN_POINT('',(-0.0175,0.0212980737651912,0.0842220038982076));
#27787=CARTESIAN_POINT('',(-0.0150850234008108,0.0212980737651912,0.0843542955648742));
#27788=CARTESIAN_POINT('',(-0.012993592316368,0.0225055620647858,0.0844865872315409));
#27789=CARTESIAN_POINT('',(-0.0109021612319251,0.0237130503643804,0.0846188788982076));
#27790=CARTESIAN_POINT('',(-0.00969467293233052,0.0258044814488233,0.0847511705648743));
#27791=CARTESIAN_POINT('',(-0.0084871846327359,0.0278959125332661,0.084883462231541));
#27792=CARTESIAN_POINT('',(-0.0084871846327359,0.0303108891324553,0.0850157538982076));
#27793=CARTESIAN_POINT('',(-0.0084871846327359,0.0327258657316446,0.0851480455648743));
#27794=CARTESIAN_POINT('',(-0.00969467293233052,0.0348172968160874,0.0852803372315409));
#27795=CARTESIAN_POINT('',(-0.0109021612319251,0.0369087279005303,0.0854126288982076));
#27796=CARTESIAN_POINT('',(-0.012993592316368,0.0381162162001248,0.0855449205648742));
#27797=CARTESIAN_POINT('',(-0.0150850234008108,0.0393237044997195,0.0856772122315409));
#27798=CARTESIAN_POINT('',(-0.0175,0.0393237044997195,0.0858095038982076));
#27799=CARTESIAN_POINT('',(-0.0199149765991893,0.0393237044997195,0.0859417955648742));
#27800=CARTESIAN_POINT('',(-0.0220064076836321,0.0381162162001248,0.0860740872315409));
#27801=CARTESIAN_POINT('',(-0.024097838768075,0.0369087279005302,0.0862063788982076));
#27802=CARTESIAN_POINT('',(-0.0253053270676696,0.0348172968160874,0.0863386705648743));
#27803=CARTESIAN_POINT('',(-0.0265128153672642,0.0327258657316446,0.086470962231541));
#27804=CARTESIAN_POINT('',(-0.0265128153672642,0.0303108891324553,0.0866032538982076));
#27805=CARTESIAN_POINT('',(-0.0265128153672642,0.0278959125332661,0.0867355455648743));
#27806=CARTESIAN_POINT('',(-0.0253053270676696,0.0258044814488233,0.0868678372315409));
#27807=CARTESIAN_POINT('',(-0.024097838768075,0.0237130503643804,0.0870001288982076));
#27808=CARTESIAN_POINT('',(-0.0220064076836321,0.0225055620647858,0.0871324205648743));
#27809=CARTESIAN_POINT('',(-0.0199149765991893,0.0212980737651912,0.0872647122315409));
#27810=CARTESIAN_POINT('',(-0.0175,0.0212980737651912,0.0873970038982076));
#27811=CARTESIAN_POINT('',(-0.0150850234008108,0.0212980737651912,0.0875292955648742));
#27812=CARTESIAN_POINT('',(-0.012993592316368,0.0225055620647858,0.0876615872315409));
#27813=CARTESIAN_POINT('',(-0.0109021612319251,0.0237130503643804,0.0877938788982077));
#27814=CARTESIAN_POINT('',(-0.00969467293233052,0.0258044814488233,0.0879261705648742));
#27815=CARTESIAN_POINT('',(-0.0084871846327359,0.0278959125332661,0.088058462231541));
#27816=CARTESIAN_POINT('',(-0.0084871846327359,0.0303108891324553,0.0881907538982076));
#27817=CARTESIAN_POINT('',(-0.0084871846327359,0.0327258657316446,0.0883230455648743));
#27818=CARTESIAN_POINT('',(-0.00969467293233052,0.0348172968160874,0.0884553372315409));
#27819=CARTESIAN_POINT('',(-0.0109021612319251,0.0369087279005303,0.0885876288982076));
#27820=CARTESIAN_POINT('',(-0.012993592316368,0.0381162162001248,0.0887199205648743));
#27821=CARTESIAN_POINT('',(-0.0150850234008108,0.0393237044997195,0.0888522122315409));
#27822=CARTESIAN_POINT('',(-0.0175,0.0393237044997195,0.0889845038982076));
#27823=CARTESIAN_POINT('',(-0.0199149765991893,0.0393237044997195,0.0891167955648742));
#27824=CARTESIAN_POINT('',(-0.0220064076836321,0.0381162162001248,0.0892490872315409));
#27825=CARTESIAN_POINT('',(-0.024097838768075,0.0369087279005302,0.0893813788982077));
#27826=CARTESIAN_POINT('',(-0.0253053270676696,0.0348172968160874,0.0895136705648743));
#27827=CARTESIAN_POINT('',(-0.0265128153672642,0.0327258657316446,0.0896459622315409));
#27828=CARTESIAN_POINT('',(-0.0265128153672642,0.0303108891324553,0.0897782538982076));
#27829=CARTESIAN_POINT('',(-0.0229927332845268,0.0376383737806892,0.0828141534627457));
#27830=CARTESIAN_POINT('',(-0.0244931530287639,0.0365136487398911,0.0829177610413327));
#27831=CARTESIAN_POINT('',(-0.0254307384683766,0.0348897031220451,0.0830188579529589));
#27832=CARTESIAN_POINT('',(-0.0266576279791795,0.0327646681540611,0.0831511496196256));
#27833=CARTESIAN_POINT('',(-0.0266576279791795,0.0303108891324553,0.0832834412862923));
#27834=CARTESIAN_POINT('',(-0.0266576279791795,0.0278571101108495,0.0834157329529589));
#27835=CARTESIAN_POINT('',(-0.0254307384683766,0.0257320751428656,0.0835480246196256));
#27836=CARTESIAN_POINT('',(-0.0242038489575737,0.0236070401748817,0.0836803162862922));
#27837=CARTESIAN_POINT('',(-0.0220788139895898,0.0223801506640788,0.0838126079529589));
#27838=CARTESIAN_POINT('',(-0.0199537790216058,0.0211532611532759,0.0839448996196255));
#27839=CARTESIAN_POINT('',(-0.0175000000000001,0.0211532611532759,0.0840771912862923));
#27840=CARTESIAN_POINT('',(-0.0150462209783943,0.0211532611532759,0.0842094829529589));
#27841=CARTESIAN_POINT('',(-0.0129211860104103,0.0223801506640788,0.0843417746196256));
#27842=CARTESIAN_POINT('',(-0.0107961510424264,0.0236070401748817,0.0844740662862923));
#27843=CARTESIAN_POINT('',(-0.00956926153162349,0.0257320751428656,0.0846063579529589));
#27844=CARTESIAN_POINT('',(-0.00834237202082059,0.0278571101108495,0.0847386496196256));
#27845=CARTESIAN_POINT('',(-0.00834237202082059,0.0303108891324554,0.0848709412862923));
#27846=CARTESIAN_POINT('',(-0.00834237202082059,0.0327646681540611,0.0850032329529589));
#27847=CARTESIAN_POINT('',(-0.00956926153162349,0.0348897031220451,0.0851355246196256));
#27848=CARTESIAN_POINT('',(-0.0107961510424264,0.037014738090029,0.0852678162862922));
#27849=CARTESIAN_POINT('',(-0.0129211860104103,0.0382416276008319,0.085400107952959));
#27850=CARTESIAN_POINT('',(-0.0150462209783943,0.0394685171116348,0.0855323996196256));
#27851=CARTESIAN_POINT('',(-0.0175000000000001,0.0394685171116348,0.0856646912862923));
#27852=CARTESIAN_POINT('',(-0.0199537790216058,0.0394685171116348,0.0857969829529589));
#27853=CARTESIAN_POINT('',(-0.0220788139895898,0.0382416276008319,0.0859292746196256));
#27854=CARTESIAN_POINT('',(-0.0242038489575737,0.037014738090029,0.0860615662862922));
#27855=CARTESIAN_POINT('',(-0.0254307384683766,0.0348897031220451,0.086193857952959));
#27856=CARTESIAN_POINT('',(-0.0266576279791795,0.0327646681540611,0.0863261496196256));
#27857=CARTESIAN_POINT('',(-0.0266576279791795,0.0303108891324553,0.0864584412862923));
#27858=CARTESIAN_POINT('',(-0.0266576279791795,0.0278571101108495,0.0865907329529589));
#27859=CARTESIAN_POINT('',(-0.0254307384683766,0.0257320751428656,0.0867230246196256));
#27860=CARTESIAN_POINT('',(-0.0242038489575737,0.0236070401748817,0.0868553162862923));
#27861=CARTESIAN_POINT('',(-0.0220788139895898,0.0223801506640788,0.086987607952959));
#27862=CARTESIAN_POINT('',(-0.0199537790216058,0.0211532611532759,0.0871198996196256));
#27863=CARTESIAN_POINT('',(-0.0175000000000001,0.0211532611532759,0.0872521912862922));
#27864=CARTESIAN_POINT('',(-0.0150462209783943,0.0211532611532759,0.0873844829529589));
#27865=CARTESIAN_POINT('',(-0.0129211860104103,0.0223801506640788,0.0875167746196255));
#27866=CARTESIAN_POINT('',(-0.0107961510424264,0.0236070401748817,0.0876490662862923));
#27867=CARTESIAN_POINT('',(-0.00956926153162349,0.0257320751428656,0.087781357952959));
#27868=CARTESIAN_POINT('',(-0.00834237202082059,0.0278571101108495,0.0879136496196256));
#27869=CARTESIAN_POINT('',(-0.00834237202082059,0.0303108891324554,0.0880459412862923));
#27870=CARTESIAN_POINT('',(-0.00834237202082059,0.0327646681540611,0.0881782329529589));
#27871=CARTESIAN_POINT('',(-0.00956926153162349,0.0348897031220451,0.0883105246196256));
#27872=CARTESIAN_POINT('',(-0.0107961510424264,0.037014738090029,0.0884428162862923));
#27873=CARTESIAN_POINT('',(-0.0129211860104103,0.0382416276008319,0.0885751079529589));
#27874=CARTESIAN_POINT('',(-0.0150462209783943,0.0394685171116348,0.0887073996196256));
#27875=CARTESIAN_POINT('',(-0.0175000000000001,0.0394685171116348,0.0888396912862922));
#27876=CARTESIAN_POINT('',(-0.0199537790216058,0.0394685171116348,0.0889719829529589));
#27877=CARTESIAN_POINT('',(-0.0220788139895898,0.0382416276008319,0.0891042746196256));
#27878=CARTESIAN_POINT('',(-0.0242038489575737,0.037014738090029,0.0892365662862923));
#27879=CARTESIAN_POINT('',(-0.0254307384683766,0.0348897031220451,0.0893688579529589));
#27880=CARTESIAN_POINT('',(-0.0266576279791795,0.0327646681540611,0.0895011496196256));
#27881=CARTESIAN_POINT('',(-0.0266576279791795,0.0303108891324553,0.0896334412862922));
#27882=CARTESIAN_POINT('',(-0.0230397407201111,0.0377010832269256,0.0826249466671701));
#27883=CARTESIAN_POINT('',(-0.024553001227011,0.0365667326614266,0.0827285542457571));
#27884=CARTESIAN_POINT('',(-0.0254986106293531,0.0349288891324553,0.0828296511573834));
#27885=CARTESIAN_POINT('',(-0.026736,0.0327856678737492,0.08296194282405));
#27886=CARTESIAN_POINT('',(-0.026736,0.0303108891324553,0.0830942344907168));
#27887=CARTESIAN_POINT('',(-0.026736,0.0278361103911615,0.0832265261573834));
#27888=CARTESIAN_POINT('',(-0.0254986106293531,0.0256928891324553,0.08335881782405));
#27889=CARTESIAN_POINT('',(-0.0242612212587062,0.0235496678737492,0.0834911094907167));
#27890=CARTESIAN_POINT('',(-0.022118,0.0223122785031022,0.0836234011573834));
#27891=CARTESIAN_POINT('',(-0.0199747787412939,0.0210748891324553,0.08375569282405));
#27892=CARTESIAN_POINT('',(-0.0175,0.0210748891324553,0.0838879844907167));
#27893=CARTESIAN_POINT('',(-0.0150252212587062,0.0210748891324554,0.0840202761573834));
#27894=CARTESIAN_POINT('',(-0.012882,0.0223122785031022,0.08415256782405));
#27895=CARTESIAN_POINT('',(-0.0107387787412939,0.0235496678737492,0.0842848594907167));
#27896=CARTESIAN_POINT('',(-0.00950138937064696,0.0256928891324553,0.0844171511573834));
#27897=CARTESIAN_POINT('',(-0.00826400000000005,0.0278361103911615,0.08454944282405));
#27898=CARTESIAN_POINT('',(-0.00826400000000005,0.0303108891324554,0.0846817344907167));
#27899=CARTESIAN_POINT('',(-0.00826400000000005,0.0327856678737492,0.0848140261573834));
#27900=CARTESIAN_POINT('',(-0.00950138937064697,0.0349288891324553,0.0849463178240501));
#27901=CARTESIAN_POINT('',(-0.0107387787412939,0.0370721103911615,0.0850786094907167));
#27902=CARTESIAN_POINT('',(-0.0128820000000001,0.0383094997618084,0.0852109011573834));
#27903=CARTESIAN_POINT('',(-0.0150252212587062,0.0395468891324554,0.08534319282405));
#27904=CARTESIAN_POINT('',(-0.0175000000000001,0.0395468891324553,0.0854754844907167));
#27905=CARTESIAN_POINT('',(-0.0199747787412939,0.0395468891324554,0.0856077761573834));
#27906=CARTESIAN_POINT('',(-0.022118,0.0383094997618084,0.0857400678240501));
#27907=CARTESIAN_POINT('',(-0.0242612212587062,0.0370721103911614,0.0858723594907167));
#27908=CARTESIAN_POINT('',(-0.0254986106293531,0.0349288891324553,0.0860046511573834));
#27909=CARTESIAN_POINT('',(-0.026736,0.0327856678737492,0.08613694282405));
#27910=CARTESIAN_POINT('',(-0.026736,0.0303108891324553,0.0862692344907167));
#27911=CARTESIAN_POINT('',(-0.026736,0.0278361103911615,0.0864015261573834));
#27912=CARTESIAN_POINT('',(-0.0254986106293531,0.0256928891324553,0.0865338178240501));
#27913=CARTESIAN_POINT('',(-0.0242612212587062,0.0235496678737492,0.0866661094907167));
#27914=CARTESIAN_POINT('',(-0.022118,0.0223122785031022,0.0867984011573834));
#27915=CARTESIAN_POINT('',(-0.0199747787412939,0.0210748891324553,0.0869306928240501));
#27916=CARTESIAN_POINT('',(-0.0175,0.0210748891324553,0.0870629844907167));
#27917=CARTESIAN_POINT('',(-0.0150252212587062,0.0210748891324554,0.0871952761573834));
#27918=CARTESIAN_POINT('',(-0.012882,0.0223122785031022,0.0873275678240501));
#27919=CARTESIAN_POINT('',(-0.0107387787412939,0.0235496678737492,0.0874598594907167));
#27920=CARTESIAN_POINT('',(-0.00950138937064696,0.0256928891324553,0.0875921511573834));
#27921=CARTESIAN_POINT('',(-0.00826400000000005,0.0278361103911615,0.0877244428240501));
#27922=CARTESIAN_POINT('',(-0.00826400000000005,0.0303108891324554,0.0878567344907168));
#27923=CARTESIAN_POINT('',(-0.00826400000000005,0.0327856678737492,0.0879890261573834));
#27924=CARTESIAN_POINT('',(-0.00950138937064697,0.0349288891324553,0.0881213178240501));
#27925=CARTESIAN_POINT('',(-0.0107387787412939,0.0370721103911615,0.0882536094907168));
#27926=CARTESIAN_POINT('',(-0.0128820000000001,0.0383094997618084,0.0883859011573834));
#27927=CARTESIAN_POINT('',(-0.0150252212587062,0.0395468891324554,0.0885181928240501));
#27928=CARTESIAN_POINT('',(-0.0175000000000001,0.0395468891324553,0.0886504844907168));
#27929=CARTESIAN_POINT('',(-0.0199747787412939,0.0395468891324554,0.0887827761573834));
#27930=CARTESIAN_POINT('',(-0.022118,0.0383094997618084,0.0889150678240501));
#27931=CARTESIAN_POINT('',(-0.0242612212587062,0.0370721103911614,0.0890473594907168));
#27932=CARTESIAN_POINT('',(-0.0254986106293531,0.0349288891324553,0.0891796511573834));
#27933=CARTESIAN_POINT('',(-0.026736,0.0327856678737492,0.0893119428240501));
#27934=CARTESIAN_POINT('',(-0.026736,0.0303108891324553,0.0894442344907167));
#27935=CARTESIAN_POINT('',(-0.0230397407201111,0.0377010832269256,0.0824201507073969));
#27936=CARTESIAN_POINT('',(-0.0245530012270111,0.0365667326614266,0.0825237582859839));
#27937=CARTESIAN_POINT('',(-0.0254986106293531,0.0349288891324553,0.0826248551976101));
#27938=CARTESIAN_POINT('',(-0.0267360000000001,0.0327856678737492,0.0827571468642768));
#27939=CARTESIAN_POINT('',(-0.026736,0.0303108891324553,0.0828894385309434));
#27940=CARTESIAN_POINT('',(-0.0267360000000001,0.0278361103911615,0.0830217301976101));
#27941=CARTESIAN_POINT('',(-0.0254986106293531,0.0256928891324554,0.0831540218642768));
#27942=CARTESIAN_POINT('',(-0.0242612212587062,0.0235496678737492,0.0832863135309434));
#27943=CARTESIAN_POINT('',(-0.022118,0.0223122785031023,0.0834186051976101));
#27944=CARTESIAN_POINT('',(-0.0199747787412939,0.0210748891324553,0.0835508968642768));
#27945=CARTESIAN_POINT('',(-0.0175,0.0210748891324553,0.0836831885309434));
#27946=CARTESIAN_POINT('',(-0.0150252212587062,0.0210748891324554,0.0838154801976102));
#27947=CARTESIAN_POINT('',(-0.012882,0.0223122785031023,0.0839477718642768));
#27948=CARTESIAN_POINT('',(-0.0107387787412939,0.0235496678737492,0.0840800635309435));
#27949=CARTESIAN_POINT('',(-0.00950138937064697,0.0256928891324554,0.0842123551976101));
#27950=CARTESIAN_POINT('',(-0.00826400000000004,0.0278361103911615,0.0843446468642768));
#27951=CARTESIAN_POINT('',(-0.008264,0.0303108891324553,0.0844769385309434));
#27952=CARTESIAN_POINT('',(-0.00826400000000005,0.0327856678737492,0.0846092301976101));
#27953=CARTESIAN_POINT('',(-0.00950138937064697,0.0349288891324553,0.0847415218642768));
#27954=CARTESIAN_POINT('',(-0.0107387787412939,0.0370721103911615,0.0848738135309434));
#27955=CARTESIAN_POINT('',(-0.012882,0.0383094997618084,0.0850061051976101));
#27956=CARTESIAN_POINT('',(-0.0150252212587062,0.0395468891324554,0.0851383968642767));
#27957=CARTESIAN_POINT('',(-0.0175,0.0395468891324554,0.0852706885309434));
#27958=CARTESIAN_POINT('',(-0.0199747787412939,0.0395468891324554,0.0854029801976102));
#27959=CARTESIAN_POINT('',(-0.022118,0.0383094997618084,0.0855352718642768));
#27960=CARTESIAN_POINT('',(-0.0242612212587062,0.0370721103911615,0.0856675635309435));
#27961=CARTESIAN_POINT('',(-0.0254986106293531,0.0349288891324553,0.0857998551976101));
#27962=CARTESIAN_POINT('',(-0.0267360000000001,0.0327856678737492,0.0859321468642768));
#27963=CARTESIAN_POINT('',(-0.026736,0.0303108891324553,0.0860644385309434));
#27964=CARTESIAN_POINT('',(-0.0267360000000001,0.0278361103911615,0.0861967301976101));
#27965=CARTESIAN_POINT('',(-0.0254986106293531,0.0256928891324554,0.0863290218642768));
#27966=CARTESIAN_POINT('',(-0.0242612212587062,0.0235496678737492,0.0864613135309434));
#27967=CARTESIAN_POINT('',(-0.022118,0.0223122785031023,0.0865936051976101));
#27968=CARTESIAN_POINT('',(-0.0199747787412939,0.0210748891324553,0.0867258968642769));
#27969=CARTESIAN_POINT('',(-0.0175,0.0210748891324553,0.0868581885309434));
#27970=CARTESIAN_POINT('',(-0.0150252212587062,0.0210748891324554,0.0869904801976102));
#27971=CARTESIAN_POINT('',(-0.012882,0.0223122785031023,0.0871227718642768));
#27972=CARTESIAN_POINT('',(-0.0107387787412939,0.0235496678737492,0.0872550635309435));
#27973=CARTESIAN_POINT('',(-0.00950138937064697,0.0256928891324554,0.0873873551976101));
#27974=CARTESIAN_POINT('',(-0.00826400000000004,0.0278361103911615,0.0875196468642768));
#27975=CARTESIAN_POINT('',(-0.008264,0.0303108891324553,0.0876519385309434));
#27976=CARTESIAN_POINT('',(-0.00826400000000005,0.0327856678737492,0.0877842301976101));
#27977=CARTESIAN_POINT('',(-0.00950138937064697,0.0349288891324553,0.0879165218642768));
#27978=CARTESIAN_POINT('',(-0.0107387787412939,0.0370721103911615,0.0880488135309434));
#27979=CARTESIAN_POINT('',(-0.012882,0.0383094997618084,0.0881811051976101));
#27980=CARTESIAN_POINT('',(-0.0150252212587062,0.0395468891324554,0.0883133968642768));
#27981=CARTESIAN_POINT('',(-0.0175,0.0395468891324554,0.0884456885309434));
#27982=CARTESIAN_POINT('',(-0.0199747787412939,0.0395468891324554,0.0885779801976102));
#27983=CARTESIAN_POINT('',(-0.022118,0.0383094997618084,0.0887102718642768));
#27984=CARTESIAN_POINT('',(-0.0242612212587062,0.0370721103911615,0.0888425635309435));
#27985=CARTESIAN_POINT('',(-0.0254986106293531,0.0349288891324553,0.0889748551976101));
#27986=CARTESIAN_POINT('',(-0.0267360000000001,0.0327856678737492,0.0891071468642768));
#27987=CARTESIAN_POINT('',(-0.026736,0.0303108891324553,0.0892394385309434));
#27988=CARTESIAN_POINT('',(-0.0234697589126183,0.0370631346381821,0.0830000000000001));
#27989=CARTESIAN_POINT('',(-0.0245706194344714,0.0360898477654954,0.0830831764537999));
#27990=CARTESIAN_POINT('',(-0.0253053270676696,0.0348172968160874,0.0831636705648742));
#27991=CARTESIAN_POINT('',(-0.0265128153672642,0.0327258657316446,0.083295962231541));
#27992=CARTESIAN_POINT('',(-0.0265128153672642,0.0303108891324553,0.0834282538982076));
#27993=CARTESIAN_POINT('',(-0.0265128153672642,0.0278959125332661,0.0835605455648743));
#27994=CARTESIAN_POINT('',(-0.0253053270676696,0.0258044814488233,0.0836928372315409));
#27995=CARTESIAN_POINT('',(-0.024097838768075,0.0237130503643804,0.0838251288982076));
#27996=CARTESIAN_POINT('',(-0.0220064076836321,0.0225055620647858,0.0839574205648743));
#27997=CARTESIAN_POINT('',(-0.0199149765991893,0.0212980737651912,0.0840897122315409));
#27998=CARTESIAN_POINT('',(-0.0175,0.0212980737651912,0.0842220038982076));
#27999=CARTESIAN_POINT('',(-0.0150850234008108,0.0212980737651912,0.0843542955648742));
#28000=CARTESIAN_POINT('',(-0.012993592316368,0.0225055620647858,0.0844865872315409));
#28001=CARTESIAN_POINT('',(-0.0109021612319251,0.0237130503643804,0.0846188788982076));
#28002=CARTESIAN_POINT('',(-0.00969467293233052,0.0258044814488233,0.0847511705648743));
#28003=CARTESIAN_POINT('',(-0.00848718463273591,0.0278959125332661,0.084883462231541));
#28004=CARTESIAN_POINT('',(-0.0084871846327359,0.0303108891324553,0.0850157538982076));
#28005=CARTESIAN_POINT('',(-0.00848718463273591,0.0327258657316446,0.0851480455648743));
#28006=CARTESIAN_POINT('',(-0.00969467293233052,0.0348172968160874,0.0852803372315409));
#28007=CARTESIAN_POINT('',(-0.0109021612319251,0.0369087279005303,0.0854126288982076));
#28008=CARTESIAN_POINT('',(-0.012993592316368,0.0381162162001248,0.0855449205648742));
#28009=CARTESIAN_POINT('',(-0.0150850234008108,0.0393237044997195,0.0856772122315409));
#28010=CARTESIAN_POINT('',(-0.0175,0.0393237044997195,0.0858095038982076));
#28011=CARTESIAN_POINT('',(-0.0199149765991893,0.0393237044997195,0.0859417955648742));
#28012=CARTESIAN_POINT('',(-0.0220064076836321,0.0381162162001248,0.0860740872315409));
#28013=CARTESIAN_POINT('',(-0.024097838768075,0.0369087279005302,0.0862063788982076));
#28014=CARTESIAN_POINT('',(-0.0253053270676696,0.0348172968160874,0.0863386705648743));
#28015=CARTESIAN_POINT('',(-0.0265128153672642,0.0327258657316446,0.086470962231541));
#28016=CARTESIAN_POINT('',(-0.0265128153672642,0.0303108891324553,0.0866032538982076));
#28017=CARTESIAN_POINT('',(-0.0265128153672642,0.0278959125332661,0.0867355455648743));
#28018=CARTESIAN_POINT('',(-0.0253053270676696,0.0258044814488233,0.0868678372315409));
#28019=CARTESIAN_POINT('',(-0.024097838768075,0.0237130503643804,0.0870001288982076));
#28020=CARTESIAN_POINT('',(-0.0220064076836321,0.0225055620647858,0.0871324205648743));
#28021=CARTESIAN_POINT('',(-0.0199149765991893,0.0212980737651912,0.0872647122315409));
#28022=CARTESIAN_POINT('',(-0.0175,0.0212980737651912,0.0873970038982076));
#28023=CARTESIAN_POINT('',(-0.0150850234008108,0.0212980737651912,0.0875292955648742));
#28024=CARTESIAN_POINT('',(-0.012993592316368,0.0225055620647858,0.0876615872315409));
#28025=CARTESIAN_POINT('',(-0.0109021612319251,0.0237130503643804,0.0877938788982077));
#28026=CARTESIAN_POINT('',(-0.00969467293233052,0.0258044814488233,0.0879261705648742));
#28027=CARTESIAN_POINT('',(-0.00848718463273591,0.0278959125332661,0.088058462231541));
#28028=CARTESIAN_POINT('',(-0.0084871846327359,0.0303108891324553,0.0881907538982076));
#28029=CARTESIAN_POINT('',(-0.00848718463273591,0.0327258657316446,0.0883230455648743));
#28030=CARTESIAN_POINT('',(-0.00969467293233052,0.0348172968160874,0.0884553372315409));
#28031=CARTESIAN_POINT('',(-0.0109021612319251,0.0369087279005303,0.0885876288982076));
#28032=CARTESIAN_POINT('',(-0.012993592316368,0.0381162162001248,0.0887199205648743));
#28033=CARTESIAN_POINT('',(-0.0150850234008108,0.0393237044997195,0.0888522122315409));
#28034=CARTESIAN_POINT('',(-0.0175,0.0393237044997195,0.0889845038982076));
#28035=CARTESIAN_POINT('',(-0.0199149765991893,0.0393237044997195,0.0891167955648742));
#28036=CARTESIAN_POINT('',(-0.0220064076836321,0.0381162162001248,0.0892490872315409));
#28037=CARTESIAN_POINT('',(-0.024097838768075,0.0369087279005302,0.0893813788982077));
#28038=CARTESIAN_POINT('',(-0.0253053270676696,0.0348172968160874,0.0895136705648743));
#28039=CARTESIAN_POINT('',(-0.0265128153672642,0.0327258657316446,0.0896459622315409));
#28040=CARTESIAN_POINT('',(-0.0265128153672642,0.0303108891324553,0.0897782538982076));
#28041=CARTESIAN_POINT('',(-0.0234697589126183,0.0370631346381822,0.083));
#28042=CARTESIAN_POINT('',(-0.0265128153672642,0.0303108891324553,0.0897782538982076));
#28043=CARTESIAN_POINT('',(-0.0234697589126183,0.0370631346381822,0.083));
#28044=CARTESIAN_POINT('',(-0.02476030267836,0.0360460956012747,0.083));
#28045=CARTESIAN_POINT('',(-0.0262028298061085,0.0339579466917452,0.0829999999999999));
#28046=CARTESIAN_POINT('',(-0.0268263894154986,0.0307216863639011,0.083));
#28047=CARTESIAN_POINT('',(-0.0266934574485126,0.0291033126587244,0.083));
#28048=CARTESIAN_POINT('',(-0.0265148517458493,0.0283018734529848,0.083));
#28049=CARTESIAN_POINT('',(-0.025974,0.0303108891324553,0.0892394385309434));
#28050=CARTESIAN_POINT('',(-0.0128220863881535,0.037278617891806,0.0829566731169614));
#28051=CARTESIAN_POINT('',(-0.0130578663098391,0.0374369131043705,0.0829736444091975));
#28052=CARTESIAN_POINT('',(-0.0133038076836321,0.0375789074227348,0.0829903512994025));
#28053=CARTESIAN_POINT('',(-0.0152512673150871,0.0387032737651912,0.0831226429660692));
#28054=CARTESIAN_POINT('',(-0.0175,0.0387032737651912,0.0832549346327359));
#28055=CARTESIAN_POINT('',(-0.019748732684913,0.0387032737651912,0.0833872262994025));
#28056=CARTESIAN_POINT('',(-0.021696192316368,0.0375789074227348,0.0835195179660692));
#28057=CARTESIAN_POINT('',(-0.023643651947823,0.0364545410802783,0.083651809632736));
#28058=CARTESIAN_POINT('',(-0.0247680182902794,0.0345070814488233,0.0837841012994025));
#28059=CARTESIAN_POINT('',(-0.0258923846327359,0.0325596218173683,0.0839163929660693));
#28060=CARTESIAN_POINT('',(-0.0258923846327359,0.0303108891324553,0.0840486846327359));
#28061=CARTESIAN_POINT('',(-0.0258923846327359,0.0280621564475424,0.0841809762994026));
#28062=CARTESIAN_POINT('',(-0.0247680182902794,0.0261146968160874,0.0843132679660692));
#28063=CARTESIAN_POINT('',(-0.023643651947823,0.0241672371846324,0.0844455596327359));
#28064=CARTESIAN_POINT('',(-0.021696192316368,0.023042870842176,0.0845778512994025));
#28065=CARTESIAN_POINT('',(-0.019748732684913,0.0219185044997195,0.0847101429660692));
#28066=CARTESIAN_POINT('',(-0.0175,0.0219185044997195,0.0848424346327359));
#28067=CARTESIAN_POINT('',(-0.0152512673150871,0.0219185044997195,0.0849747262994025));
#28068=CARTESIAN_POINT('',(-0.0133038076836321,0.023042870842176,0.0851070179660692));
#28069=CARTESIAN_POINT('',(-0.0113563480521771,0.0241672371846324,0.0852393096327359));
#28070=CARTESIAN_POINT('',(-0.0102319817097207,0.0261146968160874,0.0853716012994025));
#28071=CARTESIAN_POINT('',(-0.00910761536726418,0.0280621564475424,0.0855038929660693));
#28072=CARTESIAN_POINT('',(-0.00910761536726419,0.0303108891324553,0.0856361846327359));
#28073=CARTESIAN_POINT('',(-0.00910761536726419,0.0325596218173683,0.0857684762994026));
#28074=CARTESIAN_POINT('',(-0.0102319817097207,0.0345070814488233,0.0859007679660692));
#28075=CARTESIAN_POINT('',(-0.0113563480521771,0.0364545410802783,0.0860330596327359));
#28076=CARTESIAN_POINT('',(-0.0133038076836321,0.0375789074227348,0.0861653512994025));
#28077=CARTESIAN_POINT('',(-0.0152512673150871,0.0387032737651912,0.0862976429660692));
#28078=CARTESIAN_POINT('',(-0.0175,0.0387032737651912,0.0864299346327359));
#28079=CARTESIAN_POINT('',(-0.019748732684913,0.0387032737651912,0.0865622262994026));
#28080=CARTESIAN_POINT('',(-0.021696192316368,0.0375789074227348,0.0866945179660692));
#28081=CARTESIAN_POINT('',(-0.023643651947823,0.0364545410802783,0.0868268096327359));
#28082=CARTESIAN_POINT('',(-0.0247680182902794,0.0345070814488233,0.0869591012994025));
#28083=CARTESIAN_POINT('',(-0.0258923846327359,0.0325596218173683,0.0870913929660692));
#28084=CARTESIAN_POINT('',(-0.0258923846327359,0.0303108891324553,0.0872236846327359));
#28085=CARTESIAN_POINT('',(-0.0258923846327359,0.0280621564475424,0.0873559762994026));
#28086=CARTESIAN_POINT('',(-0.0247680182902794,0.0261146968160874,0.0874882679660692));
#28087=CARTESIAN_POINT('',(-0.023643651947823,0.0241672371846324,0.0876205596327359));
#28088=CARTESIAN_POINT('',(-0.021696192316368,0.023042870842176,0.0877528512994025));
#28089=CARTESIAN_POINT('',(-0.019748732684913,0.0219185044997195,0.0878851429660692));
#28090=CARTESIAN_POINT('',(-0.0175,0.0219185044997195,0.0880174346327359));
#28091=CARTESIAN_POINT('',(-0.0152512673150871,0.0219185044997195,0.0881497262994026));
#28092=CARTESIAN_POINT('',(-0.0133038076836321,0.023042870842176,0.0882820179660692));
#28093=CARTESIAN_POINT('',(-0.0113563480521771,0.0241672371846324,0.0884143096327359));
#28094=CARTESIAN_POINT('',(-0.0102319817097207,0.0261146968160874,0.0885466012994025));
#28095=CARTESIAN_POINT('',(-0.00910761536726418,0.0280621564475424,0.0886788929660693));
#28096=CARTESIAN_POINT('',(-0.00910761536726419,0.0303108891324553,0.0888111846327359));
#28097=CARTESIAN_POINT('',(-0.00910761536726419,0.0325596218173683,0.0889434762994026));
#28098=CARTESIAN_POINT('',(-0.0102319817097207,0.0345070814488233,0.0890757679660692));
#28099=CARTESIAN_POINT('',(-0.0113563480521771,0.0364545410802783,0.0892080596327359));
#28100=CARTESIAN_POINT('',(-0.0133038076836321,0.0375789074227348,0.0893403512994025));
#28101=CARTESIAN_POINT('',(-0.0152512673150871,0.0387032737651912,0.0894726429660692));
#28102=CARTESIAN_POINT('',(-0.0175,0.0387032737651912,0.0896049346327359));
#28103=CARTESIAN_POINT('',(-0.019748732684913,0.0387032737651912,0.0897372262994026));
#28104=CARTESIAN_POINT('',(-0.021696192316368,0.0375789074227348,0.0898695179660692));
#28105=CARTESIAN_POINT('',(-0.023643651947823,0.0364545410802783,0.0900018096327359));
#28106=CARTESIAN_POINT('',(-0.0247680182902794,0.0345070814488233,0.0901341012994025));
#28107=CARTESIAN_POINT('',(-0.0258923846327359,0.0325596218173683,0.0902663929660692));
#28108=CARTESIAN_POINT('',(-0.0258923846327359,0.0303108891324553,0.0903986846327359));
#28109=CARTESIAN_POINT('',(-0.0124762584137138,0.0377937269175881,0.0823362423824331));
#28110=CARTESIAN_POINT('',(-0.0127294690319654,0.0379637245507758,0.0823532136746692));
#28111=CARTESIAN_POINT('',(-0.012993592316368,0.0381162162001248,0.0823699205648742));
#28112=CARTESIAN_POINT('',(-0.0150850234008108,0.0393237044997195,0.0825022122315409));
#28113=CARTESIAN_POINT('',(-0.0175,0.0393237044997195,0.0826345038982076));
#28114=CARTESIAN_POINT('',(-0.0199149765991893,0.0393237044997195,0.0827667955648743));
#28115=CARTESIAN_POINT('',(-0.0220064076836321,0.0381162162001248,0.0828990872315409));
#28116=CARTESIAN_POINT('',(-0.024097838768075,0.0369087279005302,0.0830313788982076));
#28117=CARTESIAN_POINT('',(-0.0253053270676696,0.0348172968160874,0.0831636705648742));
#28118=CARTESIAN_POINT('',(-0.0265128153672642,0.0327258657316446,0.083295962231541));
#28119=CARTESIAN_POINT('',(-0.0265128153672642,0.0303108891324553,0.0834282538982076));
#28120=CARTESIAN_POINT('',(-0.0265128153672642,0.0278959125332661,0.0835605455648743));
#28121=CARTESIAN_POINT('',(-0.0253053270676696,0.0258044814488233,0.0836928372315409));
#28122=CARTESIAN_POINT('',(-0.024097838768075,0.0237130503643804,0.0838251288982076));
#28123=CARTESIAN_POINT('',(-0.0220064076836321,0.0225055620647858,0.0839574205648743));
#28124=CARTESIAN_POINT('',(-0.0199149765991893,0.0212980737651912,0.0840897122315409));
#28125=CARTESIAN_POINT('',(-0.0175,0.0212980737651912,0.0842220038982076));
#28126=CARTESIAN_POINT('',(-0.0150850234008108,0.0212980737651912,0.0843542955648742));
#28127=CARTESIAN_POINT('',(-0.012993592316368,0.0225055620647858,0.0844865872315409));
#28128=CARTESIAN_POINT('',(-0.0109021612319251,0.0237130503643804,0.0846188788982076));
#28129=CARTESIAN_POINT('',(-0.00969467293233052,0.0258044814488233,0.0847511705648743));
#28130=CARTESIAN_POINT('',(-0.0084871846327359,0.0278959125332661,0.084883462231541));
#28131=CARTESIAN_POINT('',(-0.0084871846327359,0.0303108891324553,0.0850157538982076));
#28132=CARTESIAN_POINT('',(-0.0084871846327359,0.0327258657316446,0.0851480455648743));
#28133=CARTESIAN_POINT('',(-0.00969467293233052,0.0348172968160874,0.0852803372315409));
#28134=CARTESIAN_POINT('',(-0.0109021612319251,0.0369087279005303,0.0854126288982076));
#28135=CARTESIAN_POINT('',(-0.012993592316368,0.0381162162001248,0.0855449205648742));
#28136=CARTESIAN_POINT('',(-0.0150850234008108,0.0393237044997195,0.0856772122315409));
#28137=CARTESIAN_POINT('',(-0.0175,0.0393237044997195,0.0858095038982076));
#28138=CARTESIAN_POINT('',(-0.0199149765991893,0.0393237044997195,0.0859417955648742));
#28139=CARTESIAN_POINT('',(-0.0220064076836321,0.0381162162001248,0.0860740872315409));
#28140=CARTESIAN_POINT('',(-0.024097838768075,0.0369087279005302,0.0862063788982076));
#28141=CARTESIAN_POINT('',(-0.0253053270676696,0.0348172968160874,0.0863386705648743));
#28142=CARTESIAN_POINT('',(-0.0265128153672642,0.0327258657316446,0.086470962231541));
#28143=CARTESIAN_POINT('',(-0.0265128153672642,0.0303108891324553,0.0866032538982076));
#28144=CARTESIAN_POINT('',(-0.0265128153672642,0.0278959125332661,0.0867355455648743));
#28145=CARTESIAN_POINT('',(-0.0253053270676696,0.0258044814488233,0.0868678372315409));
#28146=CARTESIAN_POINT('',(-0.024097838768075,0.0237130503643804,0.0870001288982076));
#28147=CARTESIAN_POINT('',(-0.0220064076836321,0.0225055620647858,0.0871324205648743));
#28148=CARTESIAN_POINT('',(-0.0199149765991893,0.0212980737651912,0.0872647122315409));
#28149=CARTESIAN_POINT('',(-0.0175,0.0212980737651912,0.0873970038982076));
#28150=CARTESIAN_POINT('',(-0.0150850234008108,0.0212980737651912,0.0875292955648742));
#28151=CARTESIAN_POINT('',(-0.012993592316368,0.0225055620647858,0.0876615872315409));
#28152=CARTESIAN_POINT('',(-0.0109021612319251,0.0237130503643804,0.0877938788982077));
#28153=CARTESIAN_POINT('',(-0.00969467293233052,0.0258044814488233,0.0879261705648742));
#28154=CARTESIAN_POINT('',(-0.0084871846327359,0.0278959125332661,0.088058462231541));
#28155=CARTESIAN_POINT('',(-0.0084871846327359,0.0303108891324553,0.0881907538982076));
#28156=CARTESIAN_POINT('',(-0.0084871846327359,0.0327258657316446,0.0883230455648743));
#28157=CARTESIAN_POINT('',(-0.00969467293233052,0.0348172968160874,0.0884553372315409));
#28158=CARTESIAN_POINT('',(-0.0109021612319251,0.0369087279005303,0.0885876288982076));
#28159=CARTESIAN_POINT('',(-0.012993592316368,0.0381162162001248,0.0887199205648743));
#28160=CARTESIAN_POINT('',(-0.0150850234008108,0.0393237044997195,0.0888522122315409));
#28161=CARTESIAN_POINT('',(-0.0175,0.0393237044997195,0.0889845038982076));
#28162=CARTESIAN_POINT('',(-0.0199149765991893,0.0393237044997195,0.0891167955648742));
#28163=CARTESIAN_POINT('',(-0.0220064076836321,0.0381162162001248,0.0892490872315409));
#28164=CARTESIAN_POINT('',(-0.024097838768075,0.0369087279005302,0.0893813788982077));
#28165=CARTESIAN_POINT('',(-0.0253053270676696,0.0348172968160874,0.0895136705648743));
#28166=CARTESIAN_POINT('',(-0.0265128153672642,0.0327258657316446,0.0896459622315409));
#28167=CARTESIAN_POINT('',(-0.0265128153672642,0.0303108891324553,0.0897782538982076));
#28168=CARTESIAN_POINT('',(-0.0134462729974218,0.0376593187070208,0.0830000000000001));
#28169=CARTESIAN_POINT('',(-0.0153387117874777,0.0387032737651912,0.0831277872747151));
#28170=CARTESIAN_POINT('',(-0.0175,0.0387032737651912,0.0832549346327359));
#28171=CARTESIAN_POINT('',(-0.019748732684913,0.0387032737651912,0.0833872262994025));
#28172=CARTESIAN_POINT('',(-0.021696192316368,0.0375789074227348,0.0835195179660692));
#28173=CARTESIAN_POINT('',(-0.023643651947823,0.0364545410802783,0.083651809632736));
#28174=CARTESIAN_POINT('',(-0.0247680182902794,0.0345070814488233,0.0837841012994025));
#28175=CARTESIAN_POINT('',(-0.0258923846327359,0.0325596218173683,0.0839163929660692));
#28176=CARTESIAN_POINT('',(-0.0258923846327359,0.0303108891324553,0.0840486846327359));
#28177=CARTESIAN_POINT('',(-0.0258923846327359,0.0280621564475424,0.0841809762994026));
#28178=CARTESIAN_POINT('',(-0.0247680182902794,0.0261146968160874,0.0843132679660692));
#28179=CARTESIAN_POINT('',(-0.023643651947823,0.0241672371846324,0.0844455596327359));
#28180=CARTESIAN_POINT('',(-0.021696192316368,0.023042870842176,0.0845778512994025));
#28181=CARTESIAN_POINT('',(-0.019748732684913,0.0219185044997195,0.0847101429660692));
#28182=CARTESIAN_POINT('',(-0.0175,0.0219185044997195,0.0848424346327359));
#28183=CARTESIAN_POINT('',(-0.0152512673150871,0.0219185044997195,0.0849747262994025));
#28184=CARTESIAN_POINT('',(-0.0133038076836321,0.023042870842176,0.0851070179660692));
#28185=CARTESIAN_POINT('',(-0.0113563480521771,0.0241672371846324,0.0852393096327359));
#28186=CARTESIAN_POINT('',(-0.0102319817097207,0.0261146968160874,0.0853716012994025));
#28187=CARTESIAN_POINT('',(-0.00910761536726419,0.0280621564475424,0.0855038929660693));
#28188=CARTESIAN_POINT('',(-0.00910761536726419,0.0303108891324553,0.0856361846327359));
#28189=CARTESIAN_POINT('',(-0.00910761536726419,0.0325596218173683,0.0857684762994026));
#28190=CARTESIAN_POINT('',(-0.0102319817097207,0.0345070814488233,0.0859007679660692));
#28191=CARTESIAN_POINT('',(-0.0113563480521771,0.0364545410802783,0.0860330596327359));
#28192=CARTESIAN_POINT('',(-0.0133038076836321,0.0375789074227348,0.0861653512994025));
#28193=CARTESIAN_POINT('',(-0.0152512673150871,0.0387032737651912,0.0862976429660692));
#28194=CARTESIAN_POINT('',(-0.0175,0.0387032737651912,0.0864299346327359));
#28195=CARTESIAN_POINT('',(-0.019748732684913,0.0387032737651912,0.0865622262994026));
#28196=CARTESIAN_POINT('',(-0.021696192316368,0.0375789074227348,0.0866945179660692));
#28197=CARTESIAN_POINT('',(-0.023643651947823,0.0364545410802783,0.0868268096327359));
#28198=CARTESIAN_POINT('',(-0.0247680182902794,0.0345070814488233,0.0869591012994025));
#28199=CARTESIAN_POINT('',(-0.0258923846327359,0.0325596218173683,0.0870913929660692));
#28200=CARTESIAN_POINT('',(-0.0258923846327359,0.0303108891324553,0.0872236846327359));
#28201=CARTESIAN_POINT('',(-0.0258923846327359,0.0280621564475424,0.0873559762994026));
#28202=CARTESIAN_POINT('',(-0.0247680182902794,0.0261146968160874,0.0874882679660692));
#28203=CARTESIAN_POINT('',(-0.023643651947823,0.0241672371846324,0.0876205596327359));
#28204=CARTESIAN_POINT('',(-0.021696192316368,0.023042870842176,0.0877528512994025));
#28205=CARTESIAN_POINT('',(-0.019748732684913,0.0219185044997195,0.0878851429660692));
#28206=CARTESIAN_POINT('',(-0.0175,0.0219185044997195,0.0880174346327359));
#28207=CARTESIAN_POINT('',(-0.0152512673150871,0.0219185044997195,0.0881497262994026));
#28208=CARTESIAN_POINT('',(-0.0133038076836321,0.023042870842176,0.0882820179660692));
#28209=CARTESIAN_POINT('',(-0.0113563480521771,0.0241672371846324,0.0884143096327359));
#28210=CARTESIAN_POINT('',(-0.0102319817097207,0.0261146968160874,0.0885466012994025));
#28211=CARTESIAN_POINT('',(-0.00910761536726419,0.0280621564475424,0.0886788929660692));
#28212=CARTESIAN_POINT('',(-0.00910761536726419,0.0303108891324553,0.0888111846327359));
#28213=CARTESIAN_POINT('',(-0.00910761536726419,0.0325596218173683,0.0889434762994026));
#28214=CARTESIAN_POINT('',(-0.0102319817097207,0.0345070814488233,0.0890757679660692));
#28215=CARTESIAN_POINT('',(-0.0113563480521771,0.0364545410802783,0.0892080596327359));
#28216=CARTESIAN_POINT('',(-0.0133038076836321,0.0375789074227348,0.0893403512994025));
#28217=CARTESIAN_POINT('',(-0.0152512673150871,0.0387032737651912,0.0894726429660692));
#28218=CARTESIAN_POINT('',(-0.0175,0.0387032737651912,0.0896049346327359));
#28219=CARTESIAN_POINT('',(-0.019748732684913,0.0387032737651912,0.0897372262994026));
#28220=CARTESIAN_POINT('',(-0.021696192316368,0.0375789074227348,0.0898695179660692));
#28221=CARTESIAN_POINT('',(-0.023643651947823,0.0364545410802783,0.0900018096327359));
#28222=CARTESIAN_POINT('',(-0.0247680182902794,0.0345070814488233,0.0901341012994025));
#28223=CARTESIAN_POINT('',(-0.0258923846327359,0.0325596218173683,0.0902663929660692));
#28224=CARTESIAN_POINT('',(-0.0258923846327359,0.0303108891324553,0.0903986846327359));
#28225=CARTESIAN_POINT('',(-0.0134462729974218,0.0376593187070208,0.083));
#28226=CARTESIAN_POINT('',(-0.0258923846327359,0.0303108891324553,0.0903986846327359));
#28227=CARTESIAN_POINT('',(-0.0134462729974218,0.0376593187070208,0.083));
#28228=CARTESIAN_POINT('',(-0.0149685242548422,0.038620412767118,0.083));
#28229=CARTESIAN_POINT('',(-0.0176826196805459,0.0392910823435752,0.083));
#28230=CARTESIAN_POINT('',(-0.0212176395987549,0.0385051138778108,0.0830000000000001));
#28231=CARTESIAN_POINT('',(-0.0227632438890936,0.0376199180485249,0.083));
#28232=CARTESIAN_POINT('',(-0.0234697589126183,0.0370631346381822,0.083));
#28233=CARTESIAN_POINT('',(-0.0262026,0.0303108891324553,0.0900884692654717));
#28234=CARTESIAN_POINT('',(-0.0093308,0.0303108891324553,0.083));
#28235=CARTESIAN_POINT('',(-0.00933080000000005,0.0324998196752637,0.0831322916666668));
#28236=CARTESIAN_POINT('',(-0.0104252652714042,0.0343954891324554,0.0832645833333334));
#28237=CARTESIAN_POINT('',(-0.0115197305428084,0.036291158589647,0.0833968750000001));
#28238=CARTESIAN_POINT('',(-0.0134154,0.0373856238610512,0.0835291666666667));
#28239=CARTESIAN_POINT('',(-0.0153110694571917,0.0384800891324553,0.0836614583333334));
#28240=CARTESIAN_POINT('',(-0.0175,0.0384800891324554,0.08379375));
#28241=CARTESIAN_POINT('',(-0.0196889305428084,0.0384800891324553,0.0839260416666667));
#28242=CARTESIAN_POINT('',(-0.0215846,0.0373856238610512,0.0840583333333334));
#28243=CARTESIAN_POINT('',(-0.0234802694571917,0.036291158589647,0.084190625));
#28244=CARTESIAN_POINT('',(-0.0245747347285959,0.0343954891324554,0.0843229166666667));
#28245=CARTESIAN_POINT('',(-0.0256692000000001,0.0324998196752637,0.0844552083333334));
#28246=CARTESIAN_POINT('',(-0.0256692,0.0303108891324553,0.0845875));
#28247=CARTESIAN_POINT('',(-0.0256692000000001,0.028121958589647,0.0847197916666667));
#28248=CARTESIAN_POINT('',(-0.0245747347285959,0.0262262891324554,0.0848520833333334));
#28249=CARTESIAN_POINT('',(-0.0234802694571917,0.0243306196752637,0.0849843750000001));
#28250=CARTESIAN_POINT('',(-0.0215846,0.0232361544038595,0.0851166666666667));
#28251=CARTESIAN_POINT('',(-0.0196889305428084,0.0221416891324553,0.0852489583333334));
#28252=CARTESIAN_POINT('',(-0.0175,0.0221416891324554,0.08538125));
#28253=CARTESIAN_POINT('',(-0.0153110694571917,0.0221416891324553,0.0855135416666667));
#28254=CARTESIAN_POINT('',(-0.0134154,0.0232361544038595,0.0856458333333334));
#28255=CARTESIAN_POINT('',(-0.0115197305428084,0.0243306196752637,0.0857781250000001));
#28256=CARTESIAN_POINT('',(-0.0104252652714042,0.0262262891324554,0.0859104166666667));
#28257=CARTESIAN_POINT('',(-0.00933080000000005,0.028121958589647,0.0860427083333334));
#28258=CARTESIAN_POINT('',(-0.0093308,0.0303108891324553,0.086175));
#28259=CARTESIAN_POINT('',(-0.00933080000000005,0.0324998196752637,0.0863072916666667));
#28260=CARTESIAN_POINT('',(-0.0104252652714042,0.0343954891324554,0.0864395833333334));
#28261=CARTESIAN_POINT('',(-0.0115197305428084,0.036291158589647,0.086571875));
#28262=CARTESIAN_POINT('',(-0.0134154,0.0373856238610512,0.0867041666666667));
#28263=CARTESIAN_POINT('',(-0.0153110694571917,0.0384800891324553,0.0868364583333334));
#28264=CARTESIAN_POINT('',(-0.0175,0.0384800891324554,0.08696875));
#28265=CARTESIAN_POINT('',(-0.0196889305428084,0.0384800891324553,0.0871010416666667));
#28266=CARTESIAN_POINT('',(-0.0215846,0.0373856238610512,0.0872333333333334));
#28267=CARTESIAN_POINT('',(-0.0234802694571917,0.036291158589647,0.087365625));
#28268=CARTESIAN_POINT('',(-0.0245747347285959,0.0343954891324554,0.0874979166666667));
#28269=CARTESIAN_POINT('',(-0.0256692000000001,0.0324998196752637,0.0876302083333334));
#28270=CARTESIAN_POINT('',(-0.0256692,0.0303108891324553,0.0877625));
#28271=CARTESIAN_POINT('',(-0.0256692000000001,0.028121958589647,0.0878947916666667));
#28272=CARTESIAN_POINT('',(-0.0245747347285959,0.0262262891324554,0.0880270833333334));
#28273=CARTESIAN_POINT('',(-0.0234802694571917,0.0243306196752637,0.088159375));
#28274=CARTESIAN_POINT('',(-0.0215846,0.0232361544038595,0.0882916666666667));
#28275=CARTESIAN_POINT('',(-0.0196889305428084,0.0221416891324553,0.0884239583333334));
#28276=CARTESIAN_POINT('',(-0.0175,0.0221416891324554,0.08855625));
#28277=CARTESIAN_POINT('',(-0.0153110694571917,0.0221416891324553,0.0886885416666667));
#28278=CARTESIAN_POINT('',(-0.0134154,0.0232361544038595,0.0888208333333334));
#28279=CARTESIAN_POINT('',(-0.0115197305428084,0.0243306196752637,0.088953125));
#28280=CARTESIAN_POINT('',(-0.0104252652714042,0.0262262891324554,0.0890854166666667));
#28281=CARTESIAN_POINT('',(-0.00933080000000005,0.028121958589647,0.0892177083333334));
#28282=CARTESIAN_POINT('',(-0.0093308,0.0303108891324553,0.08935));
#28283=CARTESIAN_POINT('',(-0.00933080000000005,0.0324998196752637,0.0894822916666667));
#28284=CARTESIAN_POINT('',(-0.0104252652714042,0.0343954891324554,0.0896145833333333));
#28285=CARTESIAN_POINT('',(-0.0115197305428084,0.036291158589647,0.0897468750000001));
#28286=CARTESIAN_POINT('',(-0.0134154,0.0373856238610512,0.0898791666666667));
#28287=CARTESIAN_POINT('',(-0.0153110694571917,0.0384800891324553,0.0900114583333334));
#28288=CARTESIAN_POINT('',(-0.0175,0.0384800891324554,0.09014375));
#28289=CARTESIAN_POINT('',(-0.0196889305428084,0.0384800891324553,0.0902760416666667));
#28290=CARTESIAN_POINT('',(-0.0215846,0.0373856238610512,0.0904083333333334));
#28291=CARTESIAN_POINT('',(-0.0234802694571917,0.036291158589647,0.0905406250000001));
#28292=CARTESIAN_POINT('',(-0.0245747347285959,0.0343954891324554,0.0906729166666667));
#28293=CARTESIAN_POINT('',(-0.0256692000000001,0.0324998196752637,0.0908052083333334));
#28294=CARTESIAN_POINT('',(-0.0256692,0.0303108891324553,0.0909375));
#28295=CARTESIAN_POINT('',(-0.00933080000000004,0.0303108891324554,0.0827952040402267));
#28296=CARTESIAN_POINT('',(-0.00933080000000004,0.0324998196752636,0.0829274957068934));
#28297=CARTESIAN_POINT('',(-0.0104252652714042,0.0343954891324553,0.0830597873735601));
#28298=CARTESIAN_POINT('',(-0.0115197305428084,0.036291158589647,0.0831920790402268));
#28299=CARTESIAN_POINT('',(-0.0134154000000001,0.0373856238610512,0.0833243707068934));
#28300=CARTESIAN_POINT('',(-0.0153110694571917,0.0384800891324553,0.0834566623735601));
#28301=CARTESIAN_POINT('',(-0.0175000000000001,0.0384800891324554,0.0835889540402267));
#28302=CARTESIAN_POINT('',(-0.0196889305428084,0.0384800891324553,0.0837212457068933));
#28303=CARTESIAN_POINT('',(-0.0215846000000001,0.0373856238610512,0.0838535373735601));
#28304=CARTESIAN_POINT('',(-0.0234802694571917,0.036291158589647,0.0839858290402267));
#28305=CARTESIAN_POINT('',(-0.0245747347285959,0.0343954891324553,0.0841181207068934));
#28306=CARTESIAN_POINT('',(-0.0256692000000001,0.0324998196752636,0.08425041237356));
#28307=CARTESIAN_POINT('',(-0.0256692000000001,0.0303108891324554,0.0843827040402267));
#28308=CARTESIAN_POINT('',(-0.0256692000000001,0.028121958589647,0.0845149957068933));
#28309=CARTESIAN_POINT('',(-0.0245747347285959,0.0262262891324553,0.0846472873735601));
#28310=CARTESIAN_POINT('',(-0.0234802694571917,0.0243306196752637,0.0847795790402267));
#28311=CARTESIAN_POINT('',(-0.0215846000000001,0.0232361544038595,0.0849118707068934));
#28312=CARTESIAN_POINT('',(-0.0196889305428084,0.0221416891324553,0.08504416237356));
#28313=CARTESIAN_POINT('',(-0.0175000000000001,0.0221416891324553,0.0851764540402268));
#28314=CARTESIAN_POINT('',(-0.0153110694571917,0.0221416891324553,0.0853087457068933));
#28315=CARTESIAN_POINT('',(-0.0134154000000001,0.0232361544038595,0.0854410373735601));
#28316=CARTESIAN_POINT('',(-0.0115197305428084,0.0243306196752637,0.0855733290402267));
#28317=CARTESIAN_POINT('',(-0.0104252652714042,0.0262262891324553,0.0857056207068934));
#28318=CARTESIAN_POINT('',(-0.00933080000000003,0.028121958589647,0.08583791237356));
#28319=CARTESIAN_POINT('',(-0.00933080000000004,0.0303108891324554,0.0859702040402268));
#28320=CARTESIAN_POINT('',(-0.00933080000000004,0.0324998196752636,0.0861024957068934));
#28321=CARTESIAN_POINT('',(-0.0104252652714042,0.0343954891324553,0.0862347873735601));
#28322=CARTESIAN_POINT('',(-0.0115197305428084,0.036291158589647,0.0863670790402267));
#28323=CARTESIAN_POINT('',(-0.0134154000000001,0.0373856238610512,0.0864993707068934));
#28324=CARTESIAN_POINT('',(-0.0153110694571917,0.0384800891324553,0.08663166237356));
#28325=CARTESIAN_POINT('',(-0.0175000000000001,0.0384800891324554,0.0867639540402267));
#28326=CARTESIAN_POINT('',(-0.0196889305428084,0.0384800891324553,0.0868962457068933));
#28327=CARTESIAN_POINT('',(-0.0215846000000001,0.0373856238610512,0.08702853737356));
#28328=CARTESIAN_POINT('',(-0.0234802694571917,0.036291158589647,0.0871608290402267));
#28329=CARTESIAN_POINT('',(-0.0245747347285959,0.0343954891324553,0.0872931207068933));
#28330=CARTESIAN_POINT('',(-0.0256692000000001,0.0324998196752636,0.08742541237356));
#28331=CARTESIAN_POINT('',(-0.0256692000000001,0.0303108891324554,0.0875577040402268));
#28332=CARTESIAN_POINT('',(-0.0256692000000001,0.028121958589647,0.0876899957068934));
#28333=CARTESIAN_POINT('',(-0.0245747347285959,0.0262262891324553,0.08782228737356));
#28334=CARTESIAN_POINT('',(-0.0234802694571917,0.0243306196752637,0.0879545790402267));
#28335=CARTESIAN_POINT('',(-0.0215846000000001,0.0232361544038595,0.0880868707068934));
#28336=CARTESIAN_POINT('',(-0.0196889305428084,0.0221416891324553,0.08821916237356));
#28337=CARTESIAN_POINT('',(-0.0175000000000001,0.0221416891324553,0.0883514540402267));
#28338=CARTESIAN_POINT('',(-0.0153110694571917,0.0221416891324553,0.0884837457068934));
#28339=CARTESIAN_POINT('',(-0.0134154000000001,0.0232361544038595,0.08861603737356));
#28340=CARTESIAN_POINT('',(-0.0115197305428084,0.0243306196752637,0.0887483290402267));
#28341=CARTESIAN_POINT('',(-0.0104252652714042,0.0262262891324553,0.0888806207068934));
#28342=CARTESIAN_POINT('',(-0.00933080000000003,0.028121958589647,0.08901291237356));
#28343=CARTESIAN_POINT('',(-0.00933080000000004,0.0303108891324554,0.0891452040402267));
#28344=CARTESIAN_POINT('',(-0.00933080000000004,0.0324998196752636,0.0892774957068934));
#28345=CARTESIAN_POINT('',(-0.0104252652714042,0.0343954891324553,0.08940978737356));
#28346=CARTESIAN_POINT('',(-0.0115197305428084,0.036291158589647,0.0895420790402267));
#28347=CARTESIAN_POINT('',(-0.0134154000000001,0.0373856238610512,0.0896743707068934));
#28348=CARTESIAN_POINT('',(-0.0153110694571917,0.0384800891324553,0.0898066623735601));
#28349=CARTESIAN_POINT('',(-0.0175000000000001,0.0384800891324554,0.0899389540402267));
#28350=CARTESIAN_POINT('',(-0.0196889305428084,0.0384800891324553,0.0900712457068934));
#28351=CARTESIAN_POINT('',(-0.0215846000000001,0.0373856238610512,0.09020353737356));
#28352=CARTESIAN_POINT('',(-0.0234802694571917,0.036291158589647,0.0903358290402267));
#28353=CARTESIAN_POINT('',(-0.0245747347285959,0.0343954891324553,0.0904681207068934));
#28354=CARTESIAN_POINT('',(-0.0256692000000001,0.0324998196752636,0.0906004123735601));
#28355=CARTESIAN_POINT('',(-0.0256692000000001,0.0303108891324554,0.0907327040402267));
#28356=CARTESIAN_POINT('',(-0.00925242797917949,0.0303108891324554,0.0826059972446511));
#28357=CARTESIAN_POINT('',(-0.0092524279791795,0.0325208193949517,0.0827382889113178));
#28358=CARTESIAN_POINT('',(-0.0103573931104277,0.0344346751428656,0.0828705805779845));
#28359=CARTESIAN_POINT('',(-0.0114623582416759,0.0363485308907795,0.0830028722446511));
#28360=CARTESIAN_POINT('',(-0.0133762139895898,0.0374534960220277,0.0831351639113178));
#28361=CARTESIAN_POINT('',(-0.0152900697375036,0.0385584611532759,0.0832674555779845));
#28362=CARTESIAN_POINT('',(-0.0175000000000001,0.0385584611532759,0.0833997472446512));
#28363=CARTESIAN_POINT('',(-0.0197099302624964,0.0385584611532759,0.0835320389113178));
#28364=CARTESIAN_POINT('',(-0.0216237860104103,0.0374534960220277,0.0836643305779845));
#28365=CARTESIAN_POINT('',(-0.0235376417583242,0.0363485308907795,0.0837966222446511));
#28366=CARTESIAN_POINT('',(-0.0246426068895724,0.0344346751428656,0.0839289139113178));
#28367=CARTESIAN_POINT('',(-0.0257475720208206,0.0325208193949517,0.0840612055779845));
#28368=CARTESIAN_POINT('',(-0.0257475720208206,0.0303108891324554,0.0841934972446512));
#28369=CARTESIAN_POINT('',(-0.0257475720208206,0.0281009588699589,0.0843257889113178));
#28370=CARTESIAN_POINT('',(-0.0246426068895724,0.026187103122045,0.0844580805779845));
#28371=CARTESIAN_POINT('',(-0.0235376417583242,0.0242732473741312,0.0845903722446511));
#28372=CARTESIAN_POINT('',(-0.0216237860104103,0.023168282242883,0.0847226639113178));
#28373=CARTESIAN_POINT('',(-0.0197099302624964,0.0220633171116348,0.0848549555779845));
#28374=CARTESIAN_POINT('',(-0.0175000000000001,0.0220633171116348,0.0849872472446512));
#28375=CARTESIAN_POINT('',(-0.0152900697375036,0.0220633171116348,0.0851195389113178));
#28376=CARTESIAN_POINT('',(-0.0133762139895898,0.023168282242883,0.0852518305779845));
#28377=CARTESIAN_POINT('',(-0.0114623582416759,0.0242732473741312,0.0853841222446512));
#28378=CARTESIAN_POINT('',(-0.0103573931104277,0.026187103122045,0.0855164139113179));
#28379=CARTESIAN_POINT('',(-0.0092524279791795,0.0281009588699589,0.0856487055779845));
#28380=CARTESIAN_POINT('',(-0.00925242797917949,0.0303108891324554,0.0857809972446512));
#28381=CARTESIAN_POINT('',(-0.0092524279791795,0.0325208193949517,0.0859132889113178));
#28382=CARTESIAN_POINT('',(-0.0103573931104277,0.0344346751428656,0.0860455805779845));
#28383=CARTESIAN_POINT('',(-0.0114623582416759,0.0363485308907795,0.0861778722446511));
#28384=CARTESIAN_POINT('',(-0.0133762139895898,0.0374534960220277,0.0863101639113179));
#28385=CARTESIAN_POINT('',(-0.0152900697375036,0.0385584611532759,0.0864424555779845));
#28386=CARTESIAN_POINT('',(-0.0175000000000001,0.0385584611532759,0.0865747472446512));
#28387=CARTESIAN_POINT('',(-0.0197099302624964,0.0385584611532759,0.0867070389113178));
#28388=CARTESIAN_POINT('',(-0.0216237860104103,0.0374534960220277,0.0868393305779845));
#28389=CARTESIAN_POINT('',(-0.0235376417583242,0.0363485308907795,0.0869716222446512));
#28390=CARTESIAN_POINT('',(-0.0246426068895724,0.0344346751428656,0.0871039139113179));
#28391=CARTESIAN_POINT('',(-0.0257475720208206,0.0325208193949517,0.0872362055779845));
#28392=CARTESIAN_POINT('',(-0.0257475720208206,0.0303108891324554,0.0873684972446512));
#28393=CARTESIAN_POINT('',(-0.0257475720208206,0.0281009588699589,0.0875007889113178));
#28394=CARTESIAN_POINT('',(-0.0246426068895724,0.026187103122045,0.0876330805779846));
#28395=CARTESIAN_POINT('',(-0.0235376417583242,0.0242732473741312,0.0877653722446512));
#28396=CARTESIAN_POINT('',(-0.0216237860104103,0.023168282242883,0.0878976639113178));
#28397=CARTESIAN_POINT('',(-0.0197099302624964,0.0220633171116348,0.0880299555779845));
#28398=CARTESIAN_POINT('',(-0.0175000000000001,0.0220633171116348,0.0881622472446511));
#28399=CARTESIAN_POINT('',(-0.0152900697375036,0.0220633171116348,0.0882945389113178));
#28400=CARTESIAN_POINT('',(-0.0133762139895898,0.023168282242883,0.0884268305779846));
#28401=CARTESIAN_POINT('',(-0.0114623582416759,0.0242732473741312,0.0885591222446512));
#28402=CARTESIAN_POINT('',(-0.0103573931104277,0.026187103122045,0.0886914139113178));
#28403=CARTESIAN_POINT('',(-0.0092524279791795,0.0281009588699589,0.0888237055779845));
#28404=CARTESIAN_POINT('',(-0.00925242797917949,0.0303108891324554,0.0889559972446511));
#28405=CARTESIAN_POINT('',(-0.0092524279791795,0.0325208193949517,0.0890882889113179));
#28406=CARTESIAN_POINT('',(-0.0103573931104277,0.0344346751428656,0.0892205805779845));
#28407=CARTESIAN_POINT('',(-0.0114623582416759,0.0363485308907795,0.0893528722446512));
#28408=CARTESIAN_POINT('',(-0.0133762139895898,0.0374534960220277,0.0894851639113178));
#28409=CARTESIAN_POINT('',(-0.0152900697375036,0.0385584611532759,0.0896174555779845));
#28410=CARTESIAN_POINT('',(-0.0175000000000001,0.0385584611532759,0.0897497472446512));
#28411=CARTESIAN_POINT('',(-0.0197099302624964,0.0385584611532759,0.0898820389113179));
#28412=CARTESIAN_POINT('',(-0.0216237860104103,0.0374534960220277,0.0900143305779845));
#28413=CARTESIAN_POINT('',(-0.0235376417583242,0.0363485308907795,0.0901466222446512));
#28414=CARTESIAN_POINT('',(-0.0246426068895724,0.0344346751428656,0.0902789139113178));
#28415=CARTESIAN_POINT('',(-0.0257475720208206,0.0325208193949517,0.0904112055779845));
#28416=CARTESIAN_POINT('',(-0.0257475720208206,0.0303108891324554,0.0905434972446512));
#28417=CARTESIAN_POINT('',(-0.00910761536726419,0.0303108891324553,0.0824611846327359));
#28418=CARTESIAN_POINT('',(-0.00910761536726419,0.0325596218173683,0.0825934762994026));
#28419=CARTESIAN_POINT('',(-0.0102319817097207,0.0345070814488233,0.0827257679660692));
#28420=CARTESIAN_POINT('',(-0.0113563480521771,0.0364545410802783,0.0828580596327359));
#28421=CARTESIAN_POINT('',(-0.0133038076836321,0.0375789074227348,0.0829903512994025));
#28422=CARTESIAN_POINT('',(-0.0152512673150871,0.0387032737651912,0.0831226429660692));
#28423=CARTESIAN_POINT('',(-0.0175,0.0387032737651912,0.0832549346327359));
#28424=CARTESIAN_POINT('',(-0.019748732684913,0.0387032737651912,0.0833872262994025));
#28425=CARTESIAN_POINT('',(-0.021696192316368,0.0375789074227348,0.0835195179660692));
#28426=CARTESIAN_POINT('',(-0.023643651947823,0.0364545410802783,0.083651809632736));
#28427=CARTESIAN_POINT('',(-0.0247680182902794,0.0345070814488233,0.0837841012994025));
#28428=CARTESIAN_POINT('',(-0.0258923846327359,0.0325596218173683,0.0839163929660693));
#28429=CARTESIAN_POINT('',(-0.0258923846327359,0.0303108891324553,0.0840486846327359));
#28430=CARTESIAN_POINT('',(-0.0258923846327359,0.0280621564475424,0.0841809762994026));
#28431=CARTESIAN_POINT('',(-0.0247680182902794,0.0261146968160874,0.0843132679660692));
#28432=CARTESIAN_POINT('',(-0.023643651947823,0.0241672371846324,0.0844455596327359));
#28433=CARTESIAN_POINT('',(-0.021696192316368,0.023042870842176,0.0845778512994025));
#28434=CARTESIAN_POINT('',(-0.019748732684913,0.0219185044997195,0.0847101429660692));
#28435=CARTESIAN_POINT('',(-0.0175,0.0219185044997195,0.0848424346327359));
#28436=CARTESIAN_POINT('',(-0.0152512673150871,0.0219185044997195,0.0849747262994025));
#28437=CARTESIAN_POINT('',(-0.0133038076836321,0.023042870842176,0.0851070179660692));
#28438=CARTESIAN_POINT('',(-0.0113563480521771,0.0241672371846324,0.0852393096327359));
#28439=CARTESIAN_POINT('',(-0.0102319817097207,0.0261146968160874,0.0853716012994025));
#28440=CARTESIAN_POINT('',(-0.00910761536726419,0.0280621564475424,0.0855038929660693));
#28441=CARTESIAN_POINT('',(-0.00910761536726419,0.0303108891324553,0.0856361846327359));
#28442=CARTESIAN_POINT('',(-0.00910761536726419,0.0325596218173683,0.0857684762994026));
#28443=CARTESIAN_POINT('',(-0.0102319817097207,0.0345070814488233,0.0859007679660692));
#28444=CARTESIAN_POINT('',(-0.0113563480521771,0.0364545410802783,0.0860330596327359));
#28445=CARTESIAN_POINT('',(-0.0133038076836321,0.0375789074227348,0.0861653512994025));
#28446=CARTESIAN_POINT('',(-0.0152512673150871,0.0387032737651912,0.0862976429660692));
#28447=CARTESIAN_POINT('',(-0.0175,0.0387032737651912,0.0864299346327359));
#28448=CARTESIAN_POINT('',(-0.019748732684913,0.0387032737651912,0.0865622262994026));
#28449=CARTESIAN_POINT('',(-0.021696192316368,0.0375789074227348,0.0866945179660692));
#28450=CARTESIAN_POINT('',(-0.023643651947823,0.0364545410802783,0.0868268096327359));
#28451=CARTESIAN_POINT('',(-0.0247680182902794,0.0345070814488233,0.0869591012994025));
#28452=CARTESIAN_POINT('',(-0.0258923846327359,0.0325596218173683,0.0870913929660692));
#28453=CARTESIAN_POINT('',(-0.0258923846327359,0.0303108891324553,0.0872236846327359));
#28454=CARTESIAN_POINT('',(-0.0258923846327359,0.0280621564475424,0.0873559762994026));
#28455=CARTESIAN_POINT('',(-0.0247680182902794,0.0261146968160874,0.0874882679660692));
#28456=CARTESIAN_POINT('',(-0.023643651947823,0.0241672371846324,0.0876205596327359));
#28457=CARTESIAN_POINT('',(-0.021696192316368,0.023042870842176,0.0877528512994025));
#28458=CARTESIAN_POINT('',(-0.019748732684913,0.0219185044997195,0.0878851429660692));
#28459=CARTESIAN_POINT('',(-0.0175,0.0219185044997195,0.0880174346327359));
#28460=CARTESIAN_POINT('',(-0.0152512673150871,0.0219185044997195,0.0881497262994026));
#28461=CARTESIAN_POINT('',(-0.0133038076836321,0.023042870842176,0.0882820179660692));
#28462=CARTESIAN_POINT('',(-0.0113563480521771,0.0241672371846324,0.0884143096327359));
#28463=CARTESIAN_POINT('',(-0.0102319817097207,0.0261146968160874,0.0885466012994025));
#28464=CARTESIAN_POINT('',(-0.00910761536726419,0.0280621564475424,0.0886788929660693));
#28465=CARTESIAN_POINT('',(-0.00910761536726419,0.0303108891324553,0.0888111846327359));
#28466=CARTESIAN_POINT('',(-0.00910761536726419,0.0325596218173683,0.0889434762994026));
#28467=CARTESIAN_POINT('',(-0.0102319817097207,0.0345070814488233,0.0890757679660692));
#28468=CARTESIAN_POINT('',(-0.0113563480521771,0.0364545410802783,0.0892080596327359));
#28469=CARTESIAN_POINT('',(-0.0133038076836321,0.0375789074227348,0.0893403512994025));
#28470=CARTESIAN_POINT('',(-0.0152512673150871,0.0387032737651912,0.0894726429660692));
#28471=CARTESIAN_POINT('',(-0.0175,0.0387032737651912,0.0896049346327359));
#28472=CARTESIAN_POINT('',(-0.019748732684913,0.0387032737651912,0.0897372262994026));
#28473=CARTESIAN_POINT('',(-0.021696192316368,0.0375789074227348,0.0898695179660692));
#28474=CARTESIAN_POINT('',(-0.023643651947823,0.0364545410802783,0.0900018096327359));
#28475=CARTESIAN_POINT('',(-0.0247680182902794,0.0345070814488233,0.0901341012994025));
#28476=CARTESIAN_POINT('',(-0.0258923846327359,0.0325596218173683,0.0902663929660692));
#28477=CARTESIAN_POINT('',(-0.0258923846327359,0.0303108891324553,0.0903986846327359));
#28478=CARTESIAN_POINT('',(-0.0093308,0.0303108891324553,0.083));
#28479=CARTESIAN_POINT('',(-0.00933080000000005,0.0324998196752637,0.0831322916666668));
#28480=CARTESIAN_POINT('',(-0.0104252652714042,0.0343954891324554,0.0832645833333334));
#28481=CARTESIAN_POINT('',(-0.0115197305428084,0.036291158589647,0.0833968750000001));
#28482=CARTESIAN_POINT('',(-0.0134154,0.0373856238610512,0.0835291666666667));
#28483=CARTESIAN_POINT('',(-0.0153110694571917,0.0384800891324553,0.0836614583333334));
#28484=CARTESIAN_POINT('',(-0.0175,0.0384800891324554,0.08379375));
#28485=CARTESIAN_POINT('',(-0.0196889305428084,0.0384800891324553,0.0839260416666667));
#28486=CARTESIAN_POINT('',(-0.0215846,0.0373856238610512,0.0840583333333334));
#28487=CARTESIAN_POINT('',(-0.0234802694571917,0.036291158589647,0.084190625));
#28488=CARTESIAN_POINT('',(-0.0245747347285959,0.0343954891324554,0.0843229166666667));
#28489=CARTESIAN_POINT('',(-0.0256692000000001,0.0324998196752636,0.0844552083333334));
#28490=CARTESIAN_POINT('',(-0.0256692,0.0303108891324553,0.0845875));
#28491=CARTESIAN_POINT('',(-0.0093308,0.0303108891324553,0.083));
#28492=CARTESIAN_POINT('',(-0.0256692,0.0303108891324553,0.0845875));
#28493=CARTESIAN_POINT('',(-0.0093308,0.0303108891324553,0.083));
#28494=CARTESIAN_POINT('',(-0.00933080000000005,0.0317860674431147,0.083));
#28495=CARTESIAN_POINT('',(-0.0101154411361515,0.0347108515037046,0.0830000000000001));
#28496=CARTESIAN_POINT('',(-0.012199646341259,0.0368722439921494,0.083));
#28497=CARTESIAN_POINT('',(-0.0134462729974218,0.0376593187070208,0.083));
#28498=CARTESIAN_POINT('',(-0.0264312,0.0303108891324553,0.0909375));
#28499=CARTESIAN_POINT('',(-0.0256692,0.0303108891324553,0.0909375));
#28500=CARTESIAN_POINT('',(-0.0093308,0.0303108891324553,0.08935));
#28501=CARTESIAN_POINT('',(-0.00933080000000003,0.0324998196752637,0.0894822916666667));
#28502=CARTESIAN_POINT('',(-0.0104252652714042,0.0343954891324554,0.0896145833333333));
#28503=CARTESIAN_POINT('',(-0.0115197305428084,0.036291158589647,0.0897468750000001));
#28504=CARTESIAN_POINT('',(-0.0134154,0.0373856238610512,0.0898791666666667));
#28505=CARTESIAN_POINT('',(-0.0153110694571917,0.0384800891324553,0.0900114583333334));
#28506=CARTESIAN_POINT('',(-0.0175,0.0384800891324554,0.09014375));
#28507=CARTESIAN_POINT('',(-0.0196889305428084,0.0384800891324553,0.0902760416666667));
#28508=CARTESIAN_POINT('',(-0.0215846,0.0373856238610512,0.0904083333333334));
#28509=CARTESIAN_POINT('',(-0.0234802694571917,0.036291158589647,0.0905406250000001));
#28510=CARTESIAN_POINT('',(-0.0245747347285959,0.0343954891324554,0.0906729166666667));
#28511=CARTESIAN_POINT('',(-0.0256692000000001,0.0324998196752637,0.0908052083333334));
#28512=CARTESIAN_POINT('',(-0.0256692,0.0303108891324553,0.0909375));
#28513=CARTESIAN_POINT('',(-0.0093308,0.0303108891324553,0.08935));
#28514=CARTESIAN_POINT('',(-0.0256692,0.0303108891324553,0.0877625));
#28515=CARTESIAN_POINT('',(-0.0256692,0.028121958589647,0.0878947916666667));
#28516=CARTESIAN_POINT('',(-0.0245747347285959,0.0262262891324554,0.0880270833333334));
#28517=CARTESIAN_POINT('',(-0.0234802694571917,0.0243306196752637,0.088159375));
#28518=CARTESIAN_POINT('',(-0.0215846,0.0232361544038595,0.0882916666666667));
#28519=CARTESIAN_POINT('',(-0.0196889305428084,0.0221416891324553,0.0884239583333334));
#28520=CARTESIAN_POINT('',(-0.0175,0.0221416891324554,0.08855625));
#28521=CARTESIAN_POINT('',(-0.0153110694571917,0.0221416891324553,0.0886885416666667));
#28522=CARTESIAN_POINT('',(-0.0134154,0.0232361544038595,0.0888208333333334));
#28523=CARTESIAN_POINT('',(-0.0115197305428084,0.0243306196752637,0.088953125));
#28524=CARTESIAN_POINT('',(-0.0104252652714042,0.0262262891324554,0.0890854166666667));
#28525=CARTESIAN_POINT('',(-0.00933080000000006,0.028121958589647,0.0892177083333334));
#28526=CARTESIAN_POINT('',(-0.0093308,0.0303108891324553,0.08935));
#28527=CARTESIAN_POINT('',(-0.0256692,0.0303108891324553,0.0877625));
#28528=CARTESIAN_POINT('',(-0.0093308,0.0303108891324553,0.086175));
#28529=CARTESIAN_POINT('',(-0.00933080000000004,0.0324998196752637,0.0863072916666667));
#28530=CARTESIAN_POINT('',(-0.0104252652714042,0.0343954891324554,0.0864395833333334));
#28531=CARTESIAN_POINT('',(-0.0115197305428084,0.036291158589647,0.086571875));
#28532=CARTESIAN_POINT('',(-0.0134154,0.0373856238610512,0.0867041666666667));
#28533=CARTESIAN_POINT('',(-0.0153110694571917,0.0384800891324553,0.0868364583333334));
#28534=CARTESIAN_POINT('',(-0.0175,0.0384800891324554,0.08696875));
#28535=CARTESIAN_POINT('',(-0.0196889305428084,0.0384800891324553,0.0871010416666667));
#28536=CARTESIAN_POINT('',(-0.0215846,0.0373856238610512,0.0872333333333334));
#28537=CARTESIAN_POINT('',(-0.0234802694571917,0.036291158589647,0.087365625));
#28538=CARTESIAN_POINT('',(-0.0245747347285959,0.0343954891324554,0.0874979166666667));
#28539=CARTESIAN_POINT('',(-0.0256692000000001,0.0324998196752637,0.0876302083333333));
#28540=CARTESIAN_POINT('',(-0.0256692,0.0303108891324553,0.0877625));
#28541=CARTESIAN_POINT('',(-0.0093308,0.0303108891324553,0.086175));
#28542=CARTESIAN_POINT('',(-0.0256692,0.0303108891324553,0.0845875));
#28543=CARTESIAN_POINT('',(-0.0256692,0.028121958589647,0.0847197916666667));
#28544=CARTESIAN_POINT('',(-0.0245747347285959,0.0262262891324554,0.0848520833333334));
#28545=CARTESIAN_POINT('',(-0.0234802694571917,0.0243306196752637,0.0849843750000001));
#28546=CARTESIAN_POINT('',(-0.0215846,0.0232361544038595,0.0851166666666667));
#28547=CARTESIAN_POINT('',(-0.0196889305428084,0.0221416891324553,0.0852489583333334));
#28548=CARTESIAN_POINT('',(-0.0175,0.0221416891324554,0.08538125));
#28549=CARTESIAN_POINT('',(-0.0153110694571917,0.0221416891324553,0.0855135416666667));
#28550=CARTESIAN_POINT('',(-0.0134154,0.0232361544038595,0.0856458333333334));
#28551=CARTESIAN_POINT('',(-0.0115197305428084,0.0243306196752637,0.0857781250000001));
#28552=CARTESIAN_POINT('',(-0.0104252652714042,0.0262262891324554,0.0859104166666667));
#28553=CARTESIAN_POINT('',(-0.00933080000000005,0.028121958589647,0.0860427083333333));
#28554=CARTESIAN_POINT('',(-0.0093308,0.0303108891324553,0.086175));
#28555=CARTESIAN_POINT('',(-0.0256835799347999,0.0303108891324553,0.0883593889197018));
#28556=CARTESIAN_POINT('',(-0.0256692,0.0303108891324553,0.093));
#28557=CARTESIAN_POINT('',(-0.0175,0.0303108891324553,0.083));
#28558=CARTESIAN_POINT('',(-0.0175,0.0303108891324553,0.083));
#28559=CARTESIAN_POINT('',(-0.0175,0.0303108891324553,0.093));
#28560=CARTESIAN_POINT('',(-0.0175,0.0303108891324553,0.093));
#28561=CARTESIAN_POINT('',(-0.0256692,0.0303108891324553,0.093));
#28562=CARTESIAN_POINT('',(-0.0175,0.0303108891324553,0.093));
#28563=CARTESIAN_POINT('',(-8.67361737988404E-19,0.,0.001));
#28564=CARTESIAN_POINT('',(-0.006,-4.18502038579405E-17,-0.0146355706936178));
#28565=CARTESIAN_POINT('',(-0.006,-4.18502038579405E-17,-0.0146355706936178));
#28566=CARTESIAN_POINT('',(-0.006,-2.43712308653931E-5,-0.0140410700265819));
#28567=CARTESIAN_POINT('',(-0.006,9.23323236123637E-16,0.00236442930638223));
#28568=CARTESIAN_POINT('',(-0.006,9.23323236123637E-16,0.00236442930638223));
#28569=CARTESIAN_POINT('',(-0.00599994287806969,-2.43712307521178E-5,0.00295892997067845));
#28570=CARTESIAN_POINT('',(-0.006,-2.43712308653931E-5,-0.0140410700265819));
#28571=CARTESIAN_POINT('',(-0.00600309747414711,0.000755994738560391,-0.0140090793492257));
#28572=CARTESIAN_POINT('',(-0.00585022549906422,0.00154554847924553,-0.0139767317091225));
#28573=CARTESIAN_POINT('',(-0.00488277416170381,0.00391156551240249,-0.0138719117580559));
#28574=CARTESIAN_POINT('',(-0.00345414811439852,0.00521522772168569,-0.0137995939835592));
#28575=CARTESIAN_POINT('',(-0.000920416913494161,0.00599387797088215,-0.0136909247186258));
#28576=CARTESIAN_POINT('',(-1.83364399790589E-5,0.00606458475875607,-0.0136547070017816));
#28577=CARTESIAN_POINT('',(0.00173071508355203,0.00581192078991974,-0.013582263622242));
#28578=CARTESIAN_POINT('',(0.00257620709021928,0.0054899026401681,-0.013546041378497));
#28579=CARTESIAN_POINT('',(0.0040496481570146,0.00451412616898593,-0.0134735982934369));
#28580=CARTESIAN_POINT('',(0.00467595743139725,0.00386119227478036,-0.0134373767382566));
#28581=CARTESIAN_POINT('',(0.00559115533267521,0.00234942868328478,-0.0133649337688717));
#28582=CARTESIAN_POINT('',(0.00587789190074464,0.00149118187026969,-0.013328711875432));
#28583=CARTESIAN_POINT('',(0.00605911477020831,-0.000266602851011457,-0.0132562691328768));
#28584=CARTESIAN_POINT('',(0.00595132195371268,-0.00116523586494131,-0.0132200472158988));
#28585=CARTESIAN_POINT('',(0.00536345211542811,-0.00283155473315956,-0.0131476043990316));
#28586=CARTESIAN_POINT('',(0.00488207572844726,-0.00359821831670739,-0.013111382654392));
#28587=CARTESIAN_POINT('',(0.00363763601600018,-0.00485255191712249,-0.0130389394867723));
#28588=CARTESIAN_POINT('',(0.00287504504636738,-0.00534029243914702,-0.0130027180351518));
#28589=CARTESIAN_POINT('',(0.00121351369399411,-0.00594156052931282,-0.0129302744931486));
#28590=CARTESIAN_POINT('',(0.000315825750312525,-0.00605668045304735,-0.0128940532261725));
#28591=CARTESIAN_POINT('',(-0.00144337707403964,-0.00588978902230696,-0.0128216096183549));
#28592=CARTESIAN_POINT('',(-0.00230387638883705,-0.00560996798125232,-0.012785388316591));
#28593=CARTESIAN_POINT('',(-0.00382310259116674,-0.00470721006652816,-0.0127129448611614));
#28594=CARTESIAN_POINT('',(-0.00448099997246373,-0.00408613400852397,-0.0126767233862572));
#28595=CARTESIAN_POINT('',(-0.0054688674143523,-0.00262077375144199,-0.0126042801976742));
#28596=CARTESIAN_POINT('',(-0.00579763556460296,-0.0017778661740937,-0.0125680585008892));
#28597=CARTESIAN_POINT('',(-0.00606464167597128,-3.0946622266283E-5,-0.0124956155817382));
#28598=CARTESIAN_POINT('',(-0.00600111463142179,0.00087169976698755,-0.012459393707512));
#28599=CARTESIAN_POINT('',(-0.00549586755061847,0.00256503164149849,-0.0123869509484387));
#28600=CARTESIAN_POINT('',(-0.0050523880893689,0.00335400980216192,-0.0123507290311181));
#28601=CARTESIAN_POINT('',(-0.00387159456299549,0.00466851979026504,-0.0122782862186558));
#28602=CARTESIAN_POINT('',(-0.00313347130157478,0.00519260976096335,-0.0122420644730658));
#28603=CARTESIAN_POINT('',(-0.00150374624037729,0.00587523641666246,-0.0121696213045038));
#28604=CARTESIAN_POINT('',(-0.000612553833171288,0.00603401898911306,-0.0121333998532844));
#28605=CARTESIAN_POINT('',(0.00115259631366971,0.00595367775238322,-0.012060956311437));
#28606=CARTESIAN_POINT('',(0.00202600631780663,0.00571650438740237,-0.0120247350443508));
#28607=CARTESIAN_POINT('',(0.00358743121515774,0.00488909903514313,-0.0119522914365147));
#28608=CARTESIAN_POINT('',(0.00427534604366821,0.00430127927179916,-0.0119160701347756));
#28609=CARTESIAN_POINT('',(0.00533345753982393,0.00288585701390729,-0.011843626679348));
#28610=CARTESIAN_POINT('',(0.00570359994722143,0.00206029112764935,-0.0118074052044376));
#28611=CARTESIAN_POINT('',(0.00605550136478055,0.000328434275013915,-0.0117349620158554));
#28612=CARTESIAN_POINT('',(0.00603667676489193,-0.000576124907669123,-0.0116987403190736));
#28613=CARTESIAN_POINT('',(0.00561484107606885,-0.00229224694171357,-0.0116262973999176));
#28614=CARTESIAN_POINT('',(0.00521072192138963,-0.00310187271837801,-0.0115900755256951));
#28615=CARTESIAN_POINT('',(0.0040959244307272,-0.0044729576919261,-0.0115176327666191));
#28616=CARTESIAN_POINT('',(0.0033842739627938,-0.00503216622374487,-0.0114814108492998));
#28617=CARTESIAN_POINT('',(0.00179032179752591,-0.00579474497744012,-0.0114089680368375));
#28618=CARTESIAN_POINT('',(0.000907824274980536,-0.0059964734313809,-0.0113727462912467));
#28619=CARTESIAN_POINT('',(-0.000859075264311106,-0.00600346944668868,-0.0113003031226866));
#28620=CARTESIAN_POINT('',(-0.00174319314868272,-0.00580912084620773,-0.0112640816714646));
#28621=CARTESIAN_POINT('',(-0.00334323398092842,-0.00505940150515071,-0.0111916381296202));
#28622=CARTESIAN_POINT('',(-0.0040593972898715,-0.00450604234934652,-0.0111554168625309));
#28623=CARTESIAN_POINT('',(-0.00518533147390755,-0.00314408804019317,-0.0110829732546983));
#28624=CARTESIAN_POINT('',(-0.00559593301943456,-0.00233775978428837,-0.0110467519529574));
#28625=CARTESIAN_POINT('',(-0.00603184192596513,-0.000625158391190649,-0.0109743084975298));
#28626=CARTESIAN_POINT('',(-0.00605787853325042,0.000279212400784205,-0.010938087022621));
#28627=CARTESIAN_POINT('',(-0.00572024012570424,0.00201390634250815,-0.0108656438340358));
#28628=CARTESIAN_POINT('',(-0.00535668865032753,0.00284240619482864,-0.0108294221372547));
#28629=CARTESIAN_POINT('',(-0.00431023182100595,0.00426646668808826,-0.0107569792181002));
#28630=CARTESIAN_POINT('',(-0.00362704403416047,0.0048598136669573,-0.0107207573438761));
#28631=CARTESIAN_POINT('',(-0.00207241394588092,0.00569991648120368,-0.0106483145848017));
#28632=CARTESIAN_POINT('',(-0.00120093480390402,0.00594422095445996,-0.0106120926674817));
#28633=CARTESIAN_POINT('',(0.000563511232301897,0.00603877277129276,-0.0105396498550195));
#28634=CARTESIAN_POINT('',(0.00145603076803849,0.00588742838004165,-0.01050342810943));
#28635=CARTESIAN_POINT('',(0.003091110347539,0.0052177286750386,-0.0104309849408669));
#28636=CARTESIAN_POINT('',(0.00383355477573361,0.00469983671428884,-0.0103947634896458));
#28637=CARTESIAN_POINT('',(0.00502489458107504,0.00339487724234225,-0.0103223199478029));
#28638=CARTESIAN_POINT('',(0.00547478182306626,0.00260957621096752,-0.0102860986807135));
#28639=CARTESIAN_POINT('',(0.00599381202091714,0.000920418142363337,-0.0102136550728794));
#28640=CARTESIAN_POINT('',(0.00606458992024415,1.83375614756708E-5,-0.0101774337711432));
#28641=CARTESIAN_POINT('',(0.00581193305766793,-0.00173071492951537,-0.0101049903157079));
#28642=CARTESIAN_POINT('',(0.00548990002742215,-0.00257620837226416,-0.0100687688408028));
#28643=CARTESIAN_POINT('',(0.00451412418157153,-0.00404964797549366,-0.00999632565221761));
#28644=CARTESIAN_POINT('',(0.00386119324725615,-0.00467595690529434,-0.00996010395543582));
#28645=CARTESIAN_POINT('',(0.00234942884354364,-0.00559115555682603,-0.00988766103628286));
#28646=CARTESIAN_POINT('',(0.00149118157195093,-0.00587789203903946,-0.00985143916205724));
#28647=CARTESIAN_POINT('',(-0.000266602775728381,-0.00605911465611149,-0.00977899640298428));
#28648=CARTESIAN_POINT('',(-0.00116523579238055,-0.00595132192935385,-0.00974277448566356));
#28649=CARTESIAN_POINT('',(-0.0028315547852557,-0.00536345215233157,-0.00967033167320129));
#28650=CARTESIAN_POINT('',(-0.00359821832558892,-0.00488207572751732,-0.00963410992760799));
#28651=CARTESIAN_POINT('',(-0.00485255190132513,-0.00363763601143704,-0.00956166675905256));
#28652=CARTESIAN_POINT('',(-0.00534029243944068,-0.00287504504673827,-0.00952544530782837));
#28653=CARTESIAN_POINT('',(-0.00594156053203977,-0.00121351369403066,-0.00945300176598398));
#28654=CARTESIAN_POINT('',(-0.00605668045273713,-0.000315825750337319,-0.00941678049889378));
#28655=CARTESIAN_POINT('',(-0.00588978902176606,0.00144337707403134,-0.00934433689106272));
#28656=CARTESIAN_POINT('',(-0.00560996798134601,0.00230387638883739,-0.0093081155893231));
#28657=CARTESIAN_POINT('',(-0.00470721006664119,0.00382310259118043,-0.00923567213389156));
#28658=CARTESIAN_POINT('',(-0.00408613400847974,0.00448099997245,-0.00919945065898276));
#28659=CARTESIAN_POINT('',(-0.0026207737514388,0.00546886741436465,-0.00912700747040132));
#28660=CARTESIAN_POINT('',(-0.00177786617410126,0.00579763556459996,-0.00909078577361959));
#28661=CARTESIAN_POINT('',(-3.09466222681958E-5,0.00606464167597443,-0.00901834285446272));
#28662=CARTESIAN_POINT('',(0.000871699766989816,0.00600111463142254,-0.00898212098023906));
#28663=CARTESIAN_POINT('',(0.00256503164149829,0.00549586755061753,-0.0089096782211661));
#28664=CARTESIAN_POINT('',(0.00335400980216468,0.00505238808937253,-0.00887345630384614));
#28665=CARTESIAN_POINT('',(0.00466851979026242,0.00387159456299146,-0.00880101349138235));
#28666=CARTESIAN_POINT('',(0.00519260976097037,0.0031334713015793,-0.00876479174579288));
#28667=CARTESIAN_POINT('',(0.00587523641665553,0.00150374624037253,-0.00869234857723131));
#28668=CARTESIAN_POINT('',(0.0060340189891069,0.000612553833172357,-0.00865612712601019));
#28669=CARTESIAN_POINT('',(0.00595367775238934,-0.00115259631367031,-0.00858368358416579));
#28670=CARTESIAN_POINT('',(0.0057165043874037,-0.00202600631780788,-0.00854746231707637));
#28671=CARTESIAN_POINT('',(0.00488909903514167,-0.00358743121515669,-0.00847501870924377));
#28672=CARTESIAN_POINT('',(0.00430127927179329,-0.00427534604365617,-0.00843879740750493));
#28673=CARTESIAN_POINT('',(0.00288585701391485,-0.00533345753983467,-0.00836635395207338));
#28674=CARTESIAN_POINT('',(0.0020602911276489,-0.00570359994720765,-0.00833013247716457));
#28675=CARTESIAN_POINT('',(0.000328434275016982,-0.00605550136479379,-0.00825768928858313));
#28676=CARTESIAN_POINT('',(-0.000576124907666656,-0.00603667676488749,-0.00822146759180141));
#28677=CARTESIAN_POINT('',(-0.00229224694171241,-0.00561484107607418,-0.00814902467264454));
#28678=CARTESIAN_POINT('',(-0.00310187271838032,-0.00521072192139484,-0.00811280279842165));
#28679=CARTESIAN_POINT('',(-0.004472957691924,-0.00409592443072183,-0.00804036003934715));
#28680=CARTESIAN_POINT('',(-0.00503216622374263,-0.00338427396279622,-0.00800413812202796));
#28681=CARTESIAN_POINT('',(-0.00579474497744008,-0.00179032179752817,-0.00793169530956417));
#28682=CARTESIAN_POINT('',(-0.00599647343138397,-0.000907824274979786,-0.00789547356397393));
#28683=CARTESIAN_POINT('',(-0.00600346944668562,0.000859075264311016,-0.00782303039541389));
#28684=CARTESIAN_POINT('',(-0.00580912084621274,0.0017431931486827,-0.00778680894419278));
#28685=CARTESIAN_POINT('',(-0.00505940150514794,0.00334323398092366,-0.00771436540234685));
#28686=CARTESIAN_POINT('',(-0.00450604234934851,0.00405939728987541,-0.00767814413525819));
#28687=CARTESIAN_POINT('',(-0.00314408804019073,0.00518533147390397,-0.00760570052742559));
#28688=CARTESIAN_POINT('',(-0.00233775978429126,0.00559593301943496,-0.00756947922568675));
#28689=CARTESIAN_POINT('',(-0.000625158391191966,0.00603184192596372,-0.00749703577025521));
#28690=CARTESIAN_POINT('',(0.000279212400785439,0.00605787853325739,-0.0074608142953487));
#28691=CARTESIAN_POINT('',(0.00201390634250682,0.0057202401256973,-0.00738837110676266));
#28692=CARTESIAN_POINT('',(0.00284240619482905,0.00535668865032929,-0.0073521494099817));
#28693=CARTESIAN_POINT('',(0.00426646668808612,0.00431023182100547,-0.0072797064908279));
#28694=CARTESIAN_POINT('',(0.00485981366694846,0.00362704403415547,-0.00724348461660347));
#28695=CARTESIAN_POINT('',(0.00569991648121184,0.00207241394588719,-0.00717104185752897));
#28696=CARTESIAN_POINT('',(0.00594422095445765,0.00120093480390459,-0.00713481994020902));
#28697=CARTESIAN_POINT('',(0.00603877277129507,-0.00056351123230199,-0.00706237712774675));
#28698=CARTESIAN_POINT('',(0.0058874283800451,-0.00145603076804085,-0.0070261553821569));
#28699=CARTESIAN_POINT('',(0.00521772867503515,-0.00309111034753677,-0.00695371221359457));
#28700=CARTESIAN_POINT('',(0.00469983671428812,-0.00383355477573512,-0.006917490762375));
#28701=CARTESIAN_POINT('',(0.00339487724234326,-0.00502489458107331,-0.00684504722052831));
#28702=CARTESIAN_POINT('',(0.00260957621096805,-0.00547478182307112,-0.00680882595343965));
#28703=CARTESIAN_POINT('',(0.00092041814236392,-0.00599381202091195,-0.00673638234560783));
#28704=CARTESIAN_POINT('',(1.83375614742641E-5,-0.00606458992025192,-0.00670016104386784));
#28705=CARTESIAN_POINT('',(-0.00173071492951204,-0.00581193305766056,-0.00662771758843784));
#28706=CARTESIAN_POINT('',(-0.00257620837226887,-0.00548990002742911,-0.00659149611352898));
#28707=CARTESIAN_POINT('',(-0.00404964797548944,-0.00451412418156432,-0.00651905292494602));
#28708=CARTESIAN_POINT('',(-0.00467595690530402,-0.00386119324726373,-0.00648283122816474));
#28709=CARTESIAN_POINT('',(-0.00559115555681467,-0.002349428843539,-0.00641038830900865));
#28710=CARTESIAN_POINT('',(-0.00587789203904983,-0.00149118157195279,-0.00637416643478492));
#28711=CARTESIAN_POINT('',(-0.00605911465610112,0.000266602775729709,-0.0063017236757112));
#28712=CARTESIAN_POINT('',(-0.0059513219293497,0.00116523579237788,-0.00626550175839094));
#28713=CARTESIAN_POINT('',(-0.00536345215233749,0.00283155478525354,-0.00619305894592869));
#28714=CARTESIAN_POINT('',(-0.0048820757275079,0.00359821832558035,-0.00615683720033756));
#28715=CARTESIAN_POINT('',(-0.00363763601144603,0.0048525519013342,-0.00608439403177752));
#28716=CARTESIAN_POINT('',(-0.00287504504674204,0.00534029243944514,-0.00604817258055424));
#28717=CARTESIAN_POINT('',(-0.00121351369403187,0.00594156053203358,-0.0059757290387129));
#28718=CARTESIAN_POINT('',(-0.00031582575033843,0.00605668045273254,-0.00593950777162106));
#28719=CARTESIAN_POINT('',(0.00144337707403289,0.00588978902177064,-0.00586706416378998));
#28720=CARTESIAN_POINT('',(0.00230387638884796,0.00560996798136351,-0.00583084286204893));
#28721=CARTESIAN_POINT('',(0.00382310259116669,0.00470721006662557,-0.00575839940662044));
#28722=CARTESIAN_POINT('',(0.00448099997245725,0.00408613400848599,-0.0057221779317101));
#28723=CARTESIAN_POINT('',(0.00546886741435594,0.00262077375143485,-0.00564973474312865));
#28724=CARTESIAN_POINT('',(0.00579763556459787,0.00177786617410278,-0.00561351304634461));
#28725=CARTESIAN_POINT('',(0.00606464167597621,3.0946622268693E-5,-0.00554107012719234));
#28726=CARTESIAN_POINT('',(0.00600111463141991,-0.000871699766989554,-0.0055048482529664));
#28727=CARTESIAN_POINT('',(0.00549586755062006,-0.00256503164149915,-0.0054324054938933));
#28728=CARTESIAN_POINT('',(0.00505238808936695,-0.00335400980216068,-0.00539618357657267));
#28729=CARTESIAN_POINT('',(0.00387159456299719,-0.00466851979026632,-0.00532374076411039));
#28730=CARTESIAN_POINT('',(0.00313347130158231,-0.00519260976097808,-0.00528751901851862));
#28731=CARTESIAN_POINT('',(0.00150374624036927,-0.00587523641664796,-0.00521507584996011));
#28732=CARTESIAN_POINT('',(0.000612553833171035,-0.00603401898911497,-0.00517885439873749));
#28733=CARTESIAN_POINT('',(-0.00115259631366817,-0.00595367775238131,-0.0051064108568931));
#28734=CARTESIAN_POINT('',(-0.00202600631781078,-0.00571650438740787,-0.00507018958980372));
#28735=CARTESIAN_POINT('',(-0.00358743121515375,-0.00488909903513752,-0.00499774598197099));
#28736=CARTESIAN_POINT('',(-0.00427534604366103,-0.00430127927179586,-0.00496152468023219));
#28737=CARTESIAN_POINT('',(-0.00533345753983033,-0.00288585701391166,-0.00488908122480065));
#28738=CARTESIAN_POINT('',(-0.00570359994720922,-0.00206029112764941,-0.00485285974989415));
#28739=CARTESIAN_POINT('',(-0.00605550136479229,-0.000328434275016135,-0.00478041656130811));
#28740=CARTESIAN_POINT('',(-0.00603667676488204,0.000576124907666373,-0.00474419486452637));
#28741=CARTESIAN_POINT('',(-0.00561484107607947,0.00229224694171347,-0.00467175194537411));
#28742=CARTESIAN_POINT('',(-0.00521072192140026,0.00310187271838521,-0.00463553007114899));
#28743=CARTESIAN_POINT('',(-0.00409592443071614,0.00447295769191944,-0.00456308731207436));
#28744=CARTESIAN_POINT('',(-0.00338427396279826,0.00503216622374612,-0.00452686539475448));
#28745=CARTESIAN_POINT('',(-0.00179032179752601,0.00579474497743666,-0.00445442258229221));
#28746=CARTESIAN_POINT('',(-0.000907824274979335,0.0059964734313974,-0.00441820083669967));
#28747=CARTESIAN_POINT('',(0.00085907526431096,0.00600346944667221,-0.0043457576681427));
#28748=CARTESIAN_POINT('',(0.00174319314868342,0.00580912084621372,-0.00430953621691928));
#28749=CARTESIAN_POINT('',(0.00334323398092361,0.00505940150514661,-0.00423709267507489));
#28750=CARTESIAN_POINT('',(0.00405939728986873,0.00450604234934388,-0.00420087140798552));
#28751=CARTESIAN_POINT('',(0.00518533147391094,0.00314408804019501,-0.00412842780015279));
#28752=CARTESIAN_POINT('',(0.00559593301943005,0.00233775978429005,-0.00409220649841479));
#28753=CARTESIAN_POINT('',(0.00603184192596878,0.000625158391192479,-0.00401976304298171));
#28754=CARTESIAN_POINT('',(0.00605787853326322,-0.000279212400785085,-0.00398354156807523));
#28755=CARTESIAN_POINT('',(0.00572024012569162,-0.00201390634250648,-0.00391109837949073));
#28756=CARTESIAN_POINT('',(0.00535668865032563,-0.00284240619482649,-0.0038748766827105));
#28757=CARTESIAN_POINT('',(0.00431023182100872,-0.0042664666880893,-0.00380243376355363));
#28758=CARTESIAN_POINT('',(0.00362704403415923,-0.00485981366695353,-0.00376621188933157));
#28759=CARTESIAN_POINT('',(0.00207241394588276,-0.00569991648120711,-0.0036937691302554));
#28760=CARTESIAN_POINT('',(0.00120093480390449,-0.00594422095445802,-0.00365754721293706));
#28761=CARTESIAN_POINT('',(-0.000563511232301889,-0.00603877277129467,-0.00358510440047326));
#28762=CARTESIAN_POINT('',(-0.00145603076803988,-0.00588742838004119,-0.00354888265488379));
#28763=CARTESIAN_POINT('',(-0.00309111034753821,-0.00521772867503886,-0.00347643948632222));
#28764=CARTESIAN_POINT('',(-0.00383355477573305,-0.00469983671428823,-0.00344021803510188));
#28765=CARTESIAN_POINT('',(-0.005024894581076,-0.00339487724234243,-0.00336777449325594));
#28766=CARTESIAN_POINT('',(-0.00547478182306962,-0.00260957621096737,-0.00333155322616581));
#28767=CARTESIAN_POINT('',(-0.00599381202091404,-0.000920418142362637,-0.00325910961833615));
#28768=CARTESIAN_POINT('',(-0.00606458992025173,-1.83375614733508E-5,-0.00322288831659661));
#28769=CARTESIAN_POINT('',(-0.00581193305766033,0.00173071492951357,-0.00315044486116353));
#28770=CARTESIAN_POINT('',(-0.00548990002742595,0.00257620837226724,-0.00311422338625548));
#28771=CARTESIAN_POINT('',(-0.00451412418156716,0.00404964797549147,-0.00304178019767404));
#28772=CARTESIAN_POINT('',(-0.00386119324726109,0.00467595690530463,-0.00300555850089079));
#28773=CARTESIAN_POINT('',(-0.00234942884353807,0.00559115555681618,-0.00293311558173699));
#28774=CARTESIAN_POINT('',(-0.00149118157195182,0.00587789203904661,-0.00289689370751264));
#28775=CARTESIAN_POINT('',(0.000266602775729427,0.0060591146561044,-0.00282445094843801));
#28776=CARTESIAN_POINT('',(0.00116523579237932,0.00595132192934975,-0.00278822903111813));
#28777=CARTESIAN_POINT('',(0.00283155478525638,0.00536345215233592,-0.00271578621865587));
#28778=CARTESIAN_POINT('',(0.00359821832558002,0.00488207572750747,-0.00267956447306408));
#28779=CARTESIAN_POINT('',(0.00485255190133472,0.00363763601144627,-0.00260712130450557));
#28780=CARTESIAN_POINT('',(0.00534029243944329,0.0028750450467383,-0.00257089985328367));
#28781=CARTESIAN_POINT('',(0.00594156053203786,0.00121351369402893,-0.00249845631143773));
#28782=CARTESIAN_POINT('',(0.00605668045272946,0.00031582575033894,-0.00246223504434917));
#28783=CARTESIAN_POINT('',(0.00588978902177369,-0.00144337707403387,-0.00238979143651642));
#28784=CARTESIAN_POINT('',(0.00560996798136092,-0.00230387638884949,-0.00235357013477837));
#28785=CARTESIAN_POINT('',(0.00470721006662452,-0.00382310259117127,-0.00228112667934528));
#28786=CARTESIAN_POINT('',(0.00408613400848635,-0.00448099997246406,-0.00224490520443801));
#28787=CARTESIAN_POINT('',(0.00262077375142909,-0.00546886741435278,-0.00217246201585504));
#28788=CARTESIAN_POINT('',(0.00177786617409953,-0.00579763556459878,-0.00213624031907329));
#28789=CARTESIAN_POINT('',(3.09466222649569E-5,-0.00606464167597636,-0.00206379739991795));
#28790=CARTESIAN_POINT('',(-0.000871699766989641,-0.00600111463142063,-0.00202757552569444));
#28791=CARTESIAN_POINT('',(-0.0025650316414994,-0.00549586755061925,-0.00195513276661981));
#28792=CARTESIAN_POINT('',(-0.00335400980216594,-0.0050523880893681,-0.00191891084930058));
#28793=CARTESIAN_POINT('',(-0.00466851979026617,-0.00387159456299146,-0.00184646803683676));
#28794=CARTESIAN_POINT('',(-0.00519260976097701,-0.00313347130158175,-0.0018102462912459));
#28795=CARTESIAN_POINT('',(-0.00587523641664912,-0.00150374624036962,-0.0017378031226874));
#28796=CARTESIAN_POINT('',(-0.00603401898911557,-0.00061255383316749,-0.00170158167146463));
#28797=CARTESIAN_POINT('',(-0.00595367775238039,0.00115259631367158,-0.00162913812962024));
#28798=CARTESIAN_POINT('',(-0.00571650438740898,0.00202600631781163,-0.00159291686253176));
#28799=CARTESIAN_POINT('',(-0.00488909903513646,0.00358743121515282,-0.00152047325469751));
#28800=CARTESIAN_POINT('',(-0.0043012792717929,0.0042753460436607,-0.00148425195295939));
#28801=CARTESIAN_POINT('',(-0.00288585701391163,0.00533345753983288,-0.00141180849752786));
#28802=CARTESIAN_POINT('',(-0.00206029112764908,0.00570359994721081,-0.00137558702261988));
#28803=CARTESIAN_POINT('',(-0.000328434275016096,0.00605550136479076,-0.00130314383403692));
#28804=CARTESIAN_POINT('',(0.000576124907667665,0.00603667676488167,-0.00126692213725589));
#28805=CARTESIAN_POINT('',(0.00229224694171486,0.00561484107607917,-0.00119447921809904));
#28806=CARTESIAN_POINT('',(0.00310187271838672,0.00521072192140026,-0.00115825734387622));
#28807=CARTESIAN_POINT('',(0.00447295769191957,0.00409592443071479,-0.00108581458480161));
#28808=CARTESIAN_POINT('',(0.00503216622374031,0.00338427396279337,-0.00104959266748173));
#28809=CARTESIAN_POINT('',(0.005794744977443,0.0017903217975298,-0.000977149855019475));
#28810=CARTESIAN_POINT('',(0.00599647343139357,0.000907824274979128,-0.000940928109428471));
#28811=CARTESIAN_POINT('',(0.00600346944667604,-0.000859075264311266,-0.000868484940868442));
#28812=CARTESIAN_POINT('',(0.00580912084621264,-0.0017431931486827,-0.0008322634896458));
#28813=CARTESIAN_POINT('',(0.00505940150514784,-0.00334323398092403,-0.000759819947802938));
#28814=CARTESIAN_POINT('',(0.00450604234934318,-0.00405939728986845,-0.000723598680712034));
#28815=CARTESIAN_POINT('',(0.00314408804019546,-0.00518533147391142,-0.000651155072880834));
#28816=CARTESIAN_POINT('',(0.00233775978428977,-0.00559593301942972,-0.000614933771140532));
#28817=CARTESIAN_POINT('',(0.000625158391192401,-0.00603184192596921,-0.000542490315710523));
#28818=CARTESIAN_POINT('',(-0.000279212400785806,-0.00605787853326039,-0.000506268840800958));
#28819=CARTESIAN_POINT('',(-0.00201390634250717,-0.00572024012569417,-0.000433825652219523));
#28820=CARTESIAN_POINT('',(-0.00284240619482663,-0.00535668865032544,-0.000397603955437035));
#28821=CARTESIAN_POINT('',(-0.00426646668808866,-0.0043102318210093,-0.000325161036281701));
#28822=CARTESIAN_POINT('',(-0.00485981366695287,-0.00362704403415734,-0.000288939162058086));
#28823=CARTESIAN_POINT('',(-0.00569991648120799,-0.00207241394588432,-0.000216496402983457));
#28824=CARTESIAN_POINT('',(-0.0059442209544565,-0.00120093480390377,-0.000180274485662048));
#28825=CARTESIAN_POINT('',(-0.00603877277129622,0.000563511232301556,-0.000107831673202851));
#28826=CARTESIAN_POINT('',(-0.00588742838004495,0.00145603076804102,-7.16099276087707E-5));
#28827=CARTESIAN_POINT('',(-0.00521772867503495,0.00309111034753743,8.33240948196383E-7));
#28828=CARTESIAN_POINT('',(-0.00469983671428809,0.00383355477573433,3.70546921731411E-5));
#28829=CARTESIAN_POINT('',(-0.00339487724234229,0.00502489458107499,0.000109498234014469));
#28830=CARTESIAN_POINT('',(-0.00260957621096751,0.00547478182307082,0.000145719501104603));
#28831=CARTESIAN_POINT('',(-0.000920418142362202,0.00599381202091294,0.000218163108938871));
#28832=CARTESIAN_POINT('',(-1.83375614725771E-5,0.00606458992025286,0.00025438441067611));
#28833=CARTESIAN_POINT('',(0.00173071492951319,0.00581193305765916,0.000326827866109187));
#28834=CARTESIAN_POINT('',(0.00257620837226795,0.00548990002742626,0.000363049341015702));
#28835=CARTESIAN_POINT('',(0.00404964797549103,0.0045141241815667,0.000435492529600207));
#28836=CARTESIAN_POINT('',(0.00467595690530011,0.00386119324726,0.000471714226381924));
#28837=CARTESIAN_POINT('',(0.00559115555682087,0.00234942884353889,0.000544157145535723));
#28838=CARTESIAN_POINT('',(0.00587789203904666,0.00149118157195146,0.000580379019759321));
#28839=CARTESIAN_POINT('',(0.00605911465610445,-0.000266602775729979,0.000652821778835484));
#28840=CARTESIAN_POINT('',(0.00595132192935104,-0.0011652357923806,0.000689043696154603));
#28841=CARTESIAN_POINT('',(0.00536345215233414,-0.0028315547852565,0.000761486508616866));
#28842=CARTESIAN_POINT('',(0.00488207572750542,-0.00359821832557824,0.000797708254208643));
#28843=CARTESIAN_POINT('',(0.00363763601144815,-0.00485255190133669,0.000870151422767143));
#28844=CARTESIAN_POINT('',(0.0028750450467372,-0.00534029243944135,0.000906372873988264));
#28845=CARTESIAN_POINT('',(0.00121351369403036,-0.00594156053203968,0.000978816415835729));
#28846=CARTESIAN_POINT('',(0.000315825750338376,-0.00605668045273214,0.00101503768292201));
#28847=CARTESIAN_POINT('',(-0.0014433770740335,-0.00588978902177103,0.00108748129075781));
#28848=CARTESIAN_POINT('',(-0.0023038763888485,-0.00560996798135989,0.00112370259249429));
#28849=CARTESIAN_POINT('',(-0.00382310259117005,-0.0047072100666267,0.00119614604792737));
#28850=CARTESIAN_POINT('',(-0.00448099997246035,-0.00408613400848585,0.00123236752283539));
#28851=CARTESIAN_POINT('',(-0.00546886741435506,-0.00262077375143265,0.00130481071141683));
#28852=CARTESIAN_POINT('',(-0.00579763556459847,-0.0017778661740996,0.00134103240820018));
#28853=CARTESIAN_POINT('',(-0.00606464167597601,-3.09466222654928E-5,0.00141347532735398));
#28854=CARTESIAN_POINT('',(-0.00600111463141992,0.000871699766980109,0.00144969720157956));
#28855=CARTESIAN_POINT('',(-0.00549586755062015,0.00256503164149748,0.00152213996065112));
#28856=CARTESIAN_POINT('',(-0.00505238808936944,0.00335400980220972,0.00155836187797583));
#28857=CARTESIAN_POINT('',(-0.00387159456298909,0.00466851979024306,0.00163080469043323));
#28858=CARTESIAN_POINT('',(-0.00313347130160139,0.00519260976081515,0.00166702643602028));
#28859=CARTESIAN_POINT('',(-0.00150374624037983,0.00587523641686614,0.00173946960459158));
#28860=CARTESIAN_POINT('',(-0.000612553833165579,0.00603401898939451,0.00177569105583878));
#28861=CARTESIAN_POINT('',(0.00115259631371467,0.0059536777513449,0.00184813459759908));
#28862=CARTESIAN_POINT('',(0.00202600631845691,0.00571650438746742,0.00188435586467389));
#28863=CARTESIAN_POINT('',(0.00358743121405334,0.00488909903965777,0.00195679947282889));
#28864=CARTESIAN_POINT('',(0.00427534604012664,0.00430127926719982,0.0019930207743065));
#28865=CARTESIAN_POINT('',(0.00533345754995747,0.00288585699514267,0.00206546422868242));
#28866=CARTESIAN_POINT('',(0.00570359995483104,0.0020602911659135,0.00210168570590789));
#28867=CARTESIAN_POINT('',(0.00605550130478085,0.000328434353748034,0.00217412889706531));
#28868=CARTESIAN_POINT('',(0.00603667678110669,-0.000576125165779344,0.00221035058020653));
#28869=CARTESIAN_POINT('',(0.0056148413322424,-0.00229224724916889,0.00228279349810771));
#28870=CARTESIAN_POINT('',(0.00521072173073282,-0.00310187120641182,0.00231901543922011));
#28871=CARTESIAN_POINT('',(0.00409592363987556,-0.00447295679573389,0.00239145815903209));
#28872=CARTESIAN_POINT('',(0.00338427466196768,-0.00503217385805823,0.00242767978760003));
#28873=CARTESIAN_POINT('',(0.00179032336308774,-0.00579474532206606,0.00250012295961856));
#28874=CARTESIAN_POINT('',(0.000907823357868306,-0.00599643245723689,0.00253634580897236));
#28875=CARTESIAN_POINT('',(-0.00154620346649854,-0.00600624349949343,0.00263695810271456));
#28876=CARTESIAN_POINT('',(-0.00311036825890238,-0.00536525626263524,0.00270138359384264));
#28877=CARTESIAN_POINT('',(-0.00534036428216497,-0.00315440800084661,0.00283011272614596));
#28878=CARTESIAN_POINT('',(-0.005993747924043,-0.00158510314530943,0.00289494802175126));
#28879=CARTESIAN_POINT('',(-0.00599994287806968,-2.43712307521179E-5,0.00295892997067846));
#28880=CARTESIAN_POINT('',(-0.00481,-2.43712308653838E-5,-0.0140410700265819));
#28881=CARTESIAN_POINT('',(-0.00481309747552789,0.0005972081498295,-0.0140093885644531));
#28882=CARTESIAN_POINT('',(-0.00468998407530162,0.00123726682455829,-0.0139764807930202));
#28883=CARTESIAN_POINT('',(-0.00391925933224434,0.00312747621252669,-0.013872784228301));
#28884=CARTESIAN_POINT('',(-0.0027740912685582,0.00417781018427425,-0.0137998290452317));
#28885=CARTESIAN_POINT('',(-0.000743052669427504,0.00480421623630904,-0.0136910345094936));
#28886=CARTESIAN_POINT('',(-2.09107523793298E-5,0.00486189283259464,-0.0136549080475063));
#28887=CARTESIAN_POINT('',(0.00138336308198147,0.00466047772833265,-0.0135822476417793));
#28888=CARTESIAN_POINT('',(0.00205983412778109,0.00440373135422188,-0.0135462440918831));
#28889=CARTESIAN_POINT('',(0.00324376540199818,0.00362139882094577,-0.0134735141781805));
#28890=CARTESIAN_POINT('',(0.00374510470485854,0.00309961711105746,-0.013437502604144));
#28891=CARTESIAN_POINT('',(0.00448098642623155,0.00188681812047127,-0.0133648332519321));
#28892=CARTESIAN_POINT('',(0.00471091204467595,0.00119985910905067,-0.0133287331669378));
#28893=CARTESIAN_POINT('',(0.00485766819906913,-0.000209707601454214,-0.013256221775084));
#28894=CARTESIAN_POINT('',(0.00477148103078713,-0.000930579595599502,-0.0132199460668666));
#28895=CARTESIAN_POINT('',(0.00430207967528991,-0.00226535979212377,-0.0131476977203435));
#28896=CARTESIAN_POINT('',(0.00391509509971101,-0.00288228528512647,-0.0131111635028226));
#28897=CARTESIAN_POINT('',(0.00292169918444729,-0.00388557413442109,-0.0130392727679438));
#28898=CARTESIAN_POINT('',(0.00230884595336562,-0.00427892221022316,-0.013002738946633));
#28899=CARTESIAN_POINT('',(0.000978852813182588,-0.00476172053905318,-0.0129304897411354));
#28900=CARTESIAN_POINT('',(0.000258925775658046,-0.00485523411194574,-0.0128942145009195));
#28901=CARTESIAN_POINT('',(-0.00115205885285439,-0.00472280803267504,-0.0128217027604969));
#28902=CARTESIAN_POINT('',(-0.00184127085788122,-0.00449979694527318,-0.0127856034436556));
#28903=CARTESIAN_POINT('',(-0.003061531144935,-0.00377635423162404,-0.0127129318637898));
#28904=CARTESIAN_POINT('',(-0.0035882725709729,-0.00328025220172361,-0.0126769213982539));
#28905=CARTESIAN_POINT('',(-0.00438269974044985,-0.0021043945145923,-0.0126041963336704));
#28906=CARTESIAN_POINT('',(-0.00464619750861001,-0.00143048448148469,-0.012568185646273));
#28907=CARTESIAN_POINT('',(-0.00486194590083409,-2.83941718657882E-5,-0.0124955146026973));
#28908=CARTESIAN_POINT('',(-0.00481148142262297,0.000694263094901001,-0.0124594147133711));
#28909=CARTESIAN_POINT('',(-0.00440764851959399,0.0020526935874246,-0.0123869038211612));
#28910=CARTESIAN_POINT('',(-0.00405215626122202,0.0026857101246237,-0.0123506279316278));
#28911=CARTESIAN_POINT('',(-0.00310768769660497,0.00373925423709306,-0.0122783794579231));
#28912=CARTESIAN_POINT('',(-0.00251407341947778,0.00416112641085721,-0.0122418453259864));
#28913=CARTESIAN_POINT('',(-0.00121235323067996,0.00470788827290766,-0.0121699545995431));
#28914=CARTESIAN_POINT('',(-0.000495622876170741,0.00483676574590065,-0.0121334207619492));
#28915=CARTESIAN_POINT('',(0.000917889479731042,0.00477384690220689,-0.0120611715589283));
#28916=CARTESIAN_POINT('',(0.00161880142913311,0.00458473802635917,-0.0120248963195875));
#28917=CARTESIAN_POINT('',(0.00287170398311334,0.0039224318405235,-0.0119523845786562));
#28918=CARTESIAN_POINT('',(0.00342311019952517,0.00345264644636138,-0.0119162852617685));
#28919=CARTESIAN_POINT('',(0.00427363416207398,0.00231729913548141,-0.0118436136819951));
#28920=CARTESIAN_POINT('',(0.00457042975696389,0.00165738540690319,-0.011807603216425));
#28921=CARTESIAN_POINT('',(0.00485440350323103,0.000267020440622511,-0.0117348781518639));
#28922=CARTESIAN_POINT('',(0.00483994949353749,-0.000456427476013854,-0.0116988674644479));
#28923=CARTESIAN_POINT('',(0.00450271828510177,-0.001834353351076,-0.0116261964208863));
#28924=CARTESIAN_POINT('',(0.00417954622328539,-0.00248268968912301,-0.0115900965315827));
#28925=CARTESIAN_POINT('',(0.00328660442614019,-0.00358317565608095,-0.0115175856393133));
#28926=CARTESIAN_POINT('',(0.00271592746345113,-0.00403196568092759,-0.0114813097498018));
#28927=CARTESIAN_POINT('',(0.00144017841039003,-0.00464388105095874,-0.0114090612761124));
#28928=CARTESIAN_POINT('',(0.000730306838075062,-0.00480647376857319,-0.0113725271441584));
#28929=CARTESIAN_POINT('',(-0.000681562507468831,-0.00481346911223833,-0.0113006364177347));
#28930=CARTESIAN_POINT('',(-0.00139305428604887,-0.00465825553959685,-0.0112641025801363));
#28931=CARTESIAN_POINT('',(-0.00267489142155627,-0.00405919834765848,-0.0111918533771047));
#28932=CARTESIAN_POINT('',(-0.00325008079200792,-0.00361625713726751,-0.0111555781377456));
#28933=CARTESIAN_POINT('',(-0.00415415821336922,-0.00252490095812974,-0.0110830663968616));
#28934=CARTESIAN_POINT('',(-0.00448381204370197,-0.00187986182427054,-0.011046967079966));
#28935=CARTESIAN_POINT('',(-0.00483511511877081,-0.000505456252163206,-0.0109742955001612));
#28936=CARTESIAN_POINT('',(-0.00485678044348491,0.000217803291852025,-0.0109382850346499));
#28937=CARTESIAN_POINT('',(-0.00458706833793583,0.00161100507485156,-0.0108655599700028));
#28938=CARTESIAN_POINT('',(-0.00429686304231609,0.00227385248782169,-0.0108295492826413));
#28939=CARTESIAN_POINT('',(-0.00345799262771523,0.00341783720477129,-0.0107568782390567));
#28940=CARTESIAN_POINT('',(-0.00291131299915783,0.00389314928382754,-0.0107207783497292));
#28941=CARTESIAN_POINT('',(-0.00166520460192398,0.0045681517126536,-0.0106482674575304));
#28942=CARTESIAN_POINT('',(-0.000966223329313709,0.004764391012167,-0.0106119915679807));
#28943=CARTESIAN_POINT('',(0.000446584983549955,0.00484151907170173,-0.0105397430942975));
#28944=CARTESIAN_POINT('',(0.00116464233918176,0.00472007906581758,-0.0105032089623268));
#28945=CARTESIAN_POINT('',(0.00247171653223062,0.00418624291343643,-0.01043131823593));
#28946=CARTESIAN_POINT('',(0.0030696515612859,0.00377056815459063,-0.0103947843983099));
#28947=CARTESIAN_POINT('',(0.00402466539239388,0.00272657364139763,-0.0103225351952951));
#28948=CARTESIAN_POINT('',(0.00438656481634017,0.00209723388046881,-0.0102862599559436));
#28949=CARTESIAN_POINT('',(0.00480417951319281,0.000742976793155331,-0.0102137482150274));
#28950=CARTESIAN_POINT('',(0.0048618941500755,2.0885280433355E-5,-0.0101776488981767));
#28951=CARTESIAN_POINT('',(0.00466049362906918,-0.00138333776357924,-0.0101049773183144));
#28952=CARTESIAN_POINT('',(0.00440373033433314,-0.00205983341381495,-0.010068966852824));
#28953=CARTESIAN_POINT('',(0.00362139360004503,-0.0032437696714788,-0.00999624178819235));
#28954=CARTESIAN_POINT('',(0.00309961814406215,-0.00374510407087602,-0.00996023110084268));
#28955=CARTESIAN_POINT('',(0.00188681893954217,-0.00448098632681852,-0.009887560057219));
#28956=CARTESIAN_POINT('',(0.00119985876200896,-0.00471091219153308,-0.00985146016793407));
#28957=CARTESIAN_POINT('',(-0.000209707527798131,-0.00485766808139427,-0.00977894927568926));
#28958=CARTESIAN_POINT('',(-0.000930579547875865,-0.00477148100111361,-0.00974267338616599));
#28959=CARTESIAN_POINT('',(-0.00226535986204974,-0.00430207970226204,-0.00967042491247586));
#28960=CARTESIAN_POINT('',(-0.00288228527781962,-0.00391509511292238,-0.00963389078046685));
#28961=CARTESIAN_POINT('',(-0.00388557412111365,-0.00292169917944251,-0.00956200005415361));
#28962=CARTESIAN_POINT('',(-0.00427892221277846,-0.00230884594832664,-0.00952546621648906));
#28963=CARTESIAN_POINT('',(-0.00476172054092556,-0.000978852814690387,-0.00945321701347969));
#28964=CARTESIAN_POINT('',(-0.00485523411171129,-0.000258925776843735,-0.00941694177410321));
#28965=CARTESIAN_POINT('',(-0.0047228080321108,0.00115205885347806,-0.00934443003323146));
#28966=CARTESIAN_POINT('',(-0.00449979694528425,0.00184127085801928,-0.00930833071637539));
#28967=CARTESIAN_POINT('',(-0.00377635423181849,0.00306153114481296,-0.00923565913647926));
#28968=CARTESIAN_POINT('',(-0.00328025220168744,0.00358827257095472,-0.00919964867101474));
#28969=CARTESIAN_POINT('',(-0.00210439451456859,0.00438269974047501,-0.00912692360636535));
#28970=CARTESIAN_POINT('',(-0.00143048448149271,0.00464619750860692,-0.0090909129190107));
#28971=CARTESIAN_POINT('',(-2.83941718690916E-5,0.00486194590083703,-0.00901824187541456));
#28972=CARTESIAN_POINT('',(0.000694263094903329,0.00481148142262362,-0.00898214198609713));
#28973=CARTESIAN_POINT('',(0.00205269358742323,0.00440764851959351,-0.00890963109388991));
#28974=CARTESIAN_POINT('',(0.00268571012462705,0.00405215626122519,-0.00887335520434781));
#28975=CARTESIAN_POINT('',(0.00373925423709026,0.00310768769660104,-0.00880110673065769));
#28976=CARTESIAN_POINT('',(0.00416112641086552,0.0025140734194825,-0.00876457259869544));
#28977=CARTESIAN_POINT('',(0.00470788827289936,0.00121235323067521,-0.00869268187228864));
#28978=CARTESIAN_POINT('',(0.00483676574589448,0.000495622876171375,-0.00865614803468577));
#28979=CARTESIAN_POINT('',(0.00477384690221301,-0.00091788947973133,-0.00858389883164647));
#28980=CARTESIAN_POINT('',(0.00458473802636119,-0.00161880142913334,-0.00854762359231106));
#28981=CARTESIAN_POINT('',(0.00392243184052137,-0.00287170398311328,-0.00847511185138717));
#28982=CARTESIAN_POINT('',(0.00345264644635509,-0.00342311019951396,-0.00843901253452423));
#28983=CARTESIAN_POINT('',(0.00231729913548905,-0.00427363416208414,-0.00836634095469408));
#28984=CARTESIAN_POINT('',(0.00165738540690343,-0.00457042975695016,-0.00833033048917846));
#28985=CARTESIAN_POINT('',(0.000267020440624387,-0.00485440350324432,-0.00825760542456511));
#28986=CARTESIAN_POINT('',(-0.00045642747601189,-0.00483994949353287,-0.00822159473718368));
#28987=CARTESIAN_POINT('',(-0.00183435335107504,-0.00450271828510711,-0.00814892369360519));
#28988=CARTESIAN_POINT('',(-0.00248268968912489,-0.00417954622329111,-0.00811282380429882));
#28989=CARTESIAN_POINT('',(-0.00358317565607922,-0.00328660442613433,-0.0080403129120517));
#28990=CARTESIAN_POINT('',(-0.00403196568092499,-0.00271592746345426,-0.00800403702252997));
#28991=CARTESIAN_POINT('',(-0.0046438810509595,-0.00144017841039065,-0.00793178854883908));
#28992=CARTESIAN_POINT('',(-0.00480647376857799,-0.000730306838074603,-0.00789525441687993));
#28993=CARTESIAN_POINT('',(-0.00481346911223356,0.000681562507468902,-0.00782336369046775));
#28994=CARTESIAN_POINT('',(-0.00465825553960144,0.00139305428604982,-0.00778682985285337));
#28995=CARTESIAN_POINT('',(-0.00405919834765568,0.00267489142155148,-0.00771458064984247));
#28996=CARTESIAN_POINT('',(-0.00361625713727038,0.00325008079201076,-0.00767830541046259));
#28997=CARTESIAN_POINT('',(-0.0025249009581265,0.00415415821336665,-0.00760579366959928));
#28998=CARTESIAN_POINT('',(-0.00187986182427326,0.00448381204370238,-0.00756969435269181));
#28999=CARTESIAN_POINT('',(-0.000505456252163881,0.00483511511876958,-0.00749702277289005));
#29000=CARTESIAN_POINT('',(0.000217803291852552,0.00485678044349205,-0.00746101230736261));
#29001=CARTESIAN_POINT('',(0.00161100507485096,0.00458706833792869,-0.00738828724274465));
#29002=CARTESIAN_POINT('',(0.00227385248782256,0.00429686304231747,-0.00735227655536401));
#29003=CARTESIAN_POINT('',(0.00341783720476902,0.00345799262771487,-0.00727960551178858));
#29004=CARTESIAN_POINT('',(0.00389314928381935,0.00291131299915153,-0.0072435056224768));
#29005=CARTESIAN_POINT('',(0.00456815171266123,0.0016652046019313,-0.00717099473023737));
#29006=CARTESIAN_POINT('',(0.00476439101216452,0.000966223329314663,-0.00713471884071138));
#29007=CARTESIAN_POINT('',(0.00484151907170424,-0.000446584983550539,-0.00706247036702125));
#29008=CARTESIAN_POINT('',(0.00472007906582122,-0.00116464233918382,-0.00702593623504599));
#29009=CARTESIAN_POINT('',(0.0041862429134328,-0.00247171653222866,-0.00695404550866527));
#29010=CARTESIAN_POINT('',(0.00377056815458991,-0.00306965156128732,-0.00691751167103557));
#29011=CARTESIAN_POINT('',(0.00272657364139859,-0.00402466539239229,-0.00684526246802392));
#29012=CARTESIAN_POINT('',(0.00209723388046954,-0.00438656481634525,-0.006808987228659));
#29013=CARTESIAN_POINT('',(0.000742976793155499,-0.00480417951318747,-0.00673647548776654));
#29014=CARTESIAN_POINT('',(2.08852804327653E-5,-0.00486189415008334,-0.00670037617088551));
#29015=CARTESIAN_POINT('',(-0.0013833377635771,-0.0046604936290617,-0.00662770459105998));
#29016=CARTESIAN_POINT('',(-0.00205983341381761,-0.00440373033434133,-0.0065916941255317));
#29017=CARTESIAN_POINT('',(-0.00324376967147653,-0.00362139360003666,-0.00651896906093908));
#29018=CARTESIAN_POINT('',(-0.00374510407088497,-0.00309961814407148,-0.00648295837354621));
#29019=CARTESIAN_POINT('',(-0.00448098632680823,-0.00188681893953521,-0.00641028732997003));
#29020=CARTESIAN_POINT('',(-0.00471091219154346,-0.00119985876201278,-0.00637418744064019));
#29021=CARTESIAN_POINT('',(-0.00485766808138392,0.000209707527801528,-0.00630167654843758));
#29022=CARTESIAN_POINT('',(-0.00477148100110948,0.000930579547873459,-0.00626540065889905));
#29023=CARTESIAN_POINT('',(-0.00430207970226759,0.00226535986204828,-0.00619315218519742));
#29024=CARTESIAN_POINT('',(-0.00391509511291251,0.00288228527781205,-0.00615661805322093));
#29025=CARTESIAN_POINT('',(-0.00292169917945201,0.00388557412112162,-0.00608472732685399));
#29026=CARTESIAN_POINT('',(-0.00230884594833033,0.00427892221278309,-0.00604819348920526));
#29027=CARTESIAN_POINT('',(-0.000978852814690703,0.00476172054091953,-0.00597594428621812));
#29028=CARTESIAN_POINT('',(-0.000258925776844936,0.00485523411170668,-0.00593966904683851));
#29029=CARTESIAN_POINT('',(0.00115205885347961,0.00472280803211538,-0.00586715730595063));
#29030=CARTESIAN_POINT('',(0.00184127085802903,0.00449979694530251,-0.00583105798905901));
#29031=CARTESIAN_POINT('',(0.00306153114480066,0.00377635423180173,-0.00575838640925034));
#29032=CARTESIAN_POINT('',(0.00358827257096136,0.00328025220169526,-0.00572237594372284));
#29033=CARTESIAN_POINT('',(0.00438269974046719,0.00210439451456262,-0.00564965087911179));
#29034=CARTESIAN_POINT('',(0.00464619750860448,0.00143048448149637,-0.00561364019173723));
#29035=CARTESIAN_POINT('',(0.00486194590083922,2.83941718670394E-5,-0.00554096914814263));
#29036=CARTESIAN_POINT('',(0.00481148142262117,-0.000694263094902669,-0.00550486925883093));
#29037=CARTESIAN_POINT('',(0.00440764851959588,-0.00205269358742436,-0.00543235836661051));
#29038=CARTESIAN_POINT('',(0.00405215626121919,-0.00268571012462328,-0.00539608247708809));
#29039=CARTESIAN_POINT('',(0.00310768769660717,-0.00373925423709395,-0.00532383400337187));
#29040=CARTESIAN_POINT('',(0.0025140734194861,-0.00416112641087264,-0.00528729987140581));
#29041=CARTESIAN_POINT('',(0.00121235323067142,-0.00470788827289234,-0.00521540914503274));
#29042=CARTESIAN_POINT('',(0.000495622876171233,-0.00483676574590275,-0.00517887530739772));
#29043=CARTESIAN_POINT('',(-0.000917889479730532,-0.00477384690220479,-0.00510662610438912));
#29044=CARTESIAN_POINT('',(-0.00161880142913644,-0.00458473802636499,-0.00507035086502769));
#29045=CARTESIAN_POINT('',(-0.00287170398311014,-0.00392243184051759,-0.00499783912412512));
#29046=CARTESIAN_POINT('',(-0.0034231101995181,-0.00345264644635782,-0.00496173980723916));
#29047=CARTESIAN_POINT('',(-0.00427363416208043,-0.00231729913548583,-0.00488906822743356));
#29048=CARTESIAN_POINT('',(-0.0045704297569521,-0.00165738540690207,-0.00485305776190536));
#29049=CARTESIAN_POINT('',(-0.00485440350324243,-0.000267020440625468,-0.00478033269729277));
#29050=CARTESIAN_POINT('',(-0.00483994949352744,0.000456427476012682,-0.004744322009919));
#29051=CARTESIAN_POINT('',(-0.00450271828511242,0.00183435335107489,-0.0046716509663244));
#29052=CARTESIAN_POINT('',(-0.00417954622329755,0.00248268968912865,-0.00463555107701158));
#29053=CARTESIAN_POINT('',(-0.00328660442612768,0.00358317565607573,-0.00456304018479348));
#29054=CARTESIAN_POINT('',(-0.00271592746345708,0.00403196568092808,-0.0045267642952492));
#29055=CARTESIAN_POINT('',(-0.00144017841038773,0.00464388105095646,-0.00445451582157441));
#29056=CARTESIAN_POINT('',(-0.000730306838075307,0.00480647376858355,-0.00441798168957843));
#29057=CARTESIAN_POINT('',(0.000681562507469923,0.004813469112228,-0.00434609096322378));
#29058=CARTESIAN_POINT('',(0.00139305428604971,0.00465825553960303,-0.00430955712557991));
#29059=CARTESIAN_POINT('',(0.00267489142155213,0.00405919834765383,-0.00423730792257054));
#29060=CARTESIAN_POINT('',(0.0032500807920042,0.00361625713726574,-0.00420103268320758));
#29061=CARTESIAN_POINT('',(0.00415415821337343,0.00252490095813086,-0.00412852094230885));
#29062=CARTESIAN_POINT('',(0.00448381204369767,0.00187986182427097,-0.00409242162542985));
#29063=CARTESIAN_POINT('',(0.00483511511877444,0.000505456252165615,-0.0040197500456066));
#29064=CARTESIAN_POINT('',(0.00485678044349787,-0.000217803291852029,-0.00398373958007876));
#29065=CARTESIAN_POINT('',(0.00458706833792301,-0.00161100507485092,-0.00391101451548305));
#29066=CARTESIAN_POINT('',(0.00429686304231271,-0.00227385248782118,-0.00387500382810275));
#29067=CARTESIAN_POINT('',(0.00345799262771932,-0.0034178372047709,-0.00380233278450431));
#29068=CARTESIAN_POINT('',(0.00291131299915669,-0.00389314928382361,-0.00376623289519071));
#29069=CARTESIAN_POINT('',(0.00166520460192559,-0.00456815171265726,-0.00369372200297799));
#29070=CARTESIAN_POINT('',(0.000966223329313892,-0.00476439101216487,-0.00365744611343869));
#29071=CARTESIAN_POINT('',(-0.000446584983549747,-0.00484151907170383,-0.00358519763974856));
#29072=CARTESIAN_POINT('',(-0.0011646423391832,-0.00472007906581732,-0.0035486635077798));
#29073=CARTESIAN_POINT('',(-0.00247171653222966,-0.00418624291343652,-0.00347677278138603));
#29074=CARTESIAN_POINT('',(-0.00306965156128558,-0.00377056815458988,-0.0034402389437644));
#29075=CARTESIAN_POINT('',(-0.00402466539239451,-0.00272657364139803,-0.00336798974074966));
#29076=CARTESIAN_POINT('',(-0.00438656481634332,-0.00209723388046953,-0.003331714501389));
#29077=CARTESIAN_POINT('',(-0.00480417951318985,-0.000742976793153918,-0.00325920276049104));
#29078=CARTESIAN_POINT('',(-0.00486189415008336,-2.08852804317659E-5,-0.00322310344361396));
#29079=CARTESIAN_POINT('',(-0.00466049362906131,0.00138333776357806,-0.00315043186378611));
#29080=CARTESIAN_POINT('',(-0.00440373033433799,0.00205983341381625,-0.00311442139826632));
#29081=CARTESIAN_POINT('',(-0.00362139360003972,0.0032437696714782,-0.00304169633365911));
#29082=CARTESIAN_POINT('',(-0.00309961814406801,0.00374510407088595,-0.00300568564627766));
#29083=CARTESIAN_POINT('',(-0.00188681893953579,0.00448098632680893,-0.00293301460269303));
#29084=CARTESIAN_POINT('',(-0.00119985876201082,0.00471091219154023,-0.00289691471337792));
#29085=CARTESIAN_POINT('',(0.000209707527800109,0.00485766808138716,-0.00282440382115445));
#29086=CARTESIAN_POINT('',(0.000930579547875407,0.00477148100110929,-0.00278812793162741));
#29087=CARTESIAN_POINT('',(0.00226535986204975,0.00430207970226656,-0.00271587945792348));
#29088=CARTESIAN_POINT('',(0.0028822852778121,0.0039150951129117,-0.00267934532594897));
#29089=CARTESIAN_POINT('',(0.00388557412112173,0.00292169917945267,-0.0026074545995805));
#29090=CARTESIAN_POINT('',(0.00427892221278101,0.00230884594832717,-0.00257092076193929));
#29091=CARTESIAN_POINT('',(0.00476172054092358,0.000978852814688521,-0.00249867155893835));
#29092=CARTESIAN_POINT('',(0.00485523411170341,0.000258925776843461,-0.00246239631957351));
#29093=CARTESIAN_POINT('',(0.00472280803211865,-0.00115205885347851,-0.00238988457867017));
#29094=CARTESIAN_POINT('',(0.00449979694530029,-0.00184127085803015,-0.00235378526179305));
#29095=CARTESIAN_POINT('',(0.00377635423180104,-0.00306153114480446,-0.00228111368197056));
#29096=CARTESIAN_POINT('',(0.00328025220169769,-0.00358827257096685,-0.00224510321644117));
#29097=CARTESIAN_POINT('',(0.00210439451455585,-0.00438269974046463,-0.00217237815184775));
#29098=CARTESIAN_POINT('',(0.00143048448149287,-0.00464619750860529,-0.00213636746446399));
#29099=CARTESIAN_POINT('',(2.83941718649254E-5,-0.00486194590083927,-0.00206369642087015));
#29100=CARTESIAN_POINT('',(-0.000694263094903681,-0.00481148142262189,-0.00202759653155857));
#29101=CARTESIAN_POINT('',(-0.00205269358742362,-0.00440764851959508,-0.0019550856393374));
#29102=CARTESIAN_POINT('',(-0.00268571012462754,-0.00405215626122127,-0.00191880974980833));
#29103=CARTESIAN_POINT('',(-0.00373925423709378,-0.00310768769660141,-0.00184656127610592));
#29104=CARTESIAN_POINT('',(-0.00416112641087175,-0.00251407341948451,-0.00181002714413654));
#29105=CARTESIAN_POINT('',(-0.00470788827289332,-0.00121235323067282,-0.00173813641775658));
#29106=CARTESIAN_POINT('',(-0.0048367657459032,-0.000495622876167294,-0.00170160258012523));
#29107=CARTESIAN_POINT('',(-0.0047738469022041,0.000917889479732164,-0.00162935337711587));
#29108=CARTESIAN_POINT('',(-0.00458473802636611,0.00161880142913698,-0.00159307813775496));
#29109=CARTESIAN_POINT('',(-0.00392243184051651,0.00287170398310953,-0.00152056639685241));
#29110=CARTESIAN_POINT('',(-0.00345264644635402,0.00342311019951849,-0.00148446707997406));
#29111=CARTESIAN_POINT('',(-0.00231729913548722,0.00427363416208182,-0.00141179550015312));
#29112=CARTESIAN_POINT('',(-0.00165738540690224,0.00457042975695331,-0.00137578503462994));
#29113=CARTESIAN_POINT('',(-0.000267020440625006,0.00485440350324129,-0.00130305997002273));
#29114=CARTESIAN_POINT('',(0.000456427476013587,0.00483994949352714,-0.00126704928265082));
#29115=CARTESIAN_POINT('',(0.00183435335107614,0.00450271828511218,-0.00119437823904703));
#29116=CARTESIAN_POINT('',(0.00248268968913113,0.00417954622329636,-0.00115827834973921));
#29117=CARTESIAN_POINT('',(0.00358317565607457,0.00328660442612778,-0.00108576745752035));
#29118=CARTESIAN_POINT('',(0.00403196568092297,0.0027159274634508,-0.00104949156799179));
#29119=CARTESIAN_POINT('',(0.00464388105096199,0.00144017841039315,-0.000977243094286331));
#29120=CARTESIAN_POINT('',(0.00480647376858471,0.000730306838074866,-0.000940708962314518));
#29121=CARTESIAN_POINT('',(0.00481346911222684,-0.000681562507469895,-0.00086881823594223));
#29122=CARTESIAN_POINT('',(0.00465825553960098,-0.00139305428604988,-0.000832284398307179));
#29123=CARTESIAN_POINT('',(0.00405919834765599,-0.00267489142155171,-0.000760035195297809));
#29124=CARTESIAN_POINT('',(0.00361625713726488,-0.00325008079200467,-0.000723759955934081));
#29125=CARTESIAN_POINT('',(0.00252490095813153,-0.00415415821337312,-0.000651248215036885));
#29126=CARTESIAN_POINT('',(0.00187986182427066,-0.00448381204369751,-0.000615148898156361));
#29127=CARTESIAN_POINT('',(0.000505456252165614,-0.00483511511877466,-0.000542477318334643));
#29128=CARTESIAN_POINT('',(-0.000217803291853572,-0.0048567804434947,-0.000506466852810241));
#29129=CARTESIAN_POINT('',(-0.00161100507485052,-0.00458706833792599,-0.000433741788206097));
#29130=CARTESIAN_POINT('',(-0.00227385248782081,-0.00429686304231336,-0.000397731100828119));
#29131=CARTESIAN_POINT('',(-0.0034178372047709,-0.00345799262771901,-0.000325060057233522));
#29132=CARTESIAN_POINT('',(-0.00389314928382333,-0.00291131299915446,-0.000288960167921819));
#29133=CARTESIAN_POINT('',(-0.00456815171265774,-0.00166520460192758,-0.000216449275701425));
#29134=CARTESIAN_POINT('',(-0.00476439101216319,-0.000966223329313042,-0.000180173386168644));
#29135=CARTESIAN_POINT('',(-0.00484151907170559,0.000446584983549208,-0.000107924912473147));
#29136=CARTESIAN_POINT('',(-0.00472007906582131,0.00116464233918359,-7.13907804971041E-5));
#29137=CARTESIAN_POINT('',(-0.00418624291343246,0.00247171653222957,4.99945876723195E-7));
#29138=CARTESIAN_POINT('',(-0.00377056815458997,0.003069651561286,3.70337835121602E-5));
#29139=CARTESIAN_POINT('',(-0.00272657364139774,0.00402466539239435,0.00010928298651923));
#29140=CARTESIAN_POINT('',(-0.00209723388046976,0.00438656481634434,0.000145558225883721));
#29141=CARTESIAN_POINT('',(-0.000742976793153477,0.00480417951318895,0.000218069966781685));
#29142=CARTESIAN_POINT('',(-2.0885280432126E-5,0.00486189415008451,0.000254169283662596));
#29143=CARTESIAN_POINT('',(0.00138333776357875,0.00466049362906015,0.000326840863482779));
#29144=CARTESIAN_POINT('',(0.00205983341381665,0.0044037303343389,0.000362851329005269));
#29145=CARTESIAN_POINT('',(0.00324376967147804,0.00362139360003873,0.000435576393614782));
#29146=CARTESIAN_POINT('',(0.00374510407088124,0.00309961814406744,0.00047158708098969));
#29147=CARTESIAN_POINT('',(0.00448098632681381,0.00188681893953618,0.000544258124585055));
#29148=CARTESIAN_POINT('',(0.0047109121915401,0.00119985876201141,0.000580358013895203));
#29149=CARTESIAN_POINT('',(0.00485766808138741,-0.000209707527801439,0.000652868906117898));
#29150=CARTESIAN_POINT('',(0.00477148100111083,-0.000930579547875692,0.000689144795648389));
#29151=CARTESIAN_POINT('',(0.00430207970226465,-0.00226535986205061,0.000761393269346187));
#29152=CARTESIAN_POINT('',(0.00391509511291008,-0.00288228527780993,0.000797927401320691));
#29153=CARTESIAN_POINT('',(0.00292169917945418,-0.00388557412112409,0.000869818127695285));
#29154=CARTESIAN_POINT('',(0.00230884594832506,-0.00427892221277948,0.000906351965326132));
#29155=CARTESIAN_POINT('',(0.000978852814690916,-0.00476172054092505,0.000978601168341638));
#29156=CARTESIAN_POINT('',(0.000258925776844741,-0.00485523411170611,0.00101487640770113));
#29157=CARTESIAN_POINT('',(-0.00115205885348002,-0.00472280803211599,0.00108738814860063));
#29158=CARTESIAN_POINT('',(-0.00184127085802862,-0.00449979694529959,0.00112348746547846));
#29159=CARTESIAN_POINT('',(-0.00306153114480408,-0.00377635423180277,0.00119615904530325));
#29160=CARTESIAN_POINT('',(-0.0035882725709651,-0.00328025220169392,0.00123216951082539));
#29161=CARTESIAN_POINT('',(-0.00438269974046544,-0.00210439451456205,0.00130489457543106));
#29162=CARTESIAN_POINT('',(-0.00464619750860506,-0.00143048448149263,0.00134090526280791));
#29163=CARTESIAN_POINT('',(-0.00486194590083901,-2.83941718649549E-5,0.00141357630640327));
#29164=CARTESIAN_POINT('',(-0.0048114814226229,0.000694263094889662,0.00144967619571505));
#29165=CARTESIAN_POINT('',(-0.00440764851959346,0.00205269358742906,0.00152218708793468));
#29166=CARTESIAN_POINT('',(-0.00405215626119944,0.0026857101246911,0.00155846297747023));
#29167=CARTESIAN_POINT('',(-0.00310768769666081,0.00373925423700836,0.00163071145114705));
#29168=CARTESIAN_POINT('',(-0.00251407341960766,0.00416112641070731,0.00166724558321998));
#29169=CARTESIAN_POINT('',(-0.0012123532301178,0.00470788827330421,0.00173913630957742));
#29170=CARTESIAN_POINT('',(-0.000495622876939057,0.00483676574602459,0.00177567014631293));
#29171=CARTESIAN_POINT('',(0.000917889477907517,0.0047738469014571,0.00184791935053893));
#29172=CARTESIAN_POINT('',(0.00161880143500428,0.00458473802439018,0.00188419459299961));
#29173=CARTESIAN_POINT('',(0.00287170398482693,0.00392243184277044,0.00195670632674376));
#29174=CARTESIAN_POINT('',(0.00342311018306367,0.0034526464567348,0.00199280563664444));
#29175=CARTESIAN_POINT('',(0.00427363417322163,0.00231729911780535,0.00206547725050609));
#29176=CARTESIAN_POINT('',(0.00457042977174294,0.00165738541607217,0.00210148771169285));
#29177=CARTESIAN_POINT('',(0.00485440343966745,0.000267020530351741,0.00217421263830122));
#29178=CARTESIAN_POINT('',(0.00483994947871846,-0.000456427850068477,0.00221022347312812));
#29179=CARTESIAN_POINT('',(0.00450271857873417,-0.00183435351687859,0.00228289499949617));
#29180=CARTESIAN_POINT('',(0.00417954681684493,-0.00248268734221482,0.00231899393251005));
#29181=CARTESIAN_POINT('',(0.00328660218651989,-0.0035831764053507,0.0023915033797381));
#29182=CARTESIAN_POINT('',(0.00271592340140939,-0.00403197462474551,0.0024277835632829));
#29183=CARTESIAN_POINT('',(0.00144019517612842,-0.00464387514350149,0.0025000356117708));
#29184=CARTESIAN_POINT('',(0.000730316340889192,-0.00480643860397344,0.00253653941438567));
#29185=CARTESIAN_POINT('',(-0.00123075016520761,-0.00481623257959065,0.00263642085553527));
#29186=CARTESIAN_POINT('',(-0.00249186065161184,-0.00430099307276901,0.00270163700098398));
#29187=CARTESIAN_POINT('',(-0.00427649949251748,-0.00253521549583444,0.00282965584356534));
#29188=CARTESIAN_POINT('',(-0.00480374912175907,-0.00126752528841583,0.00289545230430405));
#29189=CARTESIAN_POINT('',(-0.00480994288355359,-2.43665513178439E-5,0.00295881582269299));
#29190=CARTESIAN_POINT('',(-0.00481,2.43712308653186E-5,-0.0152300713606537));
#29191=CARTESIAN_POINT('',(-0.00480690252434544,0.000645958221424933,-0.015198389586565));
#29192=CARTESIAN_POINT('',(-0.00467712430393056,0.00128470170063566,-0.0151654813513713));
#29193=CARTESIAN_POINT('',(-0.00388793251657289,0.00316730242218104,-0.0150617853642725));
#29194=CARTESIAN_POINT('',(-0.00273168049484676,0.00420588673001337,-0.014988829115302));
#29195=CARTESIAN_POINT('',(-0.000694345269151162,0.00481158888805761,-0.0148800363035863));
#29196=CARTESIAN_POINT('',(2.83713107815876E-5,0.00486198731371525,-0.0148439092190894));
#29197=CARTESIAN_POINT('',(0.0014305306932682,0.00464623359414285,-0.0147712492556481));
#29198=CARTESIAN_POINT('',(0.00210442685798093,0.00438275491925437,-0.0147352455159436));
#29199=CARTESIAN_POINT('',(0.00328028975549539,0.00358831715552897,-0.014662515643209));
#29200=CARTESIAN_POINT('',(0.00377640149651015,0.00306156230762301,-0.0146265042621575));
#29201=CARTESIAN_POINT('',(0.00449985258902826,0.00184128806164442,-0.0145538343796196));
#29202=CARTESIAN_POINT('',(0.00472286532095683,0.00115206864444611,-0.0145177348671644));
#29203=CARTESIAN_POINT('',(0.00485529143886879,-0.000258933307440913,-0.0144452226301512));
#29204=CARTESIAN_POINT('',(0.00476177621900751,-0.000978868749884339,-0.0144089475733588));
#29205=CARTESIAN_POINT('',(0.004278970983756,-0.00230887726412092,-0.0143366984883185));
#29206=CARTESIAN_POINT('',(0.00388561768822807,-0.00292173733364788,-0.0143001645803893));
#29207=CARTESIAN_POINT('',(0.00288231585551244,-0.00391514436671711,-0.0142282738188832));
#29208=CARTESIAN_POINT('',(0.00226538287099962,-0.00430213287315544,-0.014191739718195));
#29209=CARTESIAN_POINT('',(0.00093058617559742,-0.00477153857116873,-0.0141194912327727));
#29210=CARTESIAN_POINT('',(0.000209705532278956,-0.00485772598627435,-0.0140832153449124));
#29211=CARTESIAN_POINT('',(-0.00119987733461742,-0.0047109670668637,-0.0140107044565176));
#29212=CARTESIAN_POINT('',(-0.00188684551851613,-0.00448103781073583,-0.0139746045613348));
#29213=CARTESIAN_POINT('',(-0.00309965835778344,-0.00374514575282502,-0.0139019335286979));
#29214=CARTESIAN_POINT('',(-0.00362143963251185,-0.00324380485226769,-0.0138659228311588));
#29215=CARTESIAN_POINT('',(-0.00440378449138592,-0.00205985392237314,-0.0137931977801048));
#29216=CARTESIAN_POINT('',(-0.00466055027259019,-0.0013833499116694,-0.0137571873044536));
#29217=CARTESIAN_POINT('',(-0.0048619518764676,2.0889889465098E-5,-0.0136845157355505));
#29218=CARTESIAN_POINT('',(-0.00480423591641779,0.000742989987634153,-0.0136484164128556));
#29219=CARTESIAN_POINT('',(-0.00438661502827952,0.00209726275005554,-0.0135759046751557));
#29220=CARTESIAN_POINT('',(-0.00402471076561506,0.00272660964436907,-0.0135396294384451));
#29221=CARTESIAN_POINT('',(-0.00306968457802422,0.00377061576744125,-0.0134673802260291));
#29222=CARTESIAN_POINT('',(-0.00247174219745113,0.00418629483787636,-0.0134308464034582));
#29223=CARTESIAN_POINT('',(-0.00116465174556414,0.00472013627090797,-0.0133589556504941));
#29224=CARTESIAN_POINT('',(-0.000446585888062056,0.00484157699819559,-0.0133224215335274));
#29225=CARTESIAN_POINT('',(0.000966239236385627,0.00476444673805005,-0.0132501730505603));
#29226=CARTESIAN_POINT('',(0.00166522860381854,0.00456820444675366,-0.0132138971635795));
#29227=CARTESIAN_POINT('',(0.00291135115826841,0.00389319287385263,-0.0131413862746769));
#29228=CARTESIAN_POINT('',(0.00345803688564065,0.00341787459831736,-0.0131052863794496));
#29229=CARTESIAN_POINT('',(0.00429691614588139,0.0022738756080041,-0.0130326153469013));
#29230=CARTESIAN_POINT('',(0.00458712432947191,0.00161101996177957,-0.0129966046493296));
#29231=CARTESIAN_POINT('',(0.00485683832637343,0.000217801514243265,-0.0129238795982987));
#29232=CARTESIAN_POINT('',(0.00483517209944476,-0.000505466705321743,-0.0128878691226277));
#29233=CARTESIAN_POINT('',(0.00448386361212515,-0.00187988817339661,-0.0128151975537403));
#29234=CARTESIAN_POINT('',(0.00415420527386462,-0.00252493473283444,-0.0127790982310671));
#29235=CARTESIAN_POINT('',(0.00325011613385979,-0.00361630302454977,-0.0127065864933079));
#29236=CARTESIAN_POINT('',(0.00267491956319904,-0.00405924897364133,-0.0126703112566191));
#29237=CARTESIAN_POINT('',(0.00139306656888672,-0.00465831216310324,-0.0125980620442184));
#29238=CARTESIAN_POINT('',(0.000681566348417449,-0.00481352690581254,-0.0125615282216268));
#29239=CARTESIAN_POINT('',(-0.000730320039149999,-0.00480653021885982,-0.0124896374686892));
#29240=CARTESIAN_POINT('',(-0.00144019974224342,-0.00464393491420252,-0.0124531033517134));
#29241=CARTESIAN_POINT('',(-0.00271596348504431,-0.00403201107755429,-0.0123808548687378));
#29242=CARTESIAN_POINT('',(-0.00328664678144064,-0.00358321519089635,-0.0123445789817365));
#29243=CARTESIAN_POINT('',(-0.00417959815891117,-0.00248271535820966,-0.0122720680928834));
#29244=CARTESIAN_POINT('',(-0.00450277348399899,-0.00183437096143296,-0.0122359681976468));
#29245=CARTESIAN_POINT('',(-0.00484000740253075,-0.000456428514420108,-0.0121632971650678));
#29246=CARTESIAN_POINT('',(-0.00485446092968617,0.000267028113936751,-0.0121272864675541));
#29247=CARTESIAN_POINT('',(-0.0045704825534782,0.00165740920001288,-0.012054561416438));
#29248=CARTESIAN_POINT('',(-0.00427368280511274,0.00231733059850723,-0.0120185509408203));
#29249=CARTESIAN_POINT('',(-0.00342314775915248,0.00345269052415205,-0.0119458793719114));
#29250=CARTESIAN_POINT('',(-0.00287173453630625,0.00392248105352976,-0.0119097800492129));
#29251=CARTESIAN_POINT('',(-0.00161881652045838,0.004584793945446,-0.0118372683115257));
#29252=CARTESIAN_POINT('',(-0.000917896105497493,0.00477390444385893,-0.0118009930747972));
#29253=CARTESIAN_POINT('',(0.000495633197181967,0.00483682275963525,-0.0117287438624042));
#29254=CARTESIAN_POINT('',(0.00121237179874327,0.00470794313706156,-0.0116922100397982));
#29255=CARTESIAN_POINT('',(0.00251410721827715,0.00416117351230247,-0.0116203192868814));
#29256=CARTESIAN_POINT('',(0.00310772801722916,0.00373929583689428,-0.0115837851698876));
#29257=CARTESIAN_POINT('',(0.00405220691337471,0.00268573828077846,-0.0115115366869274));
#29258=CARTESIAN_POINT('',(0.00440770278012855,0.00205271390416126,-0.0114752607999356));
#29259=CARTESIAN_POINT('',(0.00481153922799867,0.000694266935140251,-0.011402749911048));
#29260=CARTESIAN_POINT('',(0.00486200363716491,-2.83990257214252E-5,-0.0113666500158559));
#29261=CARTESIAN_POINT('',(0.00464625140691769,-0.00143050568293938,-0.0112939789832225));
#29262=CARTESIAN_POINT('',(0.00438274985912934,-0.00210442357992527,-0.0112579682857279));
#29263=CARTESIAN_POINT('',(0.00358831224336821,-0.0032802943880181,-0.0111852432346279));
#29264=CARTESIAN_POINT('',(0.00306156404473304,-0.0037764019147314,-0.0111492327590233));
#29265=CARTESIAN_POINT('',(0.00184128869076233,-0.00449985204131579,-0.0110765611900722));
#29266=CARTESIAN_POINT('',(0.00115206824794929,-0.00472286519122483,-0.0110404618674185));
#29267=CARTESIAN_POINT('',(-0.000258933233588031,-0.00485529154938711,-0.0109679501296838));
#29268=CARTESIAN_POINT('',(-0.000978868713517307,-0.00476177623805386,-0.0109316748929821));
#29269=CARTESIAN_POINT('',(-0.00230887730190845,-0.00427897093691872,-0.010859425680583));
#29270=CARTESIAN_POINT('',(-0.00292173732970695,-0.00388561770330084,-0.0108228918579371));
#29271=CARTESIAN_POINT('',(-0.00391514436387597,-0.00288231585963184,-0.0107510011051061));
#29272=CARTESIAN_POINT('',(-0.00430213287321797,-0.00226538286521935,-0.0107144669880661));
#29273=CARTESIAN_POINT('',(-0.00477153857249349,-0.000930586177030942,-0.0106422185051128));
#29274=CARTESIAN_POINT('',(-0.00485772598645182,-0.000209705533414721,-0.0106059426180949));
#29275=CARTESIAN_POINT('',(-0.00471096706635025,0.00119987733525803,-0.0105334317292525));
#29276=CARTESIAN_POINT('',(-0.00448103781074004,0.00188684551865477,-0.010497331834055));
#29277=CARTESIAN_POINT('',(-0.00374514575298108,0.00309965835763356,-0.0104246608013869));
#29278=CARTESIAN_POINT('',(-0.00324380485225424,0.00362143963252127,-0.0103886501039201));
#29279=CARTESIAN_POINT('',(-0.002059853922329,0.00440378449138652,-0.0103159250527994));
#29280=CARTESIAN_POINT('',(-0.00138334991168053,0.00466055027259388,-0.0102799145771913));
#29281=CARTESIAN_POINT('',(2.08898894649507E-5,0.00486195187646364,-0.0102072430082677));
#29282=CARTESIAN_POINT('',(0.000742989987636098,0.00480423591641733,-0.0101711436855808));
#29283=CARTESIAN_POINT('',(0.00209726275005457,0.00438661502828031,-0.0100986319478852));
#29284=CARTESIAN_POINT('',(0.00272660964436737,0.0040247107656129,-0.0100623567111655));
#29285=CARTESIAN_POINT('',(0.00377061576744357,0.00306968457802569,-0.00999010749876331));
#29286=CARTESIAN_POINT('',(0.00418629483786854,0.00247174219744889,-0.00995357367616607));
#29287=CARTESIAN_POINT('',(0.00472013627091582,0.00116465174556636,-0.00988168292324078));
#29288=CARTESIAN_POINT('',(0.00484157699820177,0.000446585888060814,-0.00984514880626354));
#29289=CARTESIAN_POINT('',(0.00476444673804396,-0.000966239236384054,-0.00977290032327878));
#29290=CARTESIAN_POINT('',(0.00456820444675509,-0.00166522860381626,-0.00973662443630273));
#29291=CARTESIAN_POINT('',(0.00389319287385112,-0.00291135115827085,-0.00966411354740819));
#29292=CARTESIAN_POINT('',(0.00341787459832332,-0.00345803688565274,-0.00962801365220536));
#29293=CARTESIAN_POINT('',(0.00227387560799953,-0.00429691614586831,-0.00955534261960021));
#29294=CARTESIAN_POINT('',(0.00161101996178304,-0.00458712432948514,-0.00951933192208457));
#29295=CARTESIAN_POINT('',(0.000217801514241914,-0.0048568383263598,-0.00944660687099837));
#29296=CARTESIAN_POINT('',(-0.000505466705321383,-0.00483517209944751,-0.00941059639536392));
#29297=CARTESIAN_POINT('',(-0.00187988817339405,-0.00448386361212312,-0.00933792482645878));
#29298=CARTESIAN_POINT('',(-0.00252493473283018,-0.00415420527386074,-0.00930182550378328));
#29299=CARTESIAN_POINT('',(-0.00361630302455418,-0.00325011613386351,-0.00922931376604625));
#29300=CARTESIAN_POINT('',(-0.00405924897363877,-0.002674919563202,-0.00919303852934839));
#29301=CARTESIAN_POINT('',(-0.00465831216310405,-0.00139306656888755,-0.00912078931694394));
#29302=CARTESIAN_POINT('',(-0.00481352690581081,-0.000681566348417764,-0.00908425549434557));
#29303=CARTESIAN_POINT('',(-0.00480653021886154,0.000730320039150845,-0.00901236474142489));
#29304=CARTESIAN_POINT('',(-0.00464393491419733,0.00144019974223911,-0.00897583062442999));
#29305=CARTESIAN_POINT('',(-0.00403201107756128,0.0027159634850448,-0.00890358214147594));
#29306=CARTESIAN_POINT('',(-0.00358321519089434,0.00328664678143411,-0.00886730625445426));
#29307=CARTESIAN_POINT('',(-0.00248271535821132,0.00417959815891801,-0.0087947953656203));
#29308=CARTESIAN_POINT('',(-0.0018343709614343,0.00450277348399542,-0.00875869547037181));
#29309=CARTESIAN_POINT('',(-0.000456428514422146,0.00484000740253341,-0.00868602443779733));
#29310=CARTESIAN_POINT('',(0.000267028113934224,0.00485446092967978,-0.00865001374026796));
#29311=CARTESIAN_POINT('',(0.00165740920001532,0.00457048255348461,-0.00857728868917869));
#29312=CARTESIAN_POINT('',(0.00231733059850565,0.00427368280511121,-0.008541278213545));
#29313=CARTESIAN_POINT('',(0.00345269052415222,0.00342314775915501,-0.0084686066446414));
#29314=CARTESIAN_POINT('',(0.00392248105353805,0.00287173453631088,-0.00843250732196013));
#29315=CARTESIAN_POINT('',(0.00458479394543713,0.00161881652045476,-0.00835999558423306));
#29316=CARTESIAN_POINT('',(0.00477390444385966,0.000917896105497934,-0.00832372034752825));
#29317=CARTESIAN_POINT('',(0.00483682275963445,-0.000495633197182035,-0.00825147113512762));
#29318=CARTESIAN_POINT('',(0.00470794313705902,-0.00121237179874085,-0.00821493731251739));
#29319=CARTESIAN_POINT('',(0.00416117351230491,-0.00251410721827962,-0.00814304655961665));
#29320=CARTESIAN_POINT('',(0.00373929583689171,-0.00310772801722806,-0.00810651244261374));
#29321=CARTESIAN_POINT('',(0.00268573828078122,-0.00405220691337558,-0.00803426395965584));
#29322=CARTESIAN_POINT('',(0.0020527139041605,-0.00440770278012326,-0.00799798807265104));
#29323=CARTESIAN_POINT('',(0.000694266935141895,-0.00481153922800366,-0.00792547718378718));
#29324=CARTESIAN_POINT('',(-2.83990257172541E-5,-0.00486200363715717,-0.00788937728856627));
#29325=CARTESIAN_POINT('',(-0.00143050568294196,-0.00464625140692552,-0.00781670625596649));
#29326=CARTESIAN_POINT('',(-0.00210442357991806,-0.0043827498591222,-0.00778069555843515));
#29327=CARTESIAN_POINT('',(-0.0032802943880256,-0.00358831224337504,-0.00770797050737502));
#29328=CARTESIAN_POINT('',(-0.00377640191471928,-0.00306156404472798,-0.00767196003172528));
#29329=CARTESIAN_POINT('',(-0.00449985204132647,-0.00184128869076967,-0.00759928846282476));
#29330=CARTESIAN_POINT('',(-0.00472286519121385,-0.00115206824794936,-0.00756318914012465));
#29331=CARTESIAN_POINT('',(-0.00485529154939798,0.000258933233587683,-0.00749067740243213));
#29332=CARTESIAN_POINT('',(-0.00476177623805565,0.000978868713516223,-0.0074544021657163));
#29333=CARTESIAN_POINT('',(-0.00427897093691827,0.00230887730190563,-0.00738215295330343));
#29334=CARTESIAN_POINT('',(-0.00388561770330705,0.00292173732971719,-0.00734561913069079));
#29335=CARTESIAN_POINT('',(-0.00288231585962521,0.00391514436386607,-0.00727372837780692));
#29336=CARTESIAN_POINT('',(-0.0022653828652209,0.00430213287321315,-0.00723719426078343));
#29337=CARTESIAN_POINT('',(-0.000930586177033348,0.0047715385724968,-0.00716494577785006));
#29338=CARTESIAN_POINT('',(-0.000209705533413502,0.00485772598645561,-0.00712866989082981));
#29339=CARTESIAN_POINT('',(0.00119987733525716,0.00471096706634635,-0.00705615900197206));
#29340=CARTESIAN_POINT('',(0.00188684551863979,0.00448103781072474,-0.00702005910673978));
#29341=CARTESIAN_POINT('',(0.003099658357646,0.00374514575299788,-0.00694738807415686));
#29342=CARTESIAN_POINT('',(0.00362143963251041,0.00324380485225148,-0.00691137737662819));
#29343=CARTESIAN_POINT('',(0.0044037844913961,0.00205985392233354,-0.00683865232554582));
#29344=CARTESIAN_POINT('',(0.00466055027259315,0.00138334991168341,-0.00680264184991632));
#29345=CARTESIAN_POINT('',(0.00486195187646409,-2.0889889466212E-5,-0.00672997028099736));
#29346=CARTESIAN_POINT('',(0.00480423591642111,-0.000742989987636956,-0.00669387095831539));
#29347=CARTESIAN_POINT('',(0.0043866150282763,-0.00209726275005415,-0.00662135922060507));
#29348=CARTESIAN_POINT('',(0.0040247107656172,-0.00272660964437124,-0.00658508398390573));
#29349=CARTESIAN_POINT('',(0.00306968457802141,-0.00377061576743955,-0.0065128347714775));
#29350=CARTESIAN_POINT('',(0.00247174219744538,-0.0041862948378624,-0.0064763009488776));
#29351=CARTESIAN_POINT('',(0.00116465174556965,-0.00472013627092198,-0.00640441019598375));
#29352=CARTESIAN_POINT('',(0.000446585888064109,-0.00484157699819391,-0.0063678760789755));
#29353=CARTESIAN_POINT('',(-0.000966239236386695,-0.00476444673805183,-0.00629562759602143));
#29354=CARTESIAN_POINT('',(-0.00166522860381339,-0.0045682044467502,-0.00625935170901975));
#29355=CARTESIAN_POINT('',(-0.00291135115827368,-0.00389319287385601,-0.00618684082014577));
#29356=CARTESIAN_POINT('',(-0.00345803688564666,-0.00341787459832007,-0.00615074092491954));
#29357=CARTESIAN_POINT('',(-0.00429691614587471,-0.00227387560800222,-0.00607806989234047));
#29358=CARTESIAN_POINT('',(-0.00458712432948343,-0.00161101996178013,-0.00604205919480918));
#29359=CARTESIAN_POINT('',(-0.00485683832636154,-0.000217801514244552,-0.00596933414372833));
#29360=CARTESIAN_POINT('',(-0.00483517209945259,0.000505466705323897,-0.00593332366809922));
#29361=CARTESIAN_POINT('',(-0.00448386361211786,0.00187988817339216,-0.00586065209917797));
#29362=CARTESIAN_POINT('',(-0.00415420527385522,0.00252493473282551,-0.00582455277649567));
#29363=CARTESIAN_POINT('',(-0.00325011613386882,0.00361630302455911,-0.00575204103878842));
#29364=CARTESIAN_POINT('',(-0.0026749195632004,0.00405924897363534,-0.00571576580206647));
#29365=CARTESIAN_POINT('',(-0.00139306656888904,0.00465831216310752,-0.00564351658968042));
#29366=CARTESIAN_POINT('',(-0.000681566348418915,0.00481352690578914,-0.0056069827670533));
#29367=CARTESIAN_POINT('',(0.000730320039152311,0.00480653021888319,-0.00553509201417171));
#29368=CARTESIAN_POINT('',(0.00144019974223843,0.00464393491419858,-0.0054985578971569));
#29369=CARTESIAN_POINT('',(0.00271596348504603,0.00403201107755983,-0.00542630941420362));
#29370=CARTESIAN_POINT('',(0.00328664678144265,0.00358321519089882,-0.00539003352719887));
#29371=CARTESIAN_POINT('',(0.00417959815890971,0.00248271535820656,-0.00531752263833027));
#29372=CARTESIAN_POINT('',(0.00450277348400127,0.00183437096143369,-0.00528142274310945));
#29373=CARTESIAN_POINT('',(0.00484000740252775,0.000456428514422211,-0.00520875171051427));
#29374=CARTESIAN_POINT('',(0.00485446092967311,-0.000267028113933861,-0.00517274101298296));
#29375=CARTESIAN_POINT('',(0.00457048255349136,-0.00165740920001511,-0.00510001596191823));
#29376=CARTESIAN_POINT('',(0.00427368280511466,-0.00231733059850962,-0.00506400548628336));
#29377=CARTESIAN_POINT('',(0.00342314775915118,-0.00345269052414871,-0.00499133391735751));
#29378=CARTESIAN_POINT('',(0.00287173453630816,-0.00392248105353095,-0.00495523459467405));
#29379=CARTESIAN_POINT('',(0.00161881652045694,-0.00458479394544451,-0.0048827228569737));
#29380=CARTESIAN_POINT('',(0.000917896105497196,-0.00477390444386005,-0.00484644762025596));
#29381=CARTESIAN_POINT('',(-0.00049563319718127,-0.00483682275963408,-0.00477419840785456));
#29382=CARTESIAN_POINT('',(-0.00121237179874249,-0.00470794313706126,-0.00473766458524968));
#29383=CARTESIAN_POINT('',(-0.00251410721827838,-0.00416117351230251,-0.00466577383233895));
#29384=CARTESIAN_POINT('',(-0.00310772801722835,-0.00373929583689227,-0.00462923971534218));
#29385=CARTESIAN_POINT('',(-0.00405220691337581,-0.0026857382807801,-0.00455699123238198));
#29386=CARTESIAN_POINT('',(-0.00440770278012495,-0.00205271390416107,-0.00452071534538068));
#29387=CARTESIAN_POINT('',(-0.00481153922800245,-0.000694266935139741,-0.00444820445651207));
#29388=CARTESIAN_POINT('',(-0.00486200363715706,2.83990257185022E-5,-0.00441210456129357));
#29389=CARTESIAN_POINT('',(-0.00464625140692539,0.00143050568294268,-0.00433943352869379));
#29390=CARTESIAN_POINT('',(-0.0043827498591258,0.00210442357992084,-0.00430342283117053));
#29391=CARTESIAN_POINT('',(-0.00358831224337125,0.00328029438802319,-0.00423069778009429));
#29392=CARTESIAN_POINT('',(-0.00306156404472769,0.00377640191472449,-0.00419468730445865));
#29393=CARTESIAN_POINT('',(-0.0018412886907671,0.00449985204132296,-0.00412201573554585));
#29394=CARTESIAN_POINT('',(-0.00115206824794905,0.00472286519122003,-0.00408591641286201));
#29395=CARTESIAN_POINT('',(0.000258933233587908,0.00485529154939188,-0.00401340467514939));
#29396=CARTESIAN_POINT('',(0.000978868713518797,0.00476177623805698,-0.00397712943844506));
#29397=CARTESIAN_POINT('',(0.00230887730190647,0.0042789709369157,-0.0039048802260291));
#29398=CARTESIAN_POINT('',(0.00292173732971809,0.00388561770330835,-0.00386834640341961));
#29399=CARTESIAN_POINT('',(0.00391514436386531,0.00288231585962375,-0.00379645565053266));
#29400=CARTESIAN_POINT('',(0.0043021328732162,0.0022653828652185,-0.00375992153351668));
#29401=CARTESIAN_POINT('',(0.00477153857249563,0.000930586177030387,-0.00368767305057105));
#29402=CARTESIAN_POINT('',(0.00485772598645863,0.000209705533410371,-0.0036513971635648));
#29403=CARTESIAN_POINT('',(0.00471096706634329,-0.0011998773352544,-0.00357888627469158));
#29404=CARTESIAN_POINT('',(0.00448103781072517,-0.00188684551864377,-0.00354278637947381));
#29405=CARTESIAN_POINT('',(0.00374514575299448,-0.0030996583576469,-0.00347011534687709));
#29406=CARTESIAN_POINT('',(0.00324380485224853,-0.00362143963250802,-0.00343410464934653));
#29407=CARTESIAN_POINT('',(0.00205985392233213,-0.00440378449140138,-0.00336137959828178));
#29408=CARTESIAN_POINT('',(0.00138334991167975,-0.00466055027259318,-0.00332536912264461));
#29409=CARTESIAN_POINT('',(-2.08898894681853E-5,-0.00486195187646488,-0.00325269755372335));
#29410=CARTESIAN_POINT('',(-0.00074298998763811,-0.00480423591642181,-0.00321659823104266));
#29411=CARTESIAN_POINT('',(-0.00209726275005327,-0.0043866150282755,-0.00314408649333233));
#29412=CARTESIAN_POINT('',(-0.00272660964437155,-0.00402471076561353,-0.00310781125662636));
#29413=CARTESIAN_POINT('',(-0.0037706157674433,-0.00306968457802139,-0.00303556204421116));
#29414=CARTESIAN_POINT('',(-0.00418629483786456,-0.00247174219744504,-0.00299902822160718));
#29415=CARTESIAN_POINT('',(-0.0047201362709199,-0.00116465174556981,-0.00292713746870873));
#29416=CARTESIAN_POINT('',(-0.00484157699819433,-0.000446585888059789,-0.00289060335170224));
#29417=CARTESIAN_POINT('',(-0.00476444673805111,0.000966239236387943,-0.00281835486874896));
#29418=CARTESIAN_POINT('',(-0.00456820444675054,0.00166522860381336,-0.00278207898174626));
#29419=CARTESIAN_POINT('',(-0.0038931928738557,0.00291135115827364,-0.00270956809287382));
#29420=CARTESIAN_POINT('',(-0.00341787459832011,0.00345803688565272,-0.00267346819765328));
#29421=CARTESIAN_POINT('',(-0.00227387560799978,0.00429691614587045,-0.00260079716506118));
#29422=CARTESIAN_POINT('',(-0.00161101996178054,0.00458712432948444,-0.00256478646753567));
#29423=CARTESIAN_POINT('',(-0.00021780151424385,0.00485683832636059,-0.00249206141645638));
#29424=CARTESIAN_POINT('',(0.000505466705324944,0.00483517209945441,-0.00245605094083143));
#29425=CARTESIAN_POINT('',(0.00187988817339327,0.0044838636121155,-0.00238337937190023));
#29426=CARTESIAN_POINT('',(0.00252493473282808,0.00415420527385413,-0.00234728004922253));
#29427=CARTESIAN_POINT('',(0.00361630302455786,0.00325011613386882,-0.00227476831151606));
#29428=CARTESIAN_POINT('',(0.00405924897364287,0.00267491956320294,-0.00223849307480867));
#29429=CARTESIAN_POINT('',(0.00465831216310039,0.00139306656888563,-0.00216624386239272));
#29430=CARTESIAN_POINT('',(0.00481352690579794,0.000681566348418114,-0.00212971003978478));
#29431=CARTESIAN_POINT('',(0.00480653021887437,-0.000730320039151922,-0.00205781928689476));
#29432=CARTESIAN_POINT('',(0.00464393491419765,-0.00144019974223965,-0.00202128516988457));
#29433=CARTESIAN_POINT('',(0.00403201107756084,-0.00271596348504455,-0.00194903668693051));
#29434=CARTESIAN_POINT('',(0.00358321519089824,-0.00328664678144329,-0.00191276079992653));
#29435=CARTESIAN_POINT('',(0.00248271535820694,-0.00417959815890921,-0.00184024991105715));
#29436=CARTESIAN_POINT('',(0.00183437096143363,-0.00450277348400167,-0.00180415001583673));
#29437=CARTESIAN_POINT('',(0.000456428514421963,-0.00484000740252739,-0.00173147898324156));
#29438=CARTESIAN_POINT('',(-0.000267028113935476,-0.00485446092967608,-0.00169546828571443));
#29439=CARTESIAN_POINT('',(-0.00165740920001464,-0.00457048255348819,-0.00162274323464126));
#29440=CARTESIAN_POINT('',(-0.00231733059850924,-0.00427368280511491,-0.00158673275900833));
#29441=CARTESIAN_POINT('',(-0.0034526905241487,-0.00342314775915125,-0.00151406119008708));
#29442=CARTESIAN_POINT('',(-0.0039224810535339,-0.0028717345363086,-0.00147796186740589));
#29443=CARTESIAN_POINT('',(-0.00458479394544172,-0.00161881652045623,-0.00140545012969634));
#29444=CARTESIAN_POINT('',(-0.00477390444386256,-0.000917896105497446,-0.00136917489298627));
#29445=CARTESIAN_POINT('',(-0.0048368227596316,0.000495633197181834,-0.00129692568057875));
#29446=CARTESIAN_POINT('',(-0.00470794313705758,0.00121237179874062,-0.00126039185796734));
#29447=CARTESIAN_POINT('',(-0.00416117351230611,0.00251410721828054,-0.00118850110507579));
#29448=CARTESIAN_POINT('',(-0.00373929583689225,0.00310772801722703,-0.00115196698806636));
#29449=CARTESIAN_POINT('',(-0.0026857382807799,0.00405220691337737,-0.0010797185051123));
#29450=CARTESIAN_POINT('',(-0.00205271390416077,0.00440770278012309,-0.0010434426181064));
#29451=CARTESIAN_POINT('',(-0.000694266935139823,0.00481153922800441,-0.000970931729240861));
#29452=CARTESIAN_POINT('',(2.83990257170628E-5,0.00486200363715436,-0.000934831834017371));
#29453=CARTESIAN_POINT('',(0.00143050568294445,0.00464625140692806,-0.000862160801424495));
#29454=CARTESIAN_POINT('',(0.00210442357992056,0.00438274985912574,-0.0008261501038993));
#29455=CARTESIAN_POINT('',(0.00328029438802367,0.00358831224337118,-0.000753425052819996));
#29456=CARTESIAN_POINT('',(0.00377640191472476,0.00306156404473047,-0.000717414577191283));
#29457=CARTESIAN_POINT('',(0.00449985204132285,0.00184128869076413,-0.000644743008267738));
#29458=CARTESIAN_POINT('',(0.00472286519121912,0.00115206824794936,-0.000608643685588099));
#29459=CARTESIAN_POINT('',(0.00485529154939288,-0.000258933233588963,-0.000536131947877782));
#29460=CARTESIAN_POINT('',(0.00476177623805602,-0.000978868713518357,-0.000499856711169238));
#29461=CARTESIAN_POINT('',(0.00427897093691628,-0.00230887730190805,-0.000427607498759415));
#29462=CARTESIAN_POINT('',(0.00388561770330911,-0.0029217373297186,-0.000391073676149546));
#29463=CARTESIAN_POINT('',(0.00288231585962286,-0.00391514436386499,-0.000319182923257227));
#29464=CARTESIAN_POINT('',(0.00226538286521803,-0.00430213287322061,-0.000282648806250469));
#29465=CARTESIAN_POINT('',(0.000930586177031152,-0.00477153857249115,-0.000210400323291803));
#29466=CARTESIAN_POINT('',(0.000209705533412433,-0.00485772598645825,-0.000174124436289757));
#29467=CARTESIAN_POINT('',(-0.00119987733525668,-0.00471096706634371,-0.000101613547421149));
#29468=CARTESIAN_POINT('',(-0.00188684551864319,-0.00448103781072582,-6.55136522011198E-5));
#29469=CARTESIAN_POINT('',(-0.00309965835764556,-0.00374514575299485,7.15738039559136E-6));
#29470=CARTESIAN_POINT('',(-0.00362143963251333,-0.00324380485224829,4.31680779204336E-5));
#29471=CARTESIAN_POINT('',(-0.00440378449139505,-0.00205985392233476,0.00011589312899667));
#29472=CARTESIAN_POINT('',(-0.00466055027259318,-0.0013833499116795,0.000151903604627322));
#29473=CARTESIAN_POINT('',(-0.00486195187646446,2.08898894681251E-5,0.000224575173550102));
#29474=CARTESIAN_POINT('',(-0.00480423591642288,0.000742989987624055,0.000260674496229834));
#29475=CARTESIAN_POINT('',(-0.00438661502827317,0.00209726275005857,0.000333186233940918));
#29476=CARTESIAN_POINT('',(-0.00402471076559106,0.00272660964443439,0.000369461470652192));
#29477=CARTESIAN_POINT('',(-0.00306968457809138,0.00377061576736623,0.000441710683041813));
#29478=CARTESIAN_POINT('',(-0.002471742197528,0.00418629483761571,0.000478244505748111));
#29479=CARTESIAN_POINT('',(-0.00116465174499404,0.0047201362713054,0.000550135258627114));
#29480=CARTESIAN_POINT('',(-0.000446585888841052,0.0048415769991423,0.000586669374733954));
#29481=CARTESIAN_POINT('',(0.000966239234472312,0.00476444673680397,0.00065891785890312));
#29482=CARTESIAN_POINT('',(0.00166522860838972,0.00456820444175427,0.000695193749022433));
#29483=CARTESIAN_POINT('',(0.00291135116219289,0.00389319287949821,0.000767704630734155));
#29484=CARTESIAN_POINT('',(0.00345803687626453,0.00341787461537647,0.000803804518873336));
#29485=CARTESIAN_POINT('',(0.00429691613675843,0.00227387557689792,0.000876475585588987));
#29486=CARTESIAN_POINT('',(0.00458712432903145,0.00161101996494976,0.000912486279229324));
#29487=CARTESIAN_POINT('',(0.00485683838280882,0.000217801624758837,0.000985211191673891));
#29488=CARTESIAN_POINT('',(0.00483517205219748,-0.00050546707194813,0.00102122181326199));
#29489=CARTESIAN_POINT('',(0.00448386339341055,-0.00187988821156079,0.00109389386837081));
#29490=CARTESIAN_POINT('',(0.00415420624873737,-0.00252493262350395,0.00112999223805531));
#29491=CARTESIAN_POINT('',(0.00325011547594119,-0.00361630500354902,0.00120250251618307));
#29492=CARTESIAN_POINT('',(0.0026749141028128,-0.00405925590161076,0.0012387820458946));
#29493=CARTESIAN_POINT('',(0.00139308020350591,-0.00465830042112489,0.00131103488438839));
#29494=CARTESIAN_POINT('',(0.000681577685454135,-0.00481351659471675,0.00134753834547939));
#29495=CARTESIAN_POINT('',(-0.00127951311719603,-0.00480384708244003,0.00144741961858554));
#29496=CARTESIAN_POINT('',(-0.00253526298152253,-0.00427549071008319,0.0015126361106183));
#29497=CARTESIAN_POINT('',(-0.00430219482895177,-0.00249195208003113,0.00164065404675544));
#29498=CARTESIAN_POINT('',(-0.00481625326789864,-0.00121879809522714,0.00170645154026259));
#29499=CARTESIAN_POINT('',(-0.00481005712741422,2.43759101882384E-5,0.00176981449410054));
#29500=CARTESIAN_POINT('',(-0.006,2.43712308653094E-5,-0.0152300713606537));
#29501=CARTESIAN_POINT('',(-0.00599690252296466,0.000804744810155825,-0.0151980803713376));
#29502=CARTESIAN_POINT('',(-0.00583736572769333,0.00159298335532281,-0.0151657322674743));
#29503=CARTESIAN_POINT('',(-0.00485144734603198,0.00395139172205703,-0.0150609128940259));
#29504=CARTESIAN_POINT('',(-0.00341173734068717,0.00524330426742482,-0.0149885940536295));
#29505=CARTESIAN_POINT('',(-0.000871709513217771,0.00600125062263071,-0.0148799265127186));
#29506=CARTESIAN_POINT('',(3.09456231818347E-5,0.00606467923987668,-0.0148437081733647));
#29507=CARTESIAN_POINT('',(0.00177788269483879,0.00579767665572992,-0.0147712652361108));
#29508=CARTESIAN_POINT('',(0.00262079982041912,0.00546892620520059,-0.014735042802557));
#29509=CARTESIAN_POINT('',(0.0040861725105118,0.00448104450356913,-0.0146625997584658));
#29510=CARTESIAN_POINT('',(0.00470725422304886,0.0038231374713461,-0.0146263783962704));
#29511=CARTESIAN_POINT('',(0.00561002149547192,0.00230389862445774,-0.0145539348965588));
#29512=CARTESIAN_POINT('',(0.00588984517702552,0.00144339140566514,-0.0145177135756586));
#29513=CARTESIAN_POINT('',(0.00605673801000797,-0.000315828556998168,-0.0144452699879439));
#29514=CARTESIAN_POINT('',(0.00594161714193286,-0.0012135250192261,-0.0144090487223906));
#29515=CARTESIAN_POINT('',(0.00534034342389439,-0.00287507220515675,-0.014336605167007));
#29516=CARTESIAN_POINT('',(0.00485259831696443,-0.00363767036522909,-0.0143003837319588));
#29517=CARTESIAN_POINT('',(0.00359825268706524,-0.00488212214941821,-0.0142279405377117));
#29518=CARTESIAN_POINT('',(0.00283158196400144,-0.00536350310207911,-0.0141917188067142));
#29519=CARTESIAN_POINT('',(0.00116524705640889,-0.00595137856142856,-0.0141192759847855));
#29520=CARTESIAN_POINT('',(0.000266605506933447,-0.00605917232737577,-0.014083054070165));
#29521=CARTESIAN_POINT('',(-0.00149119555580268,-0.00587794805649581,-0.0140106113143761));
#29522=CARTESIAN_POINT('',(-0.00234945104947196,-0.00559120884671478,-0.0139743894342706));
#29523=CARTESIAN_POINT('',(-0.00386122980401518,-0.00467600158772933,-0.0139019465260691));
#29524=CARTESIAN_POINT('',(-0.00451416703400287,-0.00404968665906797,-0.0138657248191622));
#29525=CARTESIAN_POINT('',(-0.00548995216528817,-0.00257623315922293,-0.0137932816441086));
#29526=CARTESIAN_POINT('',(-0.00581198832858315,-0.00173073160427836,-0.0137570601590698));
#29527=CARTESIAN_POINT('',(-0.00606464765160479,1.83374390645552E-5,-0.0136846167145914));
#29528=CARTESIAN_POINT('',(-0.0059938691252166,0.00092042665972075,-0.0136483954069969));
#29529=CARTESIAN_POINT('',(-0.005474834059304,0.00260960080412937,-0.0135759518024328));
#29530=CARTESIAN_POINT('',(-0.00502494259376194,0.00339490932190728,-0.0135397305379354));
#29531=CARTESIAN_POINT('',(-0.00383359144441473,0.00469988132061323,-0.0134672869867618));
#29532=CARTESIAN_POINT('',(-0.00309114007954832,0.00521777818798231,-0.0134310655505372));
#29533=CARTESIAN_POINT('',(-0.00145604475526128,0.00588748441466296,-0.0133586223554552));
#29534=CARTESIAN_POINT('',(-0.000563516845062604,0.006038830241408,-0.013322400624863));
#29535=CARTESIAN_POINT('',(0.0012009460703243,0.00594427758822637,-0.0132499578030685));
#29536=CARTESIAN_POINT('',(0.00207243349249206,0.00569997080779686,-0.0132137358883429));
#29537=CARTESIAN_POINT('',(0.00362707839031281,0.00485986006847225,-0.0131412931325354));
#29538=CARTESIAN_POINT('',(0.00431027272978388,0.00426650742375495,-0.013105071252456));
#29539=CARTESIAN_POINT('',(0.00535673952363115,0.00284243348643018,-0.0130326283442549));
#29540=CARTESIAN_POINT('',(0.00572029451972927,0.00201392568252568,-0.0129964066373418));
#29541=CARTESIAN_POINT('',(0.00605793618792313,0.000279215348634717,-0.0129239634622906));
#29542=CARTESIAN_POINT('',(0.00603189937079921,-0.000625164136977061,-0.0128877419772535));
#29543=CARTESIAN_POINT('',(0.00559598640309222,-0.00233778176403413,-0.0128152985327716));
#29544=CARTESIAN_POINT('',(0.00518538097196905,-0.00314411776208916,-0.0127790772251792));
#29545=CARTESIAN_POINT('',(0.00405943613844661,-0.00450608506039521,-0.012706633620614));
#29546=CARTESIAN_POINT('',(0.00334326606254171,-0.0050594495164588,-0.0126704123561171));
#29547=CARTESIAN_POINT('',(0.0017432099560226,-0.00580917608958445,-0.0125979688049435));
#29548=CARTESIAN_POINT('',(0.000859083785322923,-0.00600352656862025,-0.012561747368715));
#29549=CARTESIAN_POINT('',(-0.000907832795992274,-0.00599653055331017,-0.0124893041736411));
#29550=CARTESIAN_POINT('',(-0.00179033860487747,-0.00579480022081359,-0.0124530824430416));
#29551=CARTESIAN_POINT('',(-0.00338430604441628,-0.00503221423504633,-0.0123806396212533));
#29552=CARTESIAN_POINT('',(-0.00409596327930432,-0.00447300040297535,-0.0123444177065222));
#29553=CARTESIAN_POINT('',(-0.0052107714194494,-0.00310190244027309,-0.0122719749507197));
#29554=CARTESIAN_POINT('',(-0.00561489445973178,-0.00229226892145074,-0.0122357530706378));
#29555=CARTESIAN_POINT('',(-0.00603673420972488,-0.000576130653447598,-0.0121633101624367));
#29556=CARTESIAN_POINT('',(-0.00605555901945168,0.000328437222868882,-0.0121270884555252));
#29557=CARTESIAN_POINT('',(-0.00570365434124662,0.00206031046766952,-0.012054645280471));
#29558=CARTESIAN_POINT('',(-0.00533350841312408,0.00288588430551408,-0.0120184237954346));
#29559=CARTESIAN_POINT('',(-0.00427538695244329,0.00430132000746911,-0.0119459803509542));
#29560=CARTESIAN_POINT('',(-0.00358746557130879,0.00488914543665951,-0.0119097590433595));
#29561=CARTESIAN_POINT('',(-0.00202602586441541,0.00571655871399608,-0.0118373154387974));
#29562=CARTESIAN_POINT('',(-0.00115260758008782,0.00595373438615169,-0.011801094174299));
#29563=CARTESIAN_POINT('',(0.000612559445933921,0.00603407645922647,-0.0117286506231255));
#29564=CARTESIAN_POINT('',(0.00150376022760004,0.00587529245128564,-0.0116924291869014));
#29565=CARTESIAN_POINT('',(0.00313350103358548,0.00519265927390464,-0.0116199859918183));
#29566=CARTESIAN_POINT('',(0.00387163123167716,0.00466856439659248,-0.0115837642612236));
#29567=CARTESIAN_POINT('',(0.00505243610205558,0.00335404188172309,-0.0115113214394352));
#29568=CARTESIAN_POINT('',(0.00549591978685464,0.00256505623465993,-0.0114750995247055));
#29569=CARTESIAN_POINT('',(0.006001171735723,0.000871708284348305,-0.0114026567689));
#29570=CARTESIAN_POINT('',(0.00606469940733337,-3.09467446789897E-5,-0.0113664348888228));
#29571=CARTESIAN_POINT('',(0.00579769083551663,-0.00177788284887564,-0.0112939919806155));
#29572=CARTESIAN_POINT('',(0.00546891955221835,-0.00262079853837439,-0.011257770273707));
#29573=CARTESIAN_POINT('',(0.00448104282489471,-0.00408617269203305,-0.0111853270986528));
#29574=CARTESIAN_POINT('',(0.00382313914792685,-0.00470725474914973,-0.0111491056136164));
#29575=CARTESIAN_POINT('',(0.002303898594764,-0.00561002127132331,-0.011076662169136));
#29576=CARTESIAN_POINT('',(0.00144339105789126,-0.00588984503873103,-0.0110404408615413));
#29577=CARTESIAN_POINT('',(-0.000315828481518282,-0.00605673812410452,-0.0109679972569792));
#29578=CARTESIAN_POINT('',(-0.00121352495802194,-0.00594161716629411,-0.01093177599248));
#29579=CARTESIAN_POINT('',(-0.00287507222511445,-0.00534034338698825,-0.0108593324413081));
#29580=CARTESIAN_POINT('',(-0.00363767037747606,-0.0048525983178956,-0.0108231110050779));
#29581=CARTESIAN_POINT('',(-0.00488212214408763,-0.00359825269162657,-0.0107506678100055));
#29582=CARTESIAN_POINT('',(-0.00536350309988019,-0.00283158196363093,-0.0107144460794054));
#29583=CARTESIAN_POINT('',(-0.0059513785636077,-0.00116524705637126,-0.010642003257617));
#29584=CARTESIAN_POINT('',(-0.00605917232747766,-0.000266605506908352,-0.0106057813428858));
#29585=CARTESIAN_POINT('',(-0.00587794805600551,0.00149119555581136,-0.0105333385870834));
#29586=CARTESIAN_POINT('',(-0.0055912088468016,0.00234945104947269,-0.0104971167070027));
#29587=CARTESIAN_POINT('',(-0.00467600158780397,0.00386122980400121,-0.0104246737987992));
#29588=CARTESIAN_POINT('',(-0.00404968665904617,0.00451416703401636,-0.0103884520918877));
#29589=CARTESIAN_POINT('',(-0.0025762331591996,0.00548995216527635,-0.0103160089168357));
#29590=CARTESIAN_POINT('',(-0.00173073160428898,0.00581198832858672,-0.0102797874318002));
#29591=CARTESIAN_POINT('',(1.83374390657506E-5,0.00606464765160122,-0.0102073439873159));
#29592=CARTESIAN_POINT('',(0.00092042665972273,0.00599386912521625,-0.0101711226797231));
#29593=CARTESIAN_POINT('',(0.00260960080412948,0.00547483405930433,-0.010098679075161));
#29594=CARTESIAN_POINT('',(0.00339490932190509,0.00502494259375986,-0.0100624578106634));
#29595=CARTESIAN_POINT('',(0.00469988132061564,0.00383359144441648,-0.00999001425948835));
#29596=CARTESIAN_POINT('',(0.00521777818797358,0.00309114007954574,-0.00995379282326351));
#29597=CARTESIAN_POINT('',(0.0058874844146718,0.00145604475526363,-0.00988134962818345));
#29598=CARTESIAN_POINT('',(0.00603883024141418,0.000563516845061795,-0.0098451278975872));
#29599=CARTESIAN_POINT('',(0.00594427758822029,-0.00120094607032303,-0.00977268507579888));
#29600=CARTESIAN_POINT('',(0.00569997080779778,-0.0020724334924908,-0.00973646316106843));
#29601=CARTESIAN_POINT('',(0.00485986006847123,-0.00362707839031427,-0.00966402040526441));
#29602=CARTESIAN_POINT('',(0.00426650742376162,-0.00431027272979533,-0.00962779852518529));
#29603=CARTESIAN_POINT('',(0.00284243348642524,-0.00535673952361845,-0.00955535561698029));
#29604=CARTESIAN_POINT('',(0.00201392568252852,-0.00572029451974243,-0.00951913391007031));
#29605=CARTESIAN_POINT('',(0.000279215348634508,-0.00605793618790945,-0.00944669073501678));
#29606=CARTESIAN_POINT('',(-0.000625164136976053,-0.00603189937080213,-0.00941046924998202));
#29607=CARTESIAN_POINT('',(-0.00233778176403151,-0.00559598640309019,-0.00933802580549774));
#29608=CARTESIAN_POINT('',(-0.00314411776208609,-0.00518538097196428,-0.00930180449790574));
#29609=CARTESIAN_POINT('',(-0.00450608506039847,-0.0040594361384512,-0.00922936089334209));
#29610=CARTESIAN_POINT('',(-0.00505944951645661,-0.00334326606254395,-0.009193139628846));
#29611=CARTESIAN_POINT('',(-0.00580917608958444,-0.00174320995602507,-0.0091206960776694));
#29612=CARTESIAN_POINT('',(-0.00600352656861679,-0.000859083785322946,-0.00908447464143997));
#29613=CARTESIAN_POINT('',(-0.00599653055331361,0.000907832795992958,-0.00901203144637064));
#29614=CARTESIAN_POINT('',(-0.00579480022080864,0.00179033860487189,-0.00897580971576979));
#29615=CARTESIAN_POINT('',(-0.00503221423505353,0.00338430604441708,-0.00890336689397993));
#29616=CARTESIAN_POINT('',(-0.00447300040297218,0.00409596327929867,-0.00886714497924948));
#29617=CARTESIAN_POINT('',(-0.00310190244027584,0.00521077141945543,-0.008794702223447));
#29618=CARTESIAN_POINT('',(-0.0022922689214523,0.00561489445972799,-0.00875848034336713));
#29619=CARTESIAN_POINT('',(-0.00057613065345023,0.00603673420972755,-0.00868603743516212));
#29620=CARTESIAN_POINT('',(0.000328437222867063,0.00605555901944492,-0.00864981572825367));
#29621=CARTESIAN_POINT('',(0.00206031046767124,0.00570365434125339,-0.00857737255319708));
#29622=CARTESIAN_POINT('',(0.00288588430551185,0.00533350841312284,-0.00854115106816231));
#29623=CARTESIAN_POINT('',(0.0043013200074696,0.0042753869524458,-0.00846870762368109));
#29624=CARTESIAN_POINT('',(0.00488914543666715,0.00358746557131492,-0.00843248631608679));
#29625=CARTESIAN_POINT('',(0.00571655871398774,0.00202602586441055,-0.00836004271152468));
#29626=CARTESIAN_POINT('',(0.00595373438615279,0.00115260758008786,-0.00832382144702628));
#29627=CARTESIAN_POINT('',(0.00603407645922529,-0.000612559445933486,-0.00825137789585275));
#29628=CARTESIAN_POINT('',(0.0058752924512829,-0.00150376022759798,-0.00821515645962792));
#29629=CARTESIAN_POINT('',(0.00519265927390726,-0.00313350103358763,-0.00814271326454633));
#29630=CARTESIAN_POINT('',(0.00466856439658982,-0.00387163123167595,-0.00810649153395315));
#29631=CARTESIAN_POINT('',(0.00335404188172599,-0.0050524361020565,-0.00803404871216023));
#29632=CARTESIAN_POINT('',(0.002565056234659,-0.00549591978684913,-0.00799782679743132));
#29633=CARTESIAN_POINT('',(0.000871708284350316,-0.00600117173572815,-0.00792538404162886));
#29634=CARTESIAN_POINT('',(-3.09467446757314E-5,-0.00606469940732576,-0.0078891621615482));
#29635=CARTESIAN_POINT('',(-0.00177788284887691,-0.0057976908355244,-0.00781671925334474));
#29636=CARTESIAN_POINT('',(-0.00262079853836913,-0.00546891955220997,-0.00778049754643241));
#29637=CARTESIAN_POINT('',(-0.0040861726920387,-0.0044810428249027,-0.00770805437138196));
#29638=CARTESIAN_POINT('',(-0.00470725474913832,-0.00382313914792043,-0.00767183288634381));
#29639=CARTESIAN_POINT('',(-0.00561002127133291,-0.00230389859477328,-0.00759938944186337));
#29640=CARTESIAN_POINT('',(-0.00588984503872023,-0.00144339105788938,-0.00756316813426977));
#29641=CARTESIAN_POINT('',(-0.00605673812411518,0.000315828481515877,-0.00749072452970536));
#29642=CARTESIAN_POINT('',(-0.00594161716629604,0.0012135249580206,-0.0074545032652082));
#29643=CARTESIAN_POINT('',(-0.00534034338698797,0.00287507222511094,-0.00738205971403469));
#29644=CARTESIAN_POINT('',(-0.00485259831790225,0.00363767037748548,-0.00734583827780744));
#29645=CARTESIAN_POINT('',(-0.00359825269161942,0.00488212214407865,-0.00727339508273044));
#29646=CARTESIAN_POINT('',(-0.00283158196363257,0.005363503099875,-0.00723717335213202));
#29647=CARTESIAN_POINT('',(-0.00116524705637457,0.00595137856361104,-0.00716473053034522));
#29648=CARTESIAN_POINT('',(-0.000266605506907021,0.00605917232748146,-0.00712850861561236));
#29649=CARTESIAN_POINT('',(0.00149119555581047,0.00587794805600161,-0.0070560658598114));
#29650=CARTESIAN_POINT('',(0.00234945104945872,0.00559120884678573,-0.0070198439797293));
#29651=CARTESIAN_POINT('',(0.00386122980401202,0.00467600158782171,-0.00694740107152736));
#29652=CARTESIAN_POINT('',(0.0045141670340063,0.00404968665904241,-0.00691117936461584));
#29653=CARTESIAN_POINT('',(0.00548995216528485,0.00257623315920559,-0.0068387361895623));
#29654=CARTESIAN_POINT('',(0.00581198832858654,0.00173073160428969,-0.00680251470452446));
#29655=CARTESIAN_POINT('',(0.00606464765160107,-1.83374390644384E-5,-0.0067300712600463));
#29656=CARTESIAN_POINT('',(0.00599386912521984,-0.000920426659723841,-0.00669384995245127));
#29657=CARTESIAN_POINT('',(0.00547483405930049,-0.00260960080412893,-0.00662140634788747));
#29658=CARTESIAN_POINT('',(0.00502494259376497,-0.00339490932190835,-0.0065851850833907));
#29659=CARTESIAN_POINT('',(0.00383359144441144,-0.00469988132061221,-0.00651274153221563));
#29660=CARTESIAN_POINT('',(0.00309114007954164,-0.00521777818796783,-0.00647652009599003));
#29661=CARTESIAN_POINT('',(0.00145604475526746,-0.00588748441467761,-0.0064040769009115));
#29662=CARTESIAN_POINT('',(0.000563516845063924,-0.00603883024140614,-0.00636785517031527));
#29663=CARTESIAN_POINT('',(-0.00120094607032435,-0.00594427758822836,-0.00629541234852541));
#29664=CARTESIAN_POINT('',(-0.00207243349248784,-0.00569997080779289,-0.00625919043379578));
#29665=CARTESIAN_POINT('',(-0.0036270783903172,-0.00485986006847613,-0.00618674767799164));
#29666=CARTESIAN_POINT('',(-0.0043102727297894,-0.00426650742375841,-0.0061505257979118));
#29667=CARTESIAN_POINT('',(-0.0053567395236248,-0.00284243348642777,-0.00607808288970833));
#29668=CARTESIAN_POINT('',(-0.00572029451974054,-0.00201392568252749,-0.00604186118279835));
#29669=CARTESIAN_POINT('',(-0.0060579361879114,-0.000279215348635194,-0.00596941800774329));
#29670=CARTESIAN_POINT('',(-0.00603189937080701,0.000625164136977491,-0.00593319652270699));
#29671=CARTESIAN_POINT('',(-0.0055959864030851,0.00233778176403084,-0.00586075307822731));
#29672=CARTESIAN_POINT('',(-0.00518538097195793,0.00314411776208208,-0.00582453177063385));
#29673=CARTESIAN_POINT('',(-0.00405943613845727,0.00450608506040282,-0.00575208816606853));
#29674=CARTESIAN_POINT('',(-0.00334326606254177,0.00505944951645318,-0.00571586690157174));
#29675=CARTESIAN_POINT('',(-0.00174320995602712,0.00580917608958792,-0.00564342335039822));
#29676=CARTESIAN_POINT('',(-0.000859083785322943,0.00600352656860298,-0.00560720191417491));
#29677=CARTESIAN_POINT('',(0.000907832795993349,0.00599653055332741,-0.00553475871909025));
#29678=CARTESIAN_POINT('',(0.00179033860487224,0.00579480022080926,-0.00549853698849628));
#29679=CARTESIAN_POINT('',(0.00338430604441741,0.00503221423505262,-0.00542609416670796));
#29680=CARTESIAN_POINT('',(0.00409596327930708,0.00447300040297686,-0.00538987225197682));
#29681=CARTESIAN_POINT('',(0.00521077141944732,0.00310190244027081,-0.00531742949617421));
#29682=CARTESIAN_POINT('',(0.00561489445973345,0.00229226892145273,-0.00528120761609439));
#29683=CARTESIAN_POINT('',(0.00603673420972227,0.000576130653449121,-0.00520876470788938));
#29684=CARTESIAN_POINT('',(0.00605555901943846,-0.000328437222866894,-0.00517254300097944));
#29685=CARTESIAN_POINT('',(0.00570365434125996,-0.00206031046767069,-0.00510009982592591));
#29686=CARTESIAN_POINT('',(0.0053335084131272,-0.00288588430551483,-0.00506387834089111));
#29687=CARTESIAN_POINT('',(0.00427538695244096,-0.0043013200074672,-0.00499143489640682));
#29688=CARTESIAN_POINT('',(0.0035874655713107,-0.00488914543666087,-0.00495521358881489));
#29689=CARTESIAN_POINT('',(0.0020260258644141,-0.00571655871399437,-0.00488276998425111));
#29690=CARTESIAN_POINT('',(0.00115260758008779,-0.0059537343861532,-0.00484654871975433));
#29691=CARTESIAN_POINT('',(-0.000612559445933405,-0.00603407645922492,-0.00477410516857927));
#29692=CARTESIAN_POINT('',(-0.00150376022759912,-0.00587529245128513,-0.00473788373235367));
#29693=CARTESIAN_POINT('',(-0.00313350103358697,-0.00519265927390485,-0.00466544053727514));
#29694=CARTESIAN_POINT('',(-0.0038716312316762,-0.0046685643965911,-0.00462921880667965));
#29695=CARTESIAN_POINT('',(-0.00505243610205692,-0.00335404188172401,-0.00455677598488826));
#29696=CARTESIAN_POINT('',(-0.00549591978685125,-0.00256505623465877,-0.00452055407015787));
#29697=CARTESIAN_POINT('',(-0.00600117173572664,-0.000871708284348603,-0.0044481113143568));
#29698=CARTESIAN_POINT('',(-0.00606469940732523,3.09467446769893E-5,-0.00441188943427621));
#29699=CARTESIAN_POINT('',(-0.0057976908355246,0.00177788284887812,-0.00433944652607121));
#29700=CARTESIAN_POINT('',(-0.00546891955221376,0.00262079853837175,-0.00430322481915968));
#29701=CARTESIAN_POINT('',(-0.00448104282489869,0.00408617269203654,-0.00423078164410923));
#29702=CARTESIAN_POINT('',(-0.00382313914792086,0.00470725474914317,-0.0041945601590714));
#29703=CARTESIAN_POINT('',(-0.00230389859476928,0.00561002127133021,-0.00412211671459019));
#29704=CARTESIAN_POINT('',(-0.00144339105789001,0.0058898450387264,-0.00408589540699673));
#29705=CARTESIAN_POINT('',(0.000315828481517189,0.00605673812410911,-0.00401345180243295));
#29706=CARTESIAN_POINT('',(0.0012135249580228,0.00594161716629725,-0.0039772305379354));
#29707=CARTESIAN_POINT('',(0.002875072225113,0.00534034338698525,-0.00390478698676188));
#29708=CARTESIAN_POINT('',(0.00363767037748591,0.00485259831790412,-0.00386856555053472));
#29709=CARTESIAN_POINT('',(0.00488212214407839,0.00359825269161736,-0.00379612235545772));
#29710=CARTESIAN_POINT('',(0.00536350309987848,0.00283158196362959,-0.00375990062486069));
#29711=CARTESIAN_POINT('',(0.00595137856360991,0.00116524705637084,-0.00368745780307082));
#29712=CARTESIAN_POINT('',(0.00605917232748467,0.000266605506905886,-0.00365123588834047));
#29713=CARTESIAN_POINT('',(0.00587794805599835,-0.00149119555580979,-0.00357879313253784));
#29714=CARTESIAN_POINT('',(0.0055912088467858,-0.00234945104946311,-0.00354257125245874));
#29715=CARTESIAN_POINT('',(0.00467600158781796,-0.00386122980401372,-0.00347012834425219));
#29716=CARTESIAN_POINT('',(0.00404968665903719,-0.00451416703400542,-0.00343390663734299));
#29717=CARTESIAN_POINT('',(0.00257623315920537,-0.00548995216528933,-0.00336146346228945));
#29718=CARTESIAN_POINT('',(0.00173073160428629,-0.00581198832858667,-0.0033252419772539));
#29719=CARTESIAN_POINT('',(-1.83374390680346E-5,-0.00606464765160196,-0.00325279853277114));
#29720=CARTESIAN_POINT('',(-0.000920426659724022,-0.00599386912522055,-0.00321657722517854));
#29721=CARTESIAN_POINT('',(-0.00260960080412909,-0.00547483405929967,-0.00314413362061474));
#29722=CARTESIAN_POINT('',(-0.00339490932190975,-0.00502494259376035,-0.00310791235611861));
#29723=CARTESIAN_POINT('',(-0.00469988132061588,-0.00383359144441144,-0.00303546880494201));
#29724=CARTESIAN_POINT('',(-0.00521777818796983,-0.00309114007954222,-0.00299924736871654));
#29725=CARTESIAN_POINT('',(-0.00588748441467571,-0.00145604475526665,-0.00292680417363955));
#29726=CARTESIAN_POINT('',(-0.00603883024140671,-0.000563516845059997,-0.00289058244304164));
#29727=CARTESIAN_POINT('',(-0.00594427758822741,0.00120094607032737,-0.00281813962125333));
#29728=CARTESIAN_POINT('',(-0.00569997080779323,0.00207243349248791,-0.00278191770652306));
#29729=CARTESIAN_POINT('',(-0.00485986006847584,0.00362707839031703,-0.00270947495071892));
#29730=CARTESIAN_POINT('',(-0.00426650742375889,0.00431027272979482,-0.002673253070639));
#29731=CARTESIAN_POINT('',(-0.00284243348642429,0.00535673952362161,-0.00260081016243554));
#29732=CARTESIAN_POINT('',(-0.00201392568252745,0.00572029451974175,-0.00256458845552562));
#29733=CARTESIAN_POINT('',(-0.000279215348634867,0.00605793618791026,-0.00249214528047057));
#29734=CARTESIAN_POINT('',(0.00062516413697907,0.00603189937080894,-0.0024559237954365));
#29735=CARTESIAN_POINT('',(0.00233778176403195,0.00559598640308249,-0.00238348035095223));
#29736=CARTESIAN_POINT('',(0.00314411776208378,0.00518538097195793,-0.00234725904336031));
#29737=CARTESIAN_POINT('',(0.00450608506040276,0.00405943613845593,-0.00227481543879654));
#29738=CARTESIAN_POINT('',(0.0050594495164604,0.00334326606254532,-0.002238594174299));
#29739=CARTESIAN_POINT('',(0.00580917608958121,0.00174320995602248,-0.00216615062312549));
#29740=CARTESIAN_POINT('',(0.00600352656860681,0.000859083785322374,-0.00212992918689912));
#29741=CARTESIAN_POINT('',(0.00599653055332356,-0.000907832795993293,-0.00205748599182059));
#29742=CARTESIAN_POINT('',(0.00579480022080894,-0.00179033860487247,-0.00202126426122357));
#29743=CARTESIAN_POINT('',(0.00503221423505307,-0.00338430604441687,-0.00194882143943525));
#29744=CARTESIAN_POINT('',(0.00447300040297654,-0.00409596327930717,-0.00191259952470409));
#29745=CARTESIAN_POINT('',(0.00310190244027087,-0.00521077141944741,-0.00184015676890149));
#29746=CARTESIAN_POINT('',(0.00229226892145273,-0.00561489445973389,-0.0018039348888209));
#29747=CARTESIAN_POINT('',(0.000576130653448751,-0.00603673420972194,-0.00173149198061743));
#29748=CARTESIAN_POINT('',(-0.000328437222867711,-0.00605555901944176,-0.00169527027370514));
#29749=CARTESIAN_POINT('',(-0.00206031046767129,-0.00570365434125637,-0.00162282709865468));
#29750=CARTESIAN_POINT('',(-0.00288588430551477,-0.00533350841312699,-0.00158660561361686));
#29751=CARTESIAN_POINT('',(-0.00430132000746675,-0.00427538695244153,-0.00151416216913565));
#29752=CARTESIAN_POINT('',(-0.00488914543666364,-0.00358746557131148,-0.00147794086154216));
#29753=CARTESIAN_POINT('',(-0.00571655871399177,-0.00202602586441296,-0.00140549725697838));
#29754=CARTESIAN_POINT('',(-0.00595373438615588,-0.00115260758008819,-0.00136927599248006));
#29755=CARTESIAN_POINT('',(-0.00603407645922224,0.000612559445934199,-0.00129683244130807));
#29756=CARTESIAN_POINT('',(-0.00587529245128122,0.00150376022759815,-0.0012606110050794));
#29757=CARTESIAN_POINT('',(-0.00519265927390861,0.0031335010335883,-0.00118816781000394));
#29758=CARTESIAN_POINT('',(-0.00466856439659019,0.00387163123167518,-0.00115194607940538));
#29759=CARTESIAN_POINT('',(-0.00335404188172464,0.00505243610205819,-0.00107950325761706));
#29760=CARTESIAN_POINT('',(-0.00256505623465843,0.00549591978684937,-0.00104328134288591));
#29761=CARTESIAN_POINT('',(-0.000871708284348645,0.00600117173572859,-0.000970838587083295));
#29762=CARTESIAN_POINT('',(3.09467446766596E-5,0.0060646994073229,-0.000934616707003476));
#29763=CARTESIAN_POINT('',(0.00177788284887884,0.00579769083552687,-0.000862173798798473));
#29764=CARTESIAN_POINT('',(0.00262079853837167,0.00546891955221328,-0.000825952091889253));
#29765=CARTESIAN_POINT('',(0.00408617269203685,0.00448104282489897,-0.00075350891683419));
#29766=CARTESIAN_POINT('',(0.00470725474914363,0.00382313914792303,-0.000717287431798667));
#29767=CARTESIAN_POINT('',(0.00561002127132991,0.00230389859476685,-0.000644843987317453));
#29768=CARTESIAN_POINT('',(0.00588984503872567,0.00144339105788941,-0.000608622679723984));
#29769=CARTESIAN_POINT('',(0.00605673812410992,-0.000315828481517504,-0.0005361790751602));
#29770=CARTESIAN_POINT('',(0.00594161716629623,-0.00121352495802331,-0.000499957810662642));
#29771=CARTESIAN_POINT('',(0.00534034338698577,-0.00287507222511389,-0.000427514259489119));
#29772=CARTESIAN_POINT('',(0.00485259831790474,-0.00363767037748681,-0.000391292823261212));
#29773=CARTESIAN_POINT('',(0.00359825269161654,-0.00488212214407767,-0.000318849628185754));
#29774=CARTESIAN_POINT('',(0.00283158196363021,-0.00536350309988268,-0.000282627897588721));
#29775=CARTESIAN_POINT('',(0.00116524705637054,-0.00595137856360559,-0.000210185075797331));
#29776=CARTESIAN_POINT('',(0.000266605506906044,-0.00605917232748427,-0.000173963161068493));
#29777=CARTESIAN_POINT('',(-0.00149119555581014,-0.00587794805599875,-0.000101520405264349));
#29778=CARTESIAN_POINT('',(-0.00234945104946307,-0.00559120884678631,-6.52985251845243E-5));
#29779=CARTESIAN_POINT('',(-0.00386122980401153,-0.0046760015878186,7.14438301894512E-6));
#29780=CARTESIAN_POINT('',(-0.00451416703400858,-0.00404968665904013,4.33660899304402E-5));
#29781=CARTESIAN_POINT('',(-0.00548995216528468,-0.00257623315920546,0.000115809264982434));
#29782=CARTESIAN_POINT('',(-0.00581198832858678,-0.00173073160428641,0.000152030750019587));
#29783=CARTESIAN_POINT('',(-0.00606464765160127,1.83374390675391E-5,0.000224474194500801));
#29784=CARTESIAN_POINT('',(-0.00599386912521991,0.000920426659714502,0.000260695502093955));
#29785=CARTESIAN_POINT('',(-0.00547483405929987,0.00260960080412699,0.000333139106657739));
#29786=CARTESIAN_POINT('',(-0.00502494259376105,0.0033949093219533,0.000369360371157798));
#29787=CARTESIAN_POINT('',(-0.00383359144441966,0.00469988132060065,0.000441803922327982));
#29788=CARTESIAN_POINT('',(-0.00309114007952168,0.00521777818772337,0.000478025358548409));
#29789=CARTESIAN_POINT('',(-0.00145604475525611,0.00588748441486752,0.000550468553641278));
#29790=CARTESIAN_POINT('',(-0.000563516845067593,0.00603883024251221,0.000586690284260184));
#29791=CARTESIAN_POINT('',(0.00120094607027949,0.00594427758669178,0.000659133105962878));
#29792=CARTESIAN_POINT('',(0.00207243349184227,0.00569997080483151,0.000695355020696328));
#29793=CARTESIAN_POINT('',(0.0036270783914194,0.00485986007638553,0.000767797776819668));
#29794=CARTESIAN_POINT('',(0.00431027273332751,0.0042665074258414,0.000804019656535012));
#29795=CARTESIAN_POINT('',(0.00535673951349427,0.00284243345423534,0.000876462563765694));
#29796=CARTESIAN_POINT('',(0.00572029451211937,0.00201392571479105,0.000912684273444742));
#29797=CARTESIAN_POINT('',(0.00605793624792242,0.000279215448155177,0.0009851274504376));
#29798=CARTESIAN_POINT('',(0.0060318993545859,-0.000625164387659044,0.00102134892034041));
#29799=CARTESIAN_POINT('',(0.0055959861469186,-0.00233778194385103,0.00109379236698234));
#29800=CARTESIAN_POINT('',(0.00518538116262535,-0.00314411648770142,0.00113001374476538));
#29801=CARTESIAN_POINT('',(0.00405943692929677,-0.00450608539393174,0.00120245729547706));
#29802=CARTESIAN_POINT('',(0.00334326536337128,-0.00505945513492329,0.00123867827021172));
#29803=CARTESIAN_POINT('',(0.00174320839046504,-0.00580917059968966,0.00131112223223615));
#29804=CARTESIAN_POINT('',(0.000859084702433251,-0.00600351044798021,0.00134734474006646));
#29805=CARTESIAN_POINT('',(-0.00159496641848697,-0.00599385800234282,0.00144795686576414));
#29806=CARTESIAN_POINT('',(-0.00315377058881324,-0.00533975389994977,0.00151238270347832));
#29807=CARTESIAN_POINT('',(-0.00536605961859909,-0.00311114458504296,0.0016411109293347));
#29808=CARTESIAN_POINT('',(-0.00600625207018257,-0.00153637595212074,0.00170594725770846));
#29809=CARTESIAN_POINT('',(-0.00600005712193031,2.43712307539645E-5,0.00176992864208601));
#29810=CARTESIAN_POINT('',(-0.00719,2.43712308653001E-5,-0.0152300713606537));
#29811=CARTESIAN_POINT('',(-0.00718690252158388,0.000963531398886715,-0.0151977711561101));
#29812=CARTESIAN_POINT('',(-0.0069976071514561,0.00190126501000997,-0.0151659831835772));
#29813=CARTESIAN_POINT('',(-0.00581496217549105,0.00473548102193302,-0.0150600404237794));
#29814=CARTESIAN_POINT('',(-0.00409179418652758,0.00628072180483626,-0.0149883589919571));
#29815=CARTESIAN_POINT('',(-0.00104907375728438,0.0071909123572038,-0.0148798167218509));
#29816=CARTESIAN_POINT('',(3.35199355820819E-5,0.0072673711660381,-0.0148435071276401));
#29817=CARTESIAN_POINT('',(0.00212523469640938,0.00694911971731699,-0.0147712812165734));
#29818=CARTESIAN_POINT('',(0.00313717278285731,0.0065550974911468,-0.0147348400891705));
#29819=CARTESIAN_POINT('',(0.00489205526552821,0.00537377185160928,-0.0146626838737225));
#29820=CARTESIAN_POINT('',(0.00563810694958756,0.00458471263506918,-0.0146262525303834));
#29821=CARTESIAN_POINT('',(0.00672019040191557,0.00276650918727105,-0.0145540354134981));
#29822=CARTESIAN_POINT('',(0.00705682503309421,0.00173471416688417,-0.0145176922841528));
#29823=CARTESIAN_POINT('',(0.00725818458114715,-0.000372723806555423,-0.0144453173457367));
#29824=CARTESIAN_POINT('',(0.00712145806485822,-0.00144818128856786,-0.0144091498714224));
#29825=CARTESIAN_POINT('',(0.00640171586403277,-0.00344126714619258,-0.0143365118456955));
#29826=CARTESIAN_POINT('',(0.00581957894570077,-0.0043536033968103,-0.0143006028835282));
#29827=CARTESIAN_POINT('',(0.00431418951861804,-0.00584909993211931,-0.0142276072565402));
#29828=CARTESIAN_POINT('',(0.00339778105700325,-0.00642487333100277,-0.0141916978952334));
#29829=CARTESIAN_POINT('',(0.00139990793722036,-0.00713121855168838,-0.0141190607367982));
#29830=CARTESIAN_POINT('',(0.000323505481587939,-0.00726061866847718,-0.0140828927954176));
#29831=CARTESIAN_POINT('',(-0.00178251377698793,-0.0070449290461279,-0.0140105181722345));
#29832=CARTESIAN_POINT('',(-0.0028120565804278,-0.00670137988269372,-0.0139741743072064));
#29833=CARTESIAN_POINT('',(-0.00462280125024691,-0.00560685742263364,-0.0139019595234403));
#29834=CARTESIAN_POINT('',(-0.00540689443549387,-0.00485556846586822,-0.0138655268071655));
#29835=CARTESIAN_POINT('',(-0.00657611983919041,-0.00309261239607272,-0.0137933655081125));
#29836=CARTESIAN_POINT('',(-0.0069634263845761,-0.00207811329688733,-0.013756933013686));
#29837=CARTESIAN_POINT('',(-0.00726734342674198,1.57849886640124E-5,-0.0136847176936322));
#29838=CARTESIAN_POINT('',(-0.00718350233401541,0.00109786333180735,-0.0136483744011382));
#29839=CARTESIAN_POINT('',(-0.00656305309032847,0.0031219388582032,-0.0135759989297099));
#29840=CARTESIAN_POINT('',(-0.00602517442190881,0.00406320899944549,-0.0135398316374257));
#29841=CARTESIAN_POINT('',(-0.00459749831080525,0.00562914687378522,-0.0134671937474946));
#29842=CARTESIAN_POINT('',(-0.00371053796164551,0.00624926153808826,-0.0134312846976163));
#29843=CARTESIAN_POINT('',(-0.00174743776495843,0.00705483255841795,-0.0133582890604163));
#29844=CARTESIAN_POINT('',(-0.000680447802063153,0.00723608348462041,-0.0133223797161986));
#29845=CARTESIAN_POINT('',(0.00143565290426297,0.0071241084384027,-0.0132497425555768));
#29846=CARTESIAN_POINT('',(0.00247963838116558,0.00683173716884005,-0.0132135746131063));
#29847=CARTESIAN_POINT('',(0.00434280562235721,0.00582652726309188,-0.0131411999903939));
#29848=CARTESIAN_POINT('',(0.0051625085739271,0.00511514024919255,-0.0131048561254624));
#29849=CARTESIAN_POINT('',(0.0064165629013809,0.00341099136485625,-0.0130326413416085));
#29850=CARTESIAN_POINT('',(0.00685346470998661,0.00241683140327179,-0.012996208625354));
#29851=CARTESIAN_POINT('',(0.00725903404947283,0.000340629183026168,-0.0129240473262826));
#29852=CARTESIAN_POINT('',(0.00722862664215364,-0.000744861568632379,-0.0128876148318792));
#29853=CARTESIAN_POINT('',(0.00670810919405929,-0.00279567535467164,-0.0128153995118028));
#29854=CARTESIAN_POINT('',(0.00621655667007348,-0.00376330079134388,-0.0127790562192913));
#29855=CARTESIAN_POINT('',(0.00486875614303342,-0.00539586709624065,-0.0127066807479202));
#29856=CARTESIAN_POINT('',(0.00401161256188436,-0.00605965005927627,-0.0126705134556151));
#29857=CARTESIAN_POINT('',(0.00209335334315847,-0.00696004001606565,-0.0125978755656686));
#29858=CARTESIAN_POINT('',(0.0010366012222284,-0.00719352623142796,-0.0125619665158032));
#29859=CARTESIAN_POINT('',(-0.00108534555283455,-0.00718653088776051,-0.0124889708785929));
#29860=CARTESIAN_POINT('',(-0.00214047746751151,-0.00694566552742465,-0.0124530615343699));
#29861=CARTESIAN_POINT('',(-0.00405264860378823,-0.00603241739253837,-0.0123804243737688));
#29862=CARTESIAN_POINT('',(-0.004905279777168,-0.00536278561505436,-0.0123442564313078));
#29863=CARTESIAN_POINT('',(-0.00624194467998763,-0.00372108952233651,-0.012271881808556));
#29864=CARTESIAN_POINT('',(-0.00672701543546455,-0.00275016688146852,-0.0122355379436288));
#29865=CARTESIAN_POINT('',(-0.007233461016919,-0.000695832792475087,-0.0121633231598056));
#29866=CARTESIAN_POINT('',(-0.0072566571092172,0.000389846331801014,-0.0121268904434963));
#29867=CARTESIAN_POINT('',(-0.00683682612901503,0.00246321173532615,-0.0120547291445039));
#29868=CARTESIAN_POINT('',(-0.00639333402113541,0.00345443801252094,-0.0120182966500488));
#29869=CARTESIAN_POINT('',(-0.0051276261457341,0.00514994949078618,-0.0119460813299969));
#29870=CARTESIAN_POINT('',(-0.00430319660631132,0.00585580981978926,-0.0119097380375061));
#29871=CARTESIAN_POINT('',(-0.00243323520837243,0.00684832348254616,-0.011837362566069));
#29872=CARTESIAN_POINT('',(-0.00138731905467814,0.00713356432844445,-0.0118011952738008));
#29873=CARTESIAN_POINT('',(0.000729485694685875,0.00723133015881769,-0.0117285573838467));
#29874=CARTESIAN_POINT('',(0.00179514865645682,0.00704264176550971,-0.0116926483340046));
#29875=CARTESIAN_POINT('',(0.00375289484889381,0.0062241450355068,-0.0116196526967552));
#29876=CARTESIAN_POINT('',(0.00463553444612515,0.00559783295629068,-0.0115837433525595));
#29877=CARTESIAN_POINT('',(0.00605266529073645,0.00402234548266771,-0.011511106191943));
#29878=CARTESIAN_POINT('',(0.00658413679358073,0.00307739856515859,-0.0114749382494755));
#29879=CARTESIAN_POINT('',(0.00719080424344732,0.00104914963355636,-0.011402563626752));
#29880=CARTESIAN_POINT('',(0.00726739517750182,-3.34944636365538E-5,-0.0113662197617896));
#29881=CARTESIAN_POINT('',(0.00694913026411556,-0.00212526001481188,-0.0112940049780086));
#29882=CARTESIAN_POINT('',(0.00655508924530735,-0.00313717349682351,-0.0112575722616862));
#29883=CARTESIAN_POINT('',(0.0053737734064212,-0.004892050996048,-0.0111854109626777));
#29884=CARTESIAN_POINT('',(0.00458471425112067,-0.00563810758356804,-0.0111489784682096));
#29885=CARTESIAN_POINT('',(0.00276650849876566,-0.00672019050133081,-0.0110767631481999));
#29886=CARTESIAN_POINT('',(0.00173471386783323,-0.00705682488623721,-0.0110404198556641));
#29887=CARTESIAN_POINT('',(-0.000372723729448532,-0.00725818469882193,-0.0109680443842746));
#29888=CARTESIAN_POINT('',(-0.00144818120252657,-0.00712145809453435,-0.010931877091978));
#29889=CARTESIAN_POINT('',(-0.00344126714832045,-0.00640171583705778,-0.0108592392020331));
#29890=CARTESIAN_POINT('',(-0.00435360342524517,-0.00581957893249035,-0.0108233301522186));
#29891=CARTESIAN_POINT('',(-0.00584909992429929,-0.00431418952362129,-0.0107503345149048));
#29892=CARTESIAN_POINT('',(-0.00642487332654239,-0.0033977810620425,-0.0107144251707447));
#29893=CARTESIAN_POINT('',(-0.00713121855472189,-0.00139990793571158,-0.0106417880101213));
#29894=CARTESIAN_POINT('',(-0.00726061866850349,-0.000323505480401984,-0.0106056200676768));
#29895=CARTESIAN_POINT('',(-0.00704492904566077,0.00178251377636469,-0.0105332454449142));
#29896=CARTESIAN_POINT('',(-0.00670137988286316,0.00281205658029061,-0.0104969015799504));
#29897=CARTESIAN_POINT('',(-0.00560685742262686,0.00462280125036886,-0.0104246867962115));
#29898=CARTESIAN_POINT('',(-0.00485556846583809,0.00540689443551145,-0.0103882540798553));
#29899=CARTESIAN_POINT('',(-0.00309261239607019,0.00657611983916619,-0.0103160927808721));
#29900=CARTESIAN_POINT('',(-0.00207811329689743,0.00696342638457955,-0.0102796602864091));
#29901=CARTESIAN_POINT('',(1.57849886665503E-5,0.00726734342673879,-0.0102074449663641));
#29902=CARTESIAN_POINT('',(0.00109786333180936,0.00718350233401516,-0.0101711016738655));
#29903=CARTESIAN_POINT('',(0.00312193885820439,0.00656305309032835,-0.0100987262024368));
#29904=CARTESIAN_POINT('',(0.00406320899944281,0.00602517442190682,-0.0100625589101613));
#29905=CARTESIAN_POINT('',(0.00562914687378771,0.00459749831080728,-0.00998992102021339));
#29906=CARTESIAN_POINT('',(0.00624926153807862,0.00371053796164257,-0.00995401197036094));
#29907=CARTESIAN_POINT('',(0.00705483255842778,0.0017474377649609,-0.00988101633312613));
#29908=CARTESIAN_POINT('',(0.00723608348462659,0.000680447802062776,-0.00984510698891086));
#29909=CARTESIAN_POINT('',(0.00712410843839661,-0.00143565290426201,-0.00977246982831896));
#29910=CARTESIAN_POINT('',(0.00683173716884047,-0.00247963838116534,-0.00973630188583411));
#29911=CARTESIAN_POINT('',(0.00582652726309132,-0.00434280562235769,-0.00966392726312063));
#29912=CARTESIAN_POINT('',(0.00511514024919991,-0.0051625085739379,-0.00962758339816522));
#29913=CARTESIAN_POINT('',(0.00341099136485094,-0.00641656290136858,-0.00955536861436036));
#29914=CARTESIAN_POINT('',(0.00241683140327399,-0.00685346470999972,-0.00951893589805603));
#29915=CARTESIAN_POINT('',(0.000340629183027104,-0.00725903404945911,-0.00944677459903517));
#29916=CARTESIAN_POINT('',(-0.000744861568630721,-0.00722862664215674,-0.00941034210460012));
#29917=CARTESIAN_POINT('',(-0.00279567535466896,-0.00670810919405725,-0.00933812678453669));
#29918=CARTESIAN_POINT('',(-0.003763300791342,-0.00621655667006781,-0.00930178349202818));
#29919=CARTESIAN_POINT('',(-0.00539586709624276,-0.00486875614303888,-0.00922940802063791));
#29920=CARTESIAN_POINT('',(-0.00605965005927444,-0.0040116125618859,-0.00919324072834359));
#29921=CARTESIAN_POINT('',(-0.00696004001606482,-0.00209335334316259,-0.00912060283839487));
#29922=CARTESIAN_POINT('',(-0.00719352623142277,-0.00103660122222813,-0.00908469378853435));
#29923=CARTESIAN_POINT('',(-0.00718653088776567,0.00108534555283507,-0.00901169815131639));
#29924=CARTESIAN_POINT('',(-0.00694566552741994,0.00214047746750466,-0.00897578880710958));
#29925=CARTESIAN_POINT('',(-0.00603241739254579,0.00405264860378935,-0.00890315164648391));
#29926=CARTESIAN_POINT('',(-0.00536278561505002,0.00490527977716321,-0.00886698370404469));
#29927=CARTESIAN_POINT('',(-0.00372108952234035,0.00624194467999285,-0.00879460908127369));
#29928=CARTESIAN_POINT('',(-0.00275016688147031,0.00672701543546056,-0.00875826521636245));
#29929=CARTESIAN_POINT('',(-0.000695832792478314,0.00723346101692167,-0.0086860504325269));
#29930=CARTESIAN_POINT('',(0.000389846331799902,0.00725665710921006,-0.00864961771623937));
#29931=CARTESIAN_POINT('',(0.00246321173532715,0.00683682612902217,-0.00857745641721546));
#29932=CARTESIAN_POINT('',(0.00345443801251805,0.00639333402113446,-0.0085410239227796));
#29933=CARTESIAN_POINT('',(0.00514994949078697,0.00512762614573659,-0.00846880860272078));
#29934=CARTESIAN_POINT('',(0.00585580981979626,0.00430319660631894,-0.00843246531021346));
#29935=CARTESIAN_POINT('',(0.00684832348253835,0.00243323520836634,-0.00836008983881627));
#29936=CARTESIAN_POINT('',(0.00713356432844592,0.00138731905467778,-0.0083239225465243));
#29937=CARTESIAN_POINT('',(0.00723133015881612,-0.000729485694684936,-0.00825128465657788));
#29938=CARTESIAN_POINT('',(0.00704264176550677,-0.0017951486564551,-0.00821537560673844));
#29939=CARTESIAN_POINT('',(0.00622414503550962,-0.00375289484889564,-0.00814237996947601));
#29940=CARTESIAN_POINT('',(0.00559783295628793,-0.00463553444612385,-0.00810647062529255));
#29941=CARTESIAN_POINT('',(0.00402234548267076,-0.00605266529073742,-0.00803383346466462));
#29942=CARTESIAN_POINT('',(0.00307739856515751,-0.006584136793575,-0.00799766552221159));
#29943=CARTESIAN_POINT('',(0.00104914963355874,-0.00719080424345263,-0.00792529089947053));
#29944=CARTESIAN_POINT('',(-3.34944636342081E-5,-0.00726739517749434,-0.00788894703453013));
#29945=CARTESIAN_POINT('',(-0.00212526001481185,-0.00694913026412326,-0.00781673225072299));
#29946=CARTESIAN_POINT('',(-0.00313717349682018,-0.00655508924529774,-0.00778029953442967));
#29947=CARTESIAN_POINT('',(-0.0048920509960518,-0.00537377340643036,-0.0077081382353889));
#29948=CARTESIAN_POINT('',(-0.00563810758355737,-0.00458471425111287,-0.00767170574096235));
#29949=CARTESIAN_POINT('',(-0.00672019050133935,-0.00276650849877687,-0.007599490420902));
#29950=CARTESIAN_POINT('',(-0.0070568248862266,-0.0017347138678294,-0.00756314712841486));
#29951=CARTESIAN_POINT('',(-0.00725818469883238,0.00037272372944407,-0.00749077165697859));
#29952=CARTESIAN_POINT('',(-0.00712145809453643,0.00144818120252497,-0.00745460436470009));
#29953=CARTESIAN_POINT('',(-0.00640171583705767,0.00344126714831625,-0.00738196647476595));
#29954=CARTESIAN_POINT('',(-0.00581957893249744,0.00435360342525378,-0.00734605742492407));
#29955=CARTESIAN_POINT('',(-0.00431418952361361,0.00584909992429122,-0.00727306178765397));
#29956=CARTESIAN_POINT('',(-0.00339778106204424,0.00642487332653685,-0.0072371524434806));
#29957=CARTESIAN_POINT('',(-0.00139990793571579,0.00713121855472527,-0.00716451528284037));
#29958=CARTESIAN_POINT('',(-0.000323505480400539,0.0072606186685073,-0.0071283473403949));
#29959=CARTESIAN_POINT('',(0.00178251377636377,0.00704492904565687,-0.00705597271765075));
#29960=CARTESIAN_POINT('',(0.00281205658027764,0.00670137988284672,-0.00701962885271883));
#29961=CARTESIAN_POINT('',(0.00462280125037804,0.00560685742264555,-0.00694741406889786));
#29962=CARTESIAN_POINT('',(0.00540689443550218,0.00485556846583332,-0.00691098135260347));
#29963=CARTESIAN_POINT('',(0.0065761198391736,0.00309261239607762,-0.00683882005357878));
#29964=CARTESIAN_POINT('',(0.00696342638457993,0.00207811329689597,-0.00680238755913261));
#29965=CARTESIAN_POINT('',(0.00726734342673805,-1.57849886626648E-5,-0.00673017223909525));
#29966=CARTESIAN_POINT('',(0.00718350233401858,-0.00109786333181072,-0.00669382894658713));
#29967=CARTESIAN_POINT('',(0.00656305309032466,-0.00312193885820372,-0.00662145347516986));
#29968=CARTESIAN_POINT('',(0.00602517442191273,-0.00406320899944546,-0.00658528618287567));
#29969=CARTESIAN_POINT('',(0.00459749831080146,-0.00562914687378486,-0.00651264829295377));
#29970=CARTESIAN_POINT('',(0.00371053796163789,-0.00624926153807326,-0.00647673924310246));
#29971=CARTESIAN_POINT('',(0.00174743776496527,-0.00705483255843322,-0.00640374360583926));
#29972=CARTESIAN_POINT('',(0.000680447802063739,-0.00723608348461835,-0.00636783426165505));
#29973=CARTESIAN_POINT('',(-0.001435652904262,-0.00712410843840487,-0.00629519710102939));
#29974=CARTESIAN_POINT('',(-0.00247963838116228,-0.00683173716883558,-0.00625902915857182));
#29975=CARTESIAN_POINT('',(-0.00434280562236072,-0.00582652726309626,-0.0061866545358375));
#29976=CARTESIAN_POINT('',(-0.00516250857393213,-0.00511514024919673,-0.00615031067090406));
#29977=CARTESIAN_POINT('',(-0.0064165629013749,-0.00341099136485332,-0.00607809588707619));
#29978=CARTESIAN_POINT('',(-0.00685346470999765,-0.00241683140327485,-0.00604166317078753));
#29979=CARTESIAN_POINT('',(-0.00725903404946125,-0.000340629183025838,-0.00596950187175825));
#29980=CARTESIAN_POINT('',(-0.00722862664216142,0.000744861568631085,-0.00593306937731475));
#29981=CARTESIAN_POINT('',(-0.00670810919405233,0.00279567535466952,-0.00586085405727664));
#29982=CARTESIAN_POINT('',(-0.00621655667006064,0.00376330079133864,-0.00582451076477202));
#29983=CARTESIAN_POINT('',(-0.00486875614304572,0.00539586709624651,-0.00575213529334864));
#29984=CARTESIAN_POINT('',(-0.00401161256188314,0.00605965005927102,-0.00571596800107702));
#29985=CARTESIAN_POINT('',(-0.0020933533431652,0.00696004001606832,-0.00564333011111602));
#29986=CARTESIAN_POINT('',(-0.00103660122222697,0.00719352623141683,-0.00560742106129653));
#29987=CARTESIAN_POINT('',(0.00108534555283438,0.00718653088777161,-0.00553442542400878));
#29988=CARTESIAN_POINT('',(0.00214047746750604,0.00694566552741994,-0.00549851607983565));
#29989=CARTESIAN_POINT('',(0.0040526486037888,0.0060324173925454,-0.0054258789192123));
#29990=CARTESIAN_POINT('',(0.00490527977717149,0.00536278561505491,-0.00538971097675477));
#29991=CARTESIAN_POINT('',(0.00624194467998492,0.00372108952233504,-0.00531733635401815));
#29992=CARTESIAN_POINT('',(0.00672701543546565,0.00275016688147177,-0.00528099248907933));
#29993=CARTESIAN_POINT('',(0.0072334610169168,0.000695832792476032,-0.00520877770526449));
#29994=CARTESIAN_POINT('',(0.0072566571092038,-0.000389846331799926,-0.00517234498897591));
#29995=CARTESIAN_POINT('',(0.00683682612902857,-0.00246321173532627,-0.00510018368993359));
#29996=CARTESIAN_POINT('',(0.00639333402113973,-0.00345443801252004,-0.00506375119549885));
#29997=CARTESIAN_POINT('',(0.00512762614573075,-0.0051499494907857,-0.00499153587545613));
#29998=CARTESIAN_POINT('',(0.00430319660631324,-0.00585580981979079,-0.00495519258295575));
#29999=CARTESIAN_POINT('',(0.00243323520837126,-0.00684832348254423,-0.00488281711152852));
#30000=CARTESIAN_POINT('',(0.00138731905467838,-0.00713356432844633,-0.0048466498192527));
#30001=CARTESIAN_POINT('',(-0.00072948569468554,-0.00723133015881576,-0.00477401192930397));
#30002=CARTESIAN_POINT('',(-0.00179514865645575,-0.00704264176550899,-0.00473810287945765));
#30003=CARTESIAN_POINT('',(-0.00375289484889557,-0.00622414503550719,-0.00466510724221132));
#30004=CARTESIAN_POINT('',(-0.00463553444612406,-0.00559783295628993,-0.00462919789801713));
#30005=CARTESIAN_POINT('',(-0.00605266529073802,-0.00402234548266793,-0.00455656073739454));
#30006=CARTESIAN_POINT('',(-0.00658413679357753,-0.00307739856515646,-0.00452039279493507));
#30007=CARTESIAN_POINT('',(-0.00719080424345081,-0.00104914963355747,-0.00444801817220151));
#30008=CARTESIAN_POINT('',(-0.00726739517749341,3.34944636354764E-5,-0.00441167430725886));
#30009=CARTESIAN_POINT('',(-0.00694913026412382,0.00212526001481356,-0.00433945952344863));
#30010=CARTESIAN_POINT('',(-0.00655508924530171,0.00313717349682264,-0.00430302680714884));
#30011=CARTESIAN_POINT('',(-0.00537377340642612,0.00489205099604989,-0.00423086550812416));
#30012=CARTESIAN_POINT('',(-0.00458471425111404,0.00563810758356184,-0.00419443301368414));
#30013=CARTESIAN_POINT('',(-0.00276650849877146,0.00672019050133746,-0.00412221769363452));
#30014=CARTESIAN_POINT('',(-0.00173471386783098,0.00705682488623278,-0.00408587440113144));
#30015=CARTESIAN_POINT('',(0.000372723729446471,0.00725818469882635,-0.0040134989297165));
#30016=CARTESIAN_POINT('',(0.00144818120252681,0.00712145809453751,-0.00397733163742573));
#30017=CARTESIAN_POINT('',(0.00344126714831952,0.00640171583705481,-0.00390469374749465));
#30018=CARTESIAN_POINT('',(0.00435360342525374,0.00581957893249987,-0.00386878469764982));
#30019=CARTESIAN_POINT('',(0.00584909992429147,0.00431418952361097,-0.00379578906038278));
#30020=CARTESIAN_POINT('',(0.00642487332654076,0.00339778106204067,-0.00375987971620468));
#30021=CARTESIAN_POINT('',(0.00713121855472419,0.00139990793571129,-0.00368724255557058));
#30022=CARTESIAN_POINT('',(0.00726061866851071,0.000323505480401402,-0.00365107461311612));
#30023=CARTESIAN_POINT('',(0.00704492904565339,-0.00178251377636519,-0.0035786999903841));
#30024=CARTESIAN_POINT('',(0.00670137988284643,-0.00281205658028245,-0.00354235612544367));
#30025=CARTESIAN_POINT('',(0.00560685742264143,-0.00462280125038053,-0.00347014134162729));
#30026=CARTESIAN_POINT('',(0.00485556846582585,-0.00540689443550281,-0.00343370862533945));
#30027=CARTESIAN_POINT('',(0.0030926123960786,-0.00657611983917729,-0.00336154732629711));
#30028=CARTESIAN_POINT('',(0.00207811329689281,-0.00696342638458015,-0.00332511483186319));
#30029=CARTESIAN_POINT('',(-1.57849886678835E-5,-0.00726734342673904,-0.00325289951181893));
#30030=CARTESIAN_POINT('',(-0.00109786333180993,-0.00718350233401927,-0.00321655621931441));
#30031=CARTESIAN_POINT('',(-0.0031219388582049,-0.00656305309032384,-0.00314418074789715));
#30032=CARTESIAN_POINT('',(-0.00406320899944794,-0.00602517442190716,-0.00310801345561085));
#30033=CARTESIAN_POINT('',(-0.00562914687378846,-0.00459749831080149,-0.00303537556567285));
#30034=CARTESIAN_POINT('',(-0.00624926153807508,-0.0037105379616394,-0.0029994665158259));
#30035=CARTESIAN_POINT('',(-0.00705483255843151,-0.0017474377649635,-0.00292647087857037));
#30036=CARTESIAN_POINT('',(-0.00723608348461909,-0.000680447802060205,-0.00289056153438103));
#30037=CARTESIAN_POINT('',(-0.0071241084384037,0.0014356529042668,-0.00281792437375769));
#30038=CARTESIAN_POINT('',(-0.00683173716883591,0.00247963838116247,-0.00278175643129986));
#30039=CARTESIAN_POINT('',(-0.00582652726309597,0.00434280562236042,-0.00270938180856403));
#30040=CARTESIAN_POINT('',(-0.00511514024919768,0.00516250857393693,-0.00267303794362471));
#30041=CARTESIAN_POINT('',(-0.0034109913648488,0.00641656290137277,-0.00260082315980989));
#30042=CARTESIAN_POINT('',(-0.00241683140327436,0.00685346470999906,-0.00256439044351557));
#30043=CARTESIAN_POINT('',(-0.000340629183025886,0.00725903404945992,-0.00249222914448476));
#30044=CARTESIAN_POINT('',(0.000744861568633197,0.00722862664216346,-0.00245579665004158));
#30045=CARTESIAN_POINT('',(0.00279567535467062,0.00670810919404948,-0.00238358133000424));
#30046=CARTESIAN_POINT('',(0.00376330079133947,0.00621655667006173,-0.0023472380374981));
#30047=CARTESIAN_POINT('',(0.00539586709624765,0.00486875614304302,-0.00227486256607702));
#30048=CARTESIAN_POINT('',(0.00605965005927792,0.0040116125618877,-0.00223869527378932));
#30049=CARTESIAN_POINT('',(0.00696004001606203,0.00209335334315932,-0.00216605738385825));
#30050=CARTESIAN_POINT('',(0.00719352623141566,0.00103660122222664,-0.00213014833401346));
#30051=CARTESIAN_POINT('',(0.00718653088777276,-0.00108534555283466,-0.00205715269674642));
#30052=CARTESIAN_POINT('',(0.00694566552742021,-0.00214047746750529,-0.00202124335256258));
#30053=CARTESIAN_POINT('',(0.0060324173925453,-0.00405264860378919,-0.00194860619194));
#30054=CARTESIAN_POINT('',(0.00536278561505485,-0.00490527977717104,-0.00191243824948167));
#30055=CARTESIAN_POINT('',(0.0037210895223348,-0.00624194467998561,-0.00184006362674582));
#30056=CARTESIAN_POINT('',(0.00275016688147183,-0.0067270154354661,-0.00180371976180508));
#30057=CARTESIAN_POINT('',(0.000695832792475538,-0.00723346101691648,-0.00173150497799332));
#30058=CARTESIAN_POINT('',(-0.000389846331799945,-0.00725665710920745,-0.00169507226169586));
#30059=CARTESIAN_POINT('',(-0.00246321173532793,-0.00683682612902454,-0.00162291096266811));
#30060=CARTESIAN_POINT('',(-0.0034544380125203,-0.00639333402113907,-0.00158647846822539));
#30061=CARTESIAN_POINT('',(-0.0051499494907848,-0.00512762614573182,-0.00151426314818421));
#30062=CARTESIAN_POINT('',(-0.00585580981979337,-0.00430319660631435,-0.00147791985567843));
#30063=CARTESIAN_POINT('',(-0.00684832348254183,-0.0024332352083697,-0.00140554438426041));
#30064=CARTESIAN_POINT('',(-0.00713356432844919,-0.00138731905467894,-0.00136937709197385));
#30065=CARTESIAN_POINT('',(-0.00723133015881286,0.000729485694686566,-0.0012967392020374));
#30066=CARTESIAN_POINT('',(-0.00704264176550485,0.00179514865645567,-0.00126083015219145));
#30067=CARTESIAN_POINT('',(-0.0062241450355111,0.00375289484889606,-0.00118783451493208));
#30068=CARTESIAN_POINT('',(-0.00559783295628811,0.00463553444612332,-0.0011519251707444));
#30069=CARTESIAN_POINT('',(-0.00402234548266938,0.00605266529073901,-0.00107928801012182));
#30070=CARTESIAN_POINT('',(-0.00307739856515607,0.00658413679357564,-0.00104312006766541));
#30071=CARTESIAN_POINT('',(-0.00104914963355747,0.00719080424345277,-0.000970745444925725));
#30072=CARTESIAN_POINT('',(3.34944636362563E-5,0.00726739517749143,-0.000934401579989581));
#30073=CARTESIAN_POINT('',(0.00212526001481323,0.00694913026412567,-0.00086218679617245));
#30074=CARTESIAN_POINT('',(0.00313717349682277,0.00655508924530081,-0.000825754079879204));
#30075=CARTESIAN_POINT('',(0.00489205099605003,0.00537377340642675,-0.000753592780848384));
#30076=CARTESIAN_POINT('',(0.0056381075835625,0.00458471425111558,-0.000717160286406051));
#30077=CARTESIAN_POINT('',(0.00672019050133696,0.00276650849876955,-0.00064494496636717));
#30078=CARTESIAN_POINT('',(0.00705682488623223,0.00173471386782946,-0.000608601673859866));
#30079=CARTESIAN_POINT('',(0.00725818469882695,-0.000372723729446043,-0.000536226202442616));
#30080=CARTESIAN_POINT('',(0.00712145809453642,-0.00144818120252827,-0.000500058910156047));
#30081=CARTESIAN_POINT('',(0.00640171583705524,-0.00344126714831973,-0.000427421020218825));
#30082=CARTESIAN_POINT('',(0.00581957893250037,-0.00435360342525503,-0.000391511970372879));
#30083=CARTESIAN_POINT('',(0.00431418952361021,-0.00584909992429036,-0.000318516333114281));
#30084=CARTESIAN_POINT('',(0.00339778106204239,-0.00642487332654475,-0.000282606988926975));
#30085=CARTESIAN_POINT('',(0.00139990793570993,-0.00713121855472002,-0.00020996982830286));
#30086=CARTESIAN_POINT('',(0.000323505480399655,-0.00726061866851029,-0.000173801885847229));
#30087=CARTESIAN_POINT('',(-0.0017825137763636,-0.00704492904565378,-0.000101427263107548));
#30088=CARTESIAN_POINT('',(-0.00281205658028296,-0.00670137988284679,-6.50833981679304E-5));
#30089=CARTESIAN_POINT('',(-0.0046228012503775,-0.00560685742264234,7.13138564229714E-6));
#30090=CARTESIAN_POINT('',(-0.00540689443550383,-0.00485556846583195,4.3564101940445E-5));
#30091=CARTESIAN_POINT('',(-0.00657611983917429,-0.00309261239607615,0.000115725400968197));
#30092=CARTESIAN_POINT('',(-0.00696342638458038,-0.00207811329689332,0.000152157895411852));
#30093=CARTESIAN_POINT('',(-0.00726734342673808,1.57849886669528E-5,0.0002243732154515));
#30094=CARTESIAN_POINT('',(-0.00718350233401693,0.00109786333180495,0.000260716507958075));
#30095=CARTESIAN_POINT('',(-0.00656305309032657,0.00312193885819541,0.000333091979374559));
#30096=CARTESIAN_POINT('',(-0.00602517442193104,0.00406320899947221,0.000369259271663406));
#30097=CARTESIAN_POINT('',(-0.00459749831074794,0.00562914687383506,0.000441897161614154));
#30098=CARTESIAN_POINT('',(-0.00371053796151535,0.00624926153783101,0.000477806211348708));
#30099=CARTESIAN_POINT('',(-0.00174743776551818,0.00705483255842964,0.000550801848655444));
#30100=CARTESIAN_POINT('',(-0.000680447801294133,0.00723608348588212,0.000586711193786415));
#30101=CARTESIAN_POINT('',(0.00143565290608666,0.0071241084365796,0.000659348353022638));
#30102=CARTESIAN_POINT('',(0.00247963837529481,0.00683173716790875,0.000695516292370224));
#30103=CARTESIAN_POINT('',(0.0043428056206459,0.00582652727327286,0.00076789092290518));
#30104=CARTESIAN_POINT('',(0.00516250859039049,0.00511514023630632,0.000804234794196687));
#30105=CARTESIAN_POINT('',(0.00641656289023011,0.00341099133157275,0.0008764495419424));
#30106=CARTESIAN_POINT('',(0.00685346469520728,0.00241683146463233,0.000912882267660161));
#30107=CARTESIAN_POINT('',(0.00725903411303602,0.000340629271551516,0.00098504370920131));
#30108=CARTESIAN_POINT('',(0.00722862665697431,-0.000744861703369959,0.00102147602741882));
#30109=CARTESIAN_POINT('',(0.00670810890042664,-0.00279567567614128,0.00109369086559387));
#30110=CARTESIAN_POINT('',(0.00621655607651332,-0.00376330035189889,0.00113003525147544));
#30111=CARTESIAN_POINT('',(0.00486875838265234,-0.00539586578431444,0.00120241207477105));
#30112=CARTESIAN_POINT('',(0.00401161662392975,-0.00605965436823582,0.00123857449452884));
#30113=CARTESIAN_POINT('',(0.00209333657742418,-0.00696004077825442,0.0013112095800839));
#30114=CARTESIAN_POINT('',(0.00103659171941237,-0.00719350430124366,0.00134715113465353));
#30115=CARTESIAN_POINT('',(-0.00191041971977791,-0.00718386892224559,0.00144849411294274));
#30116=CARTESIAN_POINT('',(-0.00377227819610396,-0.00640401708981634,0.00151212929633834));
#30117=CARTESIAN_POINT('',(-0.0064299244082464,-0.00373033709005478,0.00164156781191397));
#30118=CARTESIAN_POINT('',(-0.00719625087246649,-0.00185395380901434,0.00170544297515432));
#30119=CARTESIAN_POINT('',(-0.00719005711644639,2.43665513196906E-5,0.00177004279007146));
#30120=CARTESIAN_POINT('',(-0.00719,-2.43712308654023E-5,-0.0140410700265819));
#30121=CARTESIAN_POINT('',(-0.00719309747276633,0.000914781327291283,-0.0140087701339982));
#30122=CARTESIAN_POINT('',(-0.00701046692282683,0.00185383013393277,-0.0139769826252248));
#30123=CARTESIAN_POINT('',(-0.00584628899116327,0.00469565481227827,-0.0138710392878109));
#30124=CARTESIAN_POINT('',(-0.00413420496023883,0.00625264525909713,-0.0137993589218868));
#30125=CARTESIAN_POINT('',(-0.00109778115756082,0.00718353970545525,-0.0136908149277581));
#30126=CARTESIAN_POINT('',(-1.57621275787881E-5,0.00726727668491749,-0.013654505956057));
#30127=CARTESIAN_POINT('',(0.0020780670851226,0.00696336385150681,-0.0135822796027047));
#30128=CARTESIAN_POINT('',(0.00309258005265746,0.00657607392611431,-0.0135458386651108));
#30129=CARTESIAN_POINT('',(0.00485553091203102,0.00540685351702608,-0.0134736824086932));
#30130=CARTESIAN_POINT('',(0.00560681015793595,0.00462276743850325,-0.0134372508723692));
#30131=CARTESIAN_POINT('',(0.00670132423911886,0.00281203924609828,-0.0133650342858113));
#30132=CARTESIAN_POINT('',(0.00704487175681332,0.0017825046314887,-0.0133286905839261));
#30133=CARTESIAN_POINT('',(0.00726056134134748,-0.000323498100568699,-0.0132563164906695));
#30134=CARTESIAN_POINT('',(0.00713116287663823,-0.00139989213428312,-0.013220148364931));
#30135=CARTESIAN_POINT('',(0.00642482455556629,-0.00339774967419534,-0.0131475110777197));
#30136=CARTESIAN_POINT('',(0.00584905635718351,-0.00431415134828831,-0.0131116018059614));
#30137=CARTESIAN_POINT('',(0.00435357284755307,-0.00581952969982387,-0.0130386062056008));
#30138=CARTESIAN_POINT('',(0.00344124413936916,-0.00640166266807087,-0.0130026971236706));
#30139=CARTESIAN_POINT('',(0.00144817457480563,-0.00712140051957246,-0.0129300592451617));
#30140=CARTESIAN_POINT('',(0.000372725724967005,-0.00725812679414896,-0.0128938919514255));
#30141=CARTESIAN_POINT('',(-0.00173469529522488,-0.00705677001193887,-0.012821516476213));
#30142=CARTESIAN_POINT('',(-0.00276648191979289,-0.00672013901723145,-0.0127851731895264));
#30143=CARTESIAN_POINT('',(-0.00458467403739847,-0.00563806590143227,-0.012712957858533));
#30144=CARTESIAN_POINT('',(-0.00537372737395455,-0.00489201581532433,-0.0126765253742606));
#30145=CARTESIAN_POINT('',(-0.00655503508825474,-0.00313715298829169,-0.0126043640616781));
#30146=CARTESIAN_POINT('',(-0.00694907362059592,-0.00212524786670271,-0.0125679313555053));
#30147=CARTESIAN_POINT('',(-0.00726733745110847,-3.34990726667784E-5,-0.012495716560779));
#30148=CARTESIAN_POINT('',(-0.0071907478402206,0.0010491364390741,-0.0124593727016529));
#30149=CARTESIAN_POINT('',(-0.00658408658164294,0.00307736969557237,-0.0123869980757161));
#30150=CARTESIAN_POINT('',(-0.00605261991751576,0.00402230947970013,-0.0123508301306084));
#30151=CARTESIAN_POINT('',(-0.00463550142938601,0.00559778534343702,-0.0122781929793886));
#30152=CARTESIAN_POINT('',(-0.00375286918367178,0.00622409311106949,-0.0122422836201452));
#30153=CARTESIAN_POINT('',(-0.00179513925007463,0.00704258456041726,-0.0121692880094645));
#30154=CARTESIAN_POINT('',(-0.000729484790171836,0.00723127223232546,-0.0121333789446197));
#30155=CARTESIAN_POINT('',(0.00138730314760839,0.00713350860255954,-0.0120607410639456));
#30156=CARTESIAN_POINT('',(0.00243321120648015,0.00684827074844557,-0.0120245737691142));
#30157=CARTESIAN_POINT('',(0.00430315844720215,0.00585576622976275,-0.0119521982943733));
#30158=CARTESIAN_POINT('',(0.00512758188781125,0.00514991209723695,-0.0119158550077828));
#30159=CARTESIAN_POINT('',(0.00639328091757387,0.00345441489233318,-0.0118436396767009));
#30160=CARTESIAN_POINT('',(0.00683677013747896,0.0024631968483955,-0.0118072071924502));
#30161=CARTESIAN_POINT('',(0.00725659922633007,0.000389848109405319,-0.011735045879847));
#30162=CARTESIAN_POINT('',(0.00723340403624636,-0.000695822339324392,-0.0116986131736994));
#30163=CARTESIAN_POINT('',(0.00672696386703592,-0.00275014053235113,-0.0116263983789488));
#30164=CARTESIAN_POINT('',(0.00624189761949387,-0.00372105574763302,-0.0115900545198076));
#30165=CARTESIAN_POINT('',(0.00490524443531421,-0.00536273972777125,-0.0115176798939249));
#30166=CARTESIAN_POINT('',(0.00405262046213646,-0.00603236676656215,-0.0114815119487978));
#30167=CARTESIAN_POINT('',(0.00214046518466179,-0.00694560890392152,-0.0114088747975626));
#30168=CARTESIAN_POINT('',(0.00108534171188601,-0.00718647309418859,-0.0113729654383349));
#30169=CARTESIAN_POINT('',(-0.00103658802115338,-0.00719346978113902,-0.0112999698276385));
#30170=CARTESIAN_POINT('',(-0.00209333201131658,-0.0069599861528186,-0.0112640607627929));
#30171=CARTESIAN_POINT('',(-0.00401157654030057,-0.00605960466264294,-0.0111914228821357));
#30172=CARTESIAN_POINT('',(-0.00486871378773508,-0.00539582756142553,-0.0111552555873162));
#30173=CARTESIAN_POINT('',(-0.00621650473444587,-0.0037632751222566,-0.011082880112535));
#30174=CARTESIAN_POINT('',(-0.00670805399516715,-0.00279565774430619,-0.0110465368259488));
#30175=CARTESIAN_POINT('',(-0.00722856873315945,-0.000744860530218091,-0.0109743214948983));
#30176=CARTESIAN_POINT('',(-0.00725897662301592,0.000340621509716384,-0.0109378890105921));
#30177=CARTESIAN_POINT('',(-0.00685341191347264,0.00241680761016474,-0.0108657276980687));
#30178=CARTESIAN_POINT('',(-0.00641651425833895,0.00341095990183559,-0.0108292949918682));
#30179=CARTESIAN_POINT('',(-0.00516247101429667,0.00511509617140522,-0.0107570801971437));
#30180=CARTESIAN_POINT('',(-0.00434277506916309,0.00582647805008706,-0.0107207363380231));
#30181=CARTESIAN_POINT('',(-0.00247962328983785,0.00683168124975376,-0.0106483617120729));
#30182=CARTESIAN_POINT('',(-0.00143564627849434,0.0071240508967529,-0.0106121937669828));
#30183=CARTESIAN_POINT('',(0.000680437481053837,0.00723602647088379,-0.0105395566157415));
#30184=CARTESIAN_POINT('',(0.00174741919689521,0.00705477769426572,-0.0105036472565332));
#30185=CARTESIAN_POINT('',(0.00371050416284737,0.00624921443664078,-0.0104306516458038));
#30186=CARTESIAN_POINT('',(0.00459745799018133,0.00562910527398703,-0.0103947425809817));
#30187=CARTESIAN_POINT('',(0.0060251237697562,0.00406318084328688,-0.0103221047003107));
#30188=CARTESIAN_POINT('',(0.00656299882979235,0.00312191854146624,-0.0102859374054834));
#30189=CARTESIAN_POINT('',(0.00718344452864146,0.00109785949157134,-0.0102135619307314));
#30190=CARTESIAN_POINT('',(0.00726728569041279,1.57898425179862E-5,-0.0101772186441096));
#30191=CARTESIAN_POINT('',(0.00696337248626668,-0.0020780920954515,-0.0101050033131013));
#30192=CARTESIAN_POINT('',(0.00657606972051115,-0.00309258333071337,-0.0100685708287816));
#30193=CARTESIAN_POINT('',(0.00540685476309802,-0.00485552627950851,-0.00999640951624288));
#30194=CARTESIAN_POINT('',(0.00462276835045015,-0.00560680973971266,-0.00995997681002896));
#30195=CARTESIAN_POINT('',(0.00281203874754511,-0.00670132478683354,-0.0098877620153467));
#30196=CARTESIAN_POINT('',(0.00178250438189289,-0.00704487188654584,-0.00985141815618041));
#30197=CARTESIAN_POINT('',(-0.000323498023658633,-0.0072605612308287,-0.0097790435302793));
#30198=CARTESIAN_POINT('',(-0.00139989203688523,-0.00713116285759408,-0.00974287558516111));
#30199=CARTESIAN_POINT('',(-0.00339774970846165,-0.00642482460240109,-0.00967023843392671));
#30200=CARTESIAN_POINT('',(-0.00431415137335821,-0.00584905634211228,-0.00963432907474912));
#30201=CARTESIAN_POINT('',(-0.00581952968153659,-0.00435357284343158,-0.0095613334639515));
#30202=CARTESIAN_POINT('',(-0.00640166266610289,-0.00344124414514989,-0.00952542439916768));
#30203=CARTESIAN_POINT('',(-0.00712140052315398,-0.00144817457337093,-0.00945278651848825));
#30204=CARTESIAN_POINT('',(-0.00725812679376296,-0.000372725723830902,-0.00941661922368434));
#30205=CARTESIAN_POINT('',(-0.00705677001142131,0.00173469529458462,-0.00934424374889396));
#30206=CARTESIAN_POINT('',(-0.00672013901740774,0.0027664819196555,-0.00930790046227081));
#30207=CARTESIAN_POINT('',(-0.00563806590146389,0.00458467403754789,-0.00923568513130384));
#30208=CARTESIAN_POINT('',(-0.00489201581527204,0.00537372737394528,-0.00919925264695077));
#30209=CARTESIAN_POINT('',(-0.00313715298830901,0.00655503508825429,-0.00912709133443729));
#30210=CARTESIAN_POINT('',(-0.0021252478667098,0.00694907362059298,-0.00909065862822848));
#30211=CARTESIAN_POINT('',(-3.34990726673003E-5,0.00726733745111181,-0.00901844383351088));
#30212=CARTESIAN_POINT('',(0.0010491364390763,0.00719074784022145,-0.00898209997438099));
#30213=CARTESIAN_POINT('',(0.00307736969557334,0.00658408658164155,-0.00890972534844229));
#30214=CARTESIAN_POINT('',(0.00402230947970229,0.00605261991751987,-0.00887355740334446));
#30215=CARTESIAN_POINT('',(0.00559778534343459,0.00463550142938187,-0.008800920252107));
#30216=CARTESIAN_POINT('',(0.00622409311107522,0.00375286918367609,-0.00876501089289031));
#30217=CARTESIAN_POINT('',(0.0070425845604117,0.00179513925006985,-0.00869201528217398));
#30218=CARTESIAN_POINT('',(0.00723127223231931,0.000729484790173338,-0.00865610621733461));
#30219=CARTESIAN_POINT('',(0.00713350860256567,-0.00138730314760929,-0.0085834683366851));
#30220=CARTESIAN_POINT('',(0.0068482707484462,-0.00243321120648243,-0.00854730104184166));
#30221=CARTESIAN_POINT('',(0.00585576622976196,-0.00430315844720011,-0.00847492556710038));
#30222=CARTESIAN_POINT('',(0.00514991209723149,-0.00512758188779838,-0.00843858228048562));
#30223=CARTESIAN_POINT('',(0.00345441489234066,-0.00639328091758518,-0.0083663669494527));
#30224=CARTESIAN_POINT('',(0.00246319684839438,-0.00683677013746513,-0.00832993446515067));
#30225=CARTESIAN_POINT('',(0.000389848109409576,-0.00725659922634325,-0.00825777315260114));
#30226=CARTESIAN_POINT('',(-0.000695822339321421,-0.00723340403624211,-0.00822134044641911));
#30227=CARTESIAN_POINT('',(-0.00275014053234976,-0.00672696386704125,-0.00814912565168388));
#30228=CARTESIAN_POINT('',(-0.00372105574763575,-0.00624189761949856,-0.00811278179254448));
#30229=CARTESIAN_POINT('',(-0.00536273972776876,-0.00490524443530932,-0.00804040716664259));
#30230=CARTESIAN_POINT('',(-0.00603236676656028,-0.00405262046213817,-0.00800423922152594));
#30231=CARTESIAN_POINT('',(-0.00694560890392066,-0.00214046518466569,-0.00793160207028925));
#30232=CARTESIAN_POINT('',(-0.00718647309418995,-0.00108534171188497,-0.00789569271106792));
#30233=CARTESIAN_POINT('',(-0.00719346978113769,0.00103658802115313,-0.00782269710036002));
#30234=CARTESIAN_POINT('',(-0.00695998615282404,0.00209333201131557,-0.00778678803553218));
#30235=CARTESIAN_POINT('',(-0.00605960466264018,0.00401157654029584,-0.00771415015485122));
#30236=CARTESIAN_POINT('',(-0.00539582756142664,0.00486871378774006,-0.00767798286005378));
#30237=CARTESIAN_POINT('',(-0.00376327512225495,0.00621650473444129,-0.0076056073852519));
#30238=CARTESIAN_POINT('',(-0.00279565774430927,0.00670805399516752,-0.00756926409868168));
#30239=CARTESIAN_POINT('',(-0.000744860530220048,0.00722856873315786,-0.00749704876762038));
#30240=CARTESIAN_POINT('',(0.000340621509718325,0.00725897662302272,-0.00746061628333479));
#30241=CARTESIAN_POINT('',(0.00241680761016268,0.00685341191346589,-0.00738845497078066));
#30242=CARTESIAN_POINT('',(0.00341095990183554,0.0064165142583411,-0.00735202226459938));
#30243=CARTESIAN_POINT('',(0.00511509617140321,0.00516247101429606,-0.0072798074698672));
#30244=CARTESIAN_POINT('',(0.00582647805007756,0.0043427750691594,-0.00724346361073014));
#30245=CARTESIAN_POINT('',(0.00683168124976245,0.00247962328984308,-0.00717108898482058));
#30246=CARTESIAN_POINT('',(0.00712405089675078,0.00143564627849451,-0.00713492103970666));
#30247=CARTESIAN_POINT('',(0.0072360264708859,-0.000680437481053441,-0.00706228388847226));
#30248=CARTESIAN_POINT('',(0.00705477769426897,-0.00174741919689787,-0.00702637452926781));
#30249=CARTESIAN_POINT('',(0.00624921443663749,-0.00371050416284487,-0.00695337891852387));
#30250=CARTESIAN_POINT('',(0.00562910527398633,-0.00459745799018292,-0.00691746985371441));
#30251=CARTESIAN_POINT('',(0.00406318084328793,-0.00602512376975431,-0.00684483197303269));
#30252=CARTESIAN_POINT('',(0.00312191854146655,-0.00656299882979698,-0.00680866467822031));
#30253=CARTESIAN_POINT('',(0.00109785949157234,-0.00718344452863644,-0.00673628920344911));
#30254=CARTESIAN_POINT('',(1.57898425157631E-5,-0.0072672856904205,-0.00669994591685016));
#30255=CARTESIAN_POINT('',(-0.00207809209544696,-0.00696337248625942,-0.0066277305858157));
#30256=CARTESIAN_POINT('',(-0.00309258333072013,-0.00657606972051688,-0.00659129810152624));
#30257=CARTESIAN_POINT('',(-0.00485552627950234,-0.00540685476309198,-0.00651913678895295));
#30258=CARTESIAN_POINT('',(-0.00560680973972307,-0.00462276835045597,-0.00648270408278328));
#30259=CARTESIAN_POINT('',(-0.00670132478682111,-0.00281203874754279,-0.00641048928804727));
#30260=CARTESIAN_POINT('',(-0.00704487188655621,-0.0017825043818928,-0.00637414542892963));
#30261=CARTESIAN_POINT('',(-0.00726056123081833,0.00032349802365789,-0.00630177080298481));
#30262=CARTESIAN_POINT('',(-0.00713116285758991,0.0013998920368823,-0.00626560285788283));
#30263=CARTESIAN_POINT('',(-0.00642482460240738,0.00339774970845881,-0.00619296570665995));
#30264=CARTESIAN_POINT('',(-0.00584905634210328,0.00431415137334864,-0.00615705634745419));
#30265=CARTESIAN_POINT('',(-0.00435357284344004,0.00581952968154678,-0.00608406073670106));
#30266=CARTESIAN_POINT('',(-0.00344124414515375,0.00640166266610718,-0.00604815167190321));
#30267=CARTESIAN_POINT('',(-0.00144817457337304,0.00712140052314761,-0.00597551379120768));
#30268=CARTESIAN_POINT('',(-0.000372725723831925,0.00725812679375837,-0.00593934649640361));
#30269=CARTESIAN_POINT('',(0.00173469529458617,0.0070567700114259,-0.00586697102162934));
#30270=CARTESIAN_POINT('',(0.00276648191966689,0.0067201390174245,-0.00583062773503884));
#30271=CARTESIAN_POINT('',(0.00458467403753271,0.0056380659014494,-0.00575841240399055));
#30272=CARTESIAN_POINT('',(0.00537372737395314,0.00489201581527671,-0.00572197991969736));
#30273=CARTESIAN_POINT('',(0.00655503508824469,0.00313715298830708,-0.00564981860714551));
#30274=CARTESIAN_POINT('',(0.00694907362059124,0.00212524786670918,-0.00561338590095199));
#30275=CARTESIAN_POINT('',(0.00726733745111319,3.34990726703471E-5,-0.00554117110624206));
#30276=CARTESIAN_POINT('',(0.00719074784021865,-0.00104913643907644,-0.00550482724710189));
#30277=CARTESIAN_POINT('',(0.00658408658164423,-0.00307736969557393,-0.00543245262117609));
#30278=CARTESIAN_POINT('',(0.00605261991751471,-0.00402230947969808,-0.00539628467605725));
#30279=CARTESIAN_POINT('',(0.00463550142938722,-0.00559778534343868,-0.00532364752484892));
#30280=CARTESIAN_POINT('',(0.00375286918367852,-0.00622409311108351,-0.00528773816563143));
#30281=CARTESIAN_POINT('',(0.00179513925006713,-0.00704258456040356,-0.00521474255488749));
#30282=CARTESIAN_POINT('',(0.000729484790170839,-0.0072312722323272,-0.00517883349007728));
#30283=CARTESIAN_POINT('',(-0.00138730314760581,-0.00713350860255783,-0.00510619560939708));
#30284=CARTESIAN_POINT('',(-0.00243321120648513,-0.00684827074845075,-0.00507002831457975));
#30285=CARTESIAN_POINT('',(-0.00430315844719737,-0.00585576622975746,-0.00499765283981685));
#30286=CARTESIAN_POINT('',(-0.00512758188780396,-0.00514991209723392,-0.00496130955322521));
#30287=CARTESIAN_POINT('',(-0.00639328091758023,-0.0034544148923375,-0.00488909422216774));
#30288=CARTESIAN_POINT('',(-0.00683677013746633,-0.00246319684839675,-0.00485266173788293));
#30289=CARTESIAN_POINT('',(-0.00725659922634214,-0.000389848109406802,-0.00478050042532344));
#30290=CARTESIAN_POINT('',(-0.00723340403623665,0.000695822339320062,-0.00474406771913376));
#30291=CARTESIAN_POINT('',(-0.00672696386704651,0.00275014053235206,-0.00467185292442382));
#30292=CARTESIAN_POINT('',(-0.00624189761950296,0.00372105574764178,-0.0046355090652864));
#30293=CARTESIAN_POINT('',(-0.00490524443530459,0.00536273972776314,-0.00456313443935523));
#30294=CARTESIAN_POINT('',(-0.00405262046213943,0.00603236676656415,-0.00452696649425976));
#30295=CARTESIAN_POINT('',(-0.00214046518466428,0.00694560890391687,-0.00445432934301002));
#30296=CARTESIAN_POINT('',(-0.00108534171188336,0.00718647309421125,-0.0044184199838209));
#30297=CARTESIAN_POINT('',(0.001036588021152,0.00719346978111642,-0.00434542437306162));
#30298=CARTESIAN_POINT('',(0.00209333201131713,0.0069599861528244,-0.00430951530825866));
#30299=CARTESIAN_POINT('',(0.00401157654029508,0.0060596046626394,-0.00423687742757923));
#30300=CARTESIAN_POINT('',(0.00486871378773325,0.00539582756142202,-0.00420071013276347));
#30301=CARTESIAN_POINT('',(0.00621650473444845,0.00376327512225915,-0.00412833465799674));
#30302=CARTESIAN_POINT('',(0.00670805399516244,0.00279565774430914,-0.00409199137139973));
#30303=CARTESIAN_POINT('',(0.00722856873316311,0.000744860530219342,-0.00401977604035683));
#30304=CARTESIAN_POINT('',(0.00725897662302856,-0.000340621509718141,-0.00398334355607171));
#30305=CARTESIAN_POINT('',(0.00685341191346022,-0.00241680761016203,-0.00391118224349841));
#30306=CARTESIAN_POINT('',(0.00641651425833855,-0.00341095990183179,-0.00387474953731824));
#30307=CARTESIAN_POINT('',(0.00516247101429811,-0.0051150961714077,-0.00380253474260294));
#30308=CARTESIAN_POINT('',(0.00434277506916177,-0.00582647805008344,-0.00376619088347242));
#30309=CARTESIAN_POINT('',(0.00247962328983992,-0.00683168124975697,-0.00369381625753282));
#30310=CARTESIAN_POINT('',(0.00143564627849509,-0.00712405089675115,-0.00365764831243543));
#30311=CARTESIAN_POINT('',(-0.000680437481054029,-0.00723602647088551,-0.00358501116119796));
#30312=CARTESIAN_POINT('',(-0.00174741919689655,-0.00705477769426506,-0.00354910180198778));
#30313=CARTESIAN_POINT('',(-0.00371050416284675,-0.0062492144366412,-0.00347610619125841));
#30314=CARTESIAN_POINT('',(-0.00459745799018052,-0.00562910527398658,-0.00344019712643935));
#30315=CARTESIAN_POINT('',(-0.00602512376975749,-0.00406318084328682,-0.00336755924576223));
#30316=CARTESIAN_POINT('',(-0.0065629988297959,-0.00312191854146521,-0.00333139195094262));
#30317=CARTESIAN_POINT('',(-0.00718344452863822,-0.00109785949157136,-0.00325901647618125));
#30318=CARTESIAN_POINT('',(-0.00726728569042009,-1.57898425149358E-5,-0.00322267318957925));
#30319=CARTESIAN_POINT('',(-0.00696337248625936,0.00207809209544908,-0.00315045785854095));
#30320=CARTESIAN_POINT('',(-0.00657606972051391,0.00309258333071823,-0.00311402537424463));
#30321=CARTESIAN_POINT('',(-0.0054068547630946,0.00485552627950473,-0.00304186406168898));
#30322=CARTESIAN_POINT('',(-0.00462276835045416,0.00560680973972331,-0.00300543135550392));
#30323=CARTESIAN_POINT('',(-0.00281203874754034,0.00670132478682342,-0.00293321656078095));
#30324=CARTESIAN_POINT('',(-0.00178250438189282,0.00704487188655298,-0.00289687270164736));
#30325=CARTESIAN_POINT('',(0.000323498023658744,0.00726056123082163,-0.00282449807572156));
#30326=CARTESIAN_POINT('',(0.00139989203688323,0.00713116285759021,-0.00278833013060885));
#30327=CARTESIAN_POINT('',(0.00339774970846299,0.00642482460240528,-0.00271569297938826));
#30328=CARTESIAN_POINT('',(0.00431415137334793,0.00584905634210323,-0.00267978362017918));
#30329=CARTESIAN_POINT('',(0.00581952968154769,0.00435357284343988,-0.00260678800943063));
#30330=CARTESIAN_POINT('',(0.00640166266610557,0.00344124414514944,-0.00257087894462805));
#30331=CARTESIAN_POINT('',(0.00712140052315214,0.00144817457336933,-0.00249824106393712));
#30332=CARTESIAN_POINT('',(0.0072581267937555,0.000372725723834419,-0.00246207376912482));
#30333=CARTESIAN_POINT('',(0.00705677001142875,-0.00173469529458923,-0.00238969829436268));
#30334=CARTESIAN_POINT('',(0.00672013901742156,-0.00276648191966884,-0.00235335500776368));
#30335=CARTESIAN_POINT('',(0.00563806590144799,-0.00458467403753809,-0.00228113967672));
#30336=CARTESIAN_POINT('',(0.00489201581527501,-0.00537372737396127,-0.00224470719243486));
#30337=CARTESIAN_POINT('',(0.00313715298830232,-0.00655503508824093,-0.00217254587986231));
#30338=CARTESIAN_POINT('',(0.00212524786670617,-0.00694907362059226,-0.00213611317368258));
#30339=CARTESIAN_POINT('',(3.34990726649879E-5,-0.00726733745111344,-0.00206389837896573));
#30340=CARTESIAN_POINT('',(-0.0010491364390756,-0.00719074784021935,-0.00202755451983032));
#30341=CARTESIAN_POINT('',(-0.00307736969557517,-0.00658408658164341,-0.00195517989390222));
#30342=CARTESIAN_POINT('',(-0.00402230947970432,-0.00605261991751492,-0.00191901194879282));
#30343=CARTESIAN_POINT('',(-0.00559778534343856,-0.00463550142938151,-0.00184637479756761));
#30344=CARTESIAN_POINT('',(-0.00622409311108227,-0.00375286918367897,-0.00181046543835526));
#30345=CARTESIAN_POINT('',(-0.00704258456040493,-0.00179513925006642,-0.00173746982761822));
#30346=CARTESIAN_POINT('',(-0.00723127223232795,-0.000729484790167686,-0.00170156076280402));
#30347=CARTESIAN_POINT('',(-0.00713350860255669,0.001387303147611,-0.00162892288212461));
#30348=CARTESIAN_POINT('',(-0.00684827074845186,0.00243321120648628,-0.00159275558730857));
#30349=CARTESIAN_POINT('',(-0.00585576622975641,0.00430315844719611,-0.00152038011254261));
#30350=CARTESIAN_POINT('',(-0.00514991209723177,0.00512758188780289,-0.00148403682594472));
#30351=CARTESIAN_POINT('',(-0.00345441489233604,0.00639328091758393,-0.0014118214949026));
#30352=CARTESIAN_POINT('',(-0.00246319684839593,0.00683677013746831,-0.00137538901060983));
#30353=CARTESIAN_POINT('',(-0.000389848109407185,0.00725659922634024,-0.00130322769805111));
#30354=CARTESIAN_POINT('',(0.000695822339321743,0.0072334040362362,-0.00126679499186096));
#30355=CARTESIAN_POINT('',(0.00275014053235359,0.00672696386704615,-0.00119458019715104));
#30356=CARTESIAN_POINT('',(0.00372105574764232,0.00624189761950416,-0.00115823633801324));
#30357=CARTESIAN_POINT('',(0.00536273972776455,0.00490524443530179,-0.00108586171208286));
#30358=CARTESIAN_POINT('',(0.00603236676655764,0.00405262046213594,-0.00104969376697167));
#30359=CARTESIAN_POINT('',(0.00694560890392401,0.00214046518466646,-0.000977056615752623));
#30360=CARTESIAN_POINT('',(0.00718647309420243,0.00108534171188339,-0.000941147256542428));
#30361=CARTESIAN_POINT('',(0.00719346978112524,-0.00103658802115264,-0.000868151645794657));
#30362=CARTESIAN_POINT('',(0.00695998615282431,-0.00209333201131553,-0.000832242580984424));
#30363=CARTESIAN_POINT('',(0.0060596046626397,-0.00401157654029634,-0.000759604700308071));
#30364=CARTESIAN_POINT('',(0.00539582756142148,-0.00486871378773222,-0.00072343740548999));
#30365=CARTESIAN_POINT('',(0.00376327512225938,-0.00621650473444972,-0.000651061930724788));
#30366=CARTESIAN_POINT('',(0.00279565774430887,-0.00670805399516193,-0.000614718644124706));
#30367=CARTESIAN_POINT('',(0.000744860530219189,-0.00722856873316375,-0.000542503313086405));
#30368=CARTESIAN_POINT('',(-0.000340621509718041,-0.00725897662302607,-0.000506070828791677));
#30369=CARTESIAN_POINT('',(-0.00241680761016381,-0.00685341191346234,-0.000433909516232949));
#30370=CARTESIAN_POINT('',(-0.00341095990183245,-0.00641651425833751,-0.000397476810045951));
#30371=CARTESIAN_POINT('',(-0.00511509617140642,-0.00516247101429958,-0.000325262015329883));
#30372=CARTESIAN_POINT('',(-0.00582647805008241,-0.00434277506916021,-0.000288918156194358));
#30373=CARTESIAN_POINT('',(-0.00683168124975823,-0.00247962328984105,-0.000216543530265495));
#30374=CARTESIAN_POINT('',(-0.00712405089674981,-0.00143564627849449,-0.000180375585155457));
#30375=CARTESIAN_POINT('',(-0.00723602647088685,0.000680437481053904,-0.000107738433932561));
#30376=CARTESIAN_POINT('',(-0.00705477769426858,0.00174741919689845,-7.18290747204408E-5));
#30377=CARTESIAN_POINT('',(-0.00624921443663745,0.00371050416284529,1.1665360196661E-6));
#30378=CARTESIAN_POINT('',(-0.00562910527398621,0.00459745799018268,3.70756008341184E-5));
#30379=CARTESIAN_POINT('',(-0.00406318084328683,0.00602512376975562,0.000109713481509706));
#30380=CARTESIAN_POINT('',(-0.00312191854146526,0.0065629988297973,0.000145880776325484));
#30381=CARTESIAN_POINT('',(-0.00109785949157093,0.00718344452863693,0.000218256251096054));
#30382=CARTESIAN_POINT('',(-1.57898425130279E-5,0.0072672856904212,0.00025459953768962));
#30383=CARTESIAN_POINT('',(0.00207809209544763,0.00696337248625816,0.000326814868735592));
#30384=CARTESIAN_POINT('',(0.00309258333071925,0.0065760697205136,0.000363247353026133));
#30385=CARTESIAN_POINT('',(0.00485552627950401,0.00540685476309468,0.000435408665585627));
#30386=CARTESIAN_POINT('',(0.00560680973971897,0.00462276835045254,0.000471841371774156));
#30387=CARTESIAN_POINT('',(0.00670132478682792,0.00281203874754161,0.000544056166486389));
#30388=CARTESIAN_POINT('',(0.00704487188655321,0.00178250438189151,0.000580400025623436));
#30389=CARTESIAN_POINT('',(0.00726056123082148,-0.000323498023658519,0.000652774651553067));
#30390=CARTESIAN_POINT('',(0.00713116285759123,-0.00139989203688551,0.000688942596660811));
#30391=CARTESIAN_POINT('',(0.00642482460240361,-0.00339774970846239,0.000761579747887542));
#30392=CARTESIAN_POINT('',(0.00584905634210076,-0.00431415137334655,0.000797489107096591));
#30393=CARTESIAN_POINT('',(0.00435357284344211,-0.00581952968154928,0.000870484717838998));
#30394=CARTESIAN_POINT('',(0.00344124414514933,-0.00640166266610323,0.000906393782650393));
#30395=CARTESIAN_POINT('',(0.00144817457336979,-0.0071214005231543,0.000979031663329816));
#30396=CARTESIAN_POINT('',(0.000372725723832011,-0.00725812679375817,0.00101519895814289));
#30397=CARTESIAN_POINT('',(-0.00173469529458699,-0.00705677001142606,0.001087574432915));
#30398=CARTESIAN_POINT('',(-0.00276648191966839,-0.00672013901742019,0.00112391771951012));
#30399=CARTESIAN_POINT('',(-0.00458467403753602,-0.00563806590145063,0.00119613305055149));
#30400=CARTESIAN_POINT('',(-0.00537372737395561,-0.00489201581527777,0.0012325655348454));
#30401=CARTESIAN_POINT('',(-0.00655503508824468,-0.00313715298830325,0.00130472684740259));
#30402=CARTESIAN_POINT('',(-0.00694907362059189,-0.00212524786670655,0.00134115955359244));
#30403=CARTESIAN_POINT('',(-0.00726733745111301,-3.34990726660305E-5,0.00141337434830467));
#30404=CARTESIAN_POINT('',(-0.00719074784021694,0.00104913643907056,0.00144971820744406));
#30405=CARTESIAN_POINT('',(-0.00658408658164684,0.00307736969556589,0.00152209283336755));
#30406=CARTESIAN_POINT('',(-0.00605261991753943,0.00402230947972834,0.00155826077848144));
#30407=CARTESIAN_POINT('',(-0.00463550142931737,0.00559778534347777,0.00163089792971939));
#30408=CARTESIAN_POINT('',(-0.00375286918359511,0.006224093110923,0.00166680728882057));
#30409=CARTESIAN_POINT('',(-0.00179513925064184,0.00704258456042806,0.00173980289960575));
#30410=CARTESIAN_POINT('',(-0.0007294847893921,0.00723127223276442,0.00177571196536462));
#30411=CARTESIAN_POINT('',(0.00138730314952183,0.00713350860123271,0.00184834984465922));
#30412=CARTESIAN_POINT('',(0.00243321120190955,0.00684827075054466,0.00188451713634817));
#30413=CARTESIAN_POINT('',(0.00430315844327975,0.00585576623654509,0.00195689261891401));
#30414=CARTESIAN_POINT('',(0.00512758189718962,0.00514991207766484,0.00199323591196856));
#30415=CARTESIAN_POINT('',(0.00639328092669331,0.00345441487247999,0.00206545120685874));
#30416=CARTESIAN_POINT('',(0.00683677013791915,0.00246319691575483,0.00210188370012292));
#30417=CARTESIAN_POINT('',(0.00725659916989426,0.000389848177144325,0.0021740451558294));
#30418=CARTESIAN_POINT('',(0.00723340408349491,-0.00069582248149021,0.00221047768728494));
#30419=CARTESIAN_POINT('',(0.00672696408575062,-0.00275014098145917,0.00228269199671924));
#30420=CARTESIAN_POINT('',(0.00624189664462071,-0.00372105507060881,0.00231903694593017));
#30421=CARTESIAN_POINT('',(0.00490524509323122,-0.00536273718611709,0.00239141293832608));
#30422=CARTESIAN_POINT('',(0.00405262592252595,-0.00603237309137095,0.00242757601191714));
#30423=CARTESIAN_POINT('',(0.00214045155004707,-0.00694561550063064,0.00250021030746631));
#30424=CARTESIAN_POINT('',(0.00108533037484742,-0.00718642631050035,0.00253615220355904));
#30425=CARTESIAN_POINT('',(-0.00186165676778948,-0.00719625441939621,0.00263749534989383));
#30426=CARTESIAN_POINT('',(-0.00372887586619293,-0.00642951945250147,0.00270113018670128));
#30427=CARTESIAN_POINT('',(-0.00640422907181245,-0.00377360050585877,0.00283056960872658));
#30428=CARTESIAN_POINT('',(-0.00718374672632692,-0.00190268100220303,0.00289444373919848));
#30429=CARTESIAN_POINT('',(-0.00718994287258576,-2.43759101863917E-5,0.00295904411866391));
#30430=CARTESIAN_POINT('',(-0.006,-2.43712308653931E-5,-0.0140410700265819));
#30431=CARTESIAN_POINT('',(-0.00600309747414711,0.000755994738560391,-0.0140090793492257));
#30432=CARTESIAN_POINT('',(-0.00585022549906422,0.00154554847924553,-0.0139767317091225));
#30433=CARTESIAN_POINT('',(-0.00488277416170381,0.00391156551240249,-0.0138719117580559));
#30434=CARTESIAN_POINT('',(-0.00345414811439852,0.00521522772168569,-0.0137995939835592));
#30435=CARTESIAN_POINT('',(-0.000920416913494161,0.00599387797088215,-0.0136909247186258));
#30436=CARTESIAN_POINT('',(-1.83364399790589E-5,0.00606458475875607,-0.0136547070017816));
#30437=CARTESIAN_POINT('',(0.00173071508355203,0.00581192078991974,-0.013582263622242));
#30438=CARTESIAN_POINT('',(0.00257620709021928,0.0054899026401681,-0.013546041378497));
#30439=CARTESIAN_POINT('',(0.0040496481570146,0.00451412616898593,-0.0134735982934369));
#30440=CARTESIAN_POINT('',(0.00467595743139725,0.00386119227478036,-0.0134373767382566));
#30441=CARTESIAN_POINT('',(0.00559115533267521,0.00234942868328478,-0.0133649337688717));
#30442=CARTESIAN_POINT('',(0.00587789190074464,0.00149118187026969,-0.013328711875432));
#30443=CARTESIAN_POINT('',(0.00605911477020831,-0.000266602851011457,-0.0132562691328768));
#30444=CARTESIAN_POINT('',(0.00595132195371268,-0.00116523586494131,-0.0132200472158988));
#30445=CARTESIAN_POINT('',(0.00536345211542811,-0.00283155473315956,-0.0131476043990316));
#30446=CARTESIAN_POINT('',(0.00488207572844726,-0.00359821831670739,-0.013111382654392));
#30447=CARTESIAN_POINT('',(0.00363763601600018,-0.00485255191712249,-0.0130389394867723));
#30448=CARTESIAN_POINT('',(0.00287504504636738,-0.00534029243914702,-0.0130027180351518));
#30449=CARTESIAN_POINT('',(0.00121351369399411,-0.00594156052931282,-0.0129302744931486));
#30450=CARTESIAN_POINT('',(0.000315825750312525,-0.00605668045304735,-0.0128940532261725));
#30451=CARTESIAN_POINT('',(-0.00144337707403964,-0.00588978902230696,-0.0128216096183549));
#30452=CARTESIAN_POINT('',(-0.00230387638883705,-0.00560996798125232,-0.012785388316591));
#30453=CARTESIAN_POINT('',(-0.00382310259116674,-0.00470721006652816,-0.0127129448611614));
#30454=CARTESIAN_POINT('',(-0.00448099997246373,-0.00408613400852397,-0.0126767233862572));
#30455=CARTESIAN_POINT('',(-0.0054688674143523,-0.00262077375144199,-0.0126042801976742));
#30456=CARTESIAN_POINT('',(-0.00579763556460296,-0.0017778661740937,-0.0125680585008892));
#30457=CARTESIAN_POINT('',(-0.00606464167597128,-3.0946622266283E-5,-0.0124956155817382));
#30458=CARTESIAN_POINT('',(-0.00600111463142179,0.00087169976698755,-0.012459393707512));
#30459=CARTESIAN_POINT('',(-0.00549586755061847,0.00256503164149849,-0.0123869509484387));
#30460=CARTESIAN_POINT('',(-0.0050523880893689,0.00335400980216192,-0.0123507290311181));
#30461=CARTESIAN_POINT('',(-0.00387159456299549,0.00466851979026504,-0.0122782862186558));
#30462=CARTESIAN_POINT('',(-0.00313347130157478,0.00519260976096335,-0.0122420644730658));
#30463=CARTESIAN_POINT('',(-0.00150374624037729,0.00587523641666246,-0.0121696213045038));
#30464=CARTESIAN_POINT('',(-0.000612553833171288,0.00603401898911306,-0.0121333998532844));
#30465=CARTESIAN_POINT('',(0.00115259631366971,0.00595367775238322,-0.012060956311437));
#30466=CARTESIAN_POINT('',(0.00202600631780663,0.00571650438740237,-0.0120247350443508));
#30467=CARTESIAN_POINT('',(0.00358743121515774,0.00488909903514313,-0.0119522914365147));
#30468=CARTESIAN_POINT('',(0.00427534604366821,0.00430127927179916,-0.0119160701347756));
#30469=CARTESIAN_POINT('',(0.00533345753982393,0.00288585701390729,-0.011843626679348));
#30470=CARTESIAN_POINT('',(0.00570359994722143,0.00206029112764935,-0.0118074052044376));
#30471=CARTESIAN_POINT('',(0.00605550136478055,0.000328434275013915,-0.0117349620158554));
#30472=CARTESIAN_POINT('',(0.00603667676489193,-0.000576124907669123,-0.0116987403190736));
#30473=CARTESIAN_POINT('',(0.00561484107606885,-0.00229224694171357,-0.0116262973999176));
#30474=CARTESIAN_POINT('',(0.00521072192138963,-0.00310187271837801,-0.0115900755256951));
#30475=CARTESIAN_POINT('',(0.0040959244307272,-0.0044729576919261,-0.0115176327666191));
#30476=CARTESIAN_POINT('',(0.0033842739627938,-0.00503216622374487,-0.0114814108492998));
#30477=CARTESIAN_POINT('',(0.00179032179752591,-0.00579474497744012,-0.0114089680368375));
#30478=CARTESIAN_POINT('',(0.000907824274980536,-0.0059964734313809,-0.0113727462912467));
#30479=CARTESIAN_POINT('',(-0.000859075264311106,-0.00600346944668868,-0.0113003031226866));
#30480=CARTESIAN_POINT('',(-0.00174319314868272,-0.00580912084620773,-0.0112640816714646));
#30481=CARTESIAN_POINT('',(-0.00334323398092842,-0.00505940150515071,-0.0111916381296202));
#30482=CARTESIAN_POINT('',(-0.0040593972898715,-0.00450604234934652,-0.0111554168625309));
#30483=CARTESIAN_POINT('',(-0.00518533147390755,-0.00314408804019317,-0.0110829732546983));
#30484=CARTESIAN_POINT('',(-0.00559593301943456,-0.00233775978428837,-0.0110467519529574));
#30485=CARTESIAN_POINT('',(-0.00603184192596513,-0.000625158391190649,-0.0109743084975298));
#30486=CARTESIAN_POINT('',(-0.00605787853325042,0.000279212400784205,-0.010938087022621));
#30487=CARTESIAN_POINT('',(-0.00572024012570424,0.00201390634250815,-0.0108656438340358));
#30488=CARTESIAN_POINT('',(-0.00535668865032753,0.00284240619482864,-0.0108294221372547));
#30489=CARTESIAN_POINT('',(-0.00431023182100595,0.00426646668808826,-0.0107569792181002));
#30490=CARTESIAN_POINT('',(-0.00362704403416047,0.0048598136669573,-0.0107207573438761));
#30491=CARTESIAN_POINT('',(-0.00207241394588092,0.00569991648120368,-0.0106483145848017));
#30492=CARTESIAN_POINT('',(-0.00120093480390402,0.00594422095445996,-0.0106120926674817));
#30493=CARTESIAN_POINT('',(0.000563511232301897,0.00603877277129276,-0.0105396498550195));
#30494=CARTESIAN_POINT('',(0.00145603076803849,0.00588742838004165,-0.01050342810943));
#30495=CARTESIAN_POINT('',(0.003091110347539,0.0052177286750386,-0.0104309849408669));
#30496=CARTESIAN_POINT('',(0.00383355477573361,0.00469983671428884,-0.0103947634896458));
#30497=CARTESIAN_POINT('',(0.00502489458107504,0.00339487724234225,-0.0103223199478029));
#30498=CARTESIAN_POINT('',(0.00547478182306626,0.00260957621096752,-0.0102860986807135));
#30499=CARTESIAN_POINT('',(0.00599381202091714,0.000920418142363337,-0.0102136550728794));
#30500=CARTESIAN_POINT('',(0.00606458992024415,1.83375614756708E-5,-0.0101774337711432));
#30501=CARTESIAN_POINT('',(0.00581193305766793,-0.00173071492951537,-0.0101049903157079));
#30502=CARTESIAN_POINT('',(0.00548990002742215,-0.00257620837226416,-0.0100687688408028));
#30503=CARTESIAN_POINT('',(0.00451412418157153,-0.00404964797549366,-0.00999632565221761));
#30504=CARTESIAN_POINT('',(0.00386119324725615,-0.00467595690529434,-0.00996010395543582));
#30505=CARTESIAN_POINT('',(0.00234942884354364,-0.00559115555682603,-0.00988766103628286));
#30506=CARTESIAN_POINT('',(0.00149118157195093,-0.00587789203903946,-0.00985143916205724));
#30507=CARTESIAN_POINT('',(-0.000266602775728381,-0.00605911465611149,-0.00977899640298428));
#30508=CARTESIAN_POINT('',(-0.00116523579238055,-0.00595132192935385,-0.00974277448566356));
#30509=CARTESIAN_POINT('',(-0.0028315547852557,-0.00536345215233157,-0.00967033167320129));
#30510=CARTESIAN_POINT('',(-0.00359821832558892,-0.00488207572751732,-0.00963410992760799));
#30511=CARTESIAN_POINT('',(-0.00485255190132513,-0.00363763601143704,-0.00956166675905256));
#30512=CARTESIAN_POINT('',(-0.00534029243944068,-0.00287504504673827,-0.00952544530782837));
#30513=CARTESIAN_POINT('',(-0.00594156053203977,-0.00121351369403066,-0.00945300176598398));
#30514=CARTESIAN_POINT('',(-0.00605668045273713,-0.000315825750337319,-0.00941678049889378));
#30515=CARTESIAN_POINT('',(-0.00588978902176606,0.00144337707403134,-0.00934433689106272));
#30516=CARTESIAN_POINT('',(-0.00560996798134601,0.00230387638883739,-0.0093081155893231));
#30517=CARTESIAN_POINT('',(-0.00470721006664119,0.00382310259118043,-0.00923567213389156));
#30518=CARTESIAN_POINT('',(-0.00408613400847974,0.00448099997245,-0.00919945065898276));
#30519=CARTESIAN_POINT('',(-0.0026207737514388,0.00546886741436465,-0.00912700747040132));
#30520=CARTESIAN_POINT('',(-0.00177786617410126,0.00579763556459996,-0.00909078577361959));
#30521=CARTESIAN_POINT('',(-3.09466222681958E-5,0.00606464167597443,-0.00901834285446272));
#30522=CARTESIAN_POINT('',(0.000871699766989816,0.00600111463142254,-0.00898212098023906));
#30523=CARTESIAN_POINT('',(0.00256503164149829,0.00549586755061753,-0.0089096782211661));
#30524=CARTESIAN_POINT('',(0.00335400980216468,0.00505238808937253,-0.00887345630384614));
#30525=CARTESIAN_POINT('',(0.00466851979026242,0.00387159456299146,-0.00880101349138235));
#30526=CARTESIAN_POINT('',(0.00519260976097037,0.0031334713015793,-0.00876479174579288));
#30527=CARTESIAN_POINT('',(0.00587523641665553,0.00150374624037253,-0.00869234857723131));
#30528=CARTESIAN_POINT('',(0.0060340189891069,0.000612553833172357,-0.00865612712601019));
#30529=CARTESIAN_POINT('',(0.00595367775238934,-0.00115259631367031,-0.00858368358416579));
#30530=CARTESIAN_POINT('',(0.0057165043874037,-0.00202600631780788,-0.00854746231707637));
#30531=CARTESIAN_POINT('',(0.00488909903514167,-0.00358743121515669,-0.00847501870924377));
#30532=CARTESIAN_POINT('',(0.00430127927179329,-0.00427534604365617,-0.00843879740750493));
#30533=CARTESIAN_POINT('',(0.00288585701391485,-0.00533345753983467,-0.00836635395207338));
#30534=CARTESIAN_POINT('',(0.0020602911276489,-0.00570359994720765,-0.00833013247716457));
#30535=CARTESIAN_POINT('',(0.000328434275016982,-0.00605550136479379,-0.00825768928858313));
#30536=CARTESIAN_POINT('',(-0.000576124907666656,-0.00603667676488749,-0.00822146759180141));
#30537=CARTESIAN_POINT('',(-0.00229224694171241,-0.00561484107607418,-0.00814902467264454));
#30538=CARTESIAN_POINT('',(-0.00310187271838032,-0.00521072192139484,-0.00811280279842165));
#30539=CARTESIAN_POINT('',(-0.004472957691924,-0.00409592443072183,-0.00804036003934715));
#30540=CARTESIAN_POINT('',(-0.00503216622374263,-0.00338427396279622,-0.00800413812202796));
#30541=CARTESIAN_POINT('',(-0.00579474497744008,-0.00179032179752817,-0.00793169530956417));
#30542=CARTESIAN_POINT('',(-0.00599647343138397,-0.000907824274979786,-0.00789547356397393));
#30543=CARTESIAN_POINT('',(-0.00600346944668562,0.000859075264311016,-0.00782303039541389));
#30544=CARTESIAN_POINT('',(-0.00580912084621274,0.0017431931486827,-0.00778680894419278));
#30545=CARTESIAN_POINT('',(-0.00505940150514794,0.00334323398092366,-0.00771436540234685));
#30546=CARTESIAN_POINT('',(-0.00450604234934851,0.00405939728987541,-0.00767814413525819));
#30547=CARTESIAN_POINT('',(-0.00314408804019073,0.00518533147390397,-0.00760570052742559));
#30548=CARTESIAN_POINT('',(-0.00233775978429126,0.00559593301943496,-0.00756947922568675));
#30549=CARTESIAN_POINT('',(-0.000625158391191966,0.00603184192596372,-0.00749703577025521));
#30550=CARTESIAN_POINT('',(0.000279212400785439,0.00605787853325739,-0.0074608142953487));
#30551=CARTESIAN_POINT('',(0.00201390634250682,0.0057202401256973,-0.00738837110676266));
#30552=CARTESIAN_POINT('',(0.00284240619482905,0.00535668865032929,-0.0073521494099817));
#30553=CARTESIAN_POINT('',(0.00426646668808612,0.00431023182100547,-0.0072797064908279));
#30554=CARTESIAN_POINT('',(0.00485981366694846,0.00362704403415547,-0.00724348461660347));
#30555=CARTESIAN_POINT('',(0.00569991648121184,0.00207241394588719,-0.00717104185752897));
#30556=CARTESIAN_POINT('',(0.00594422095445765,0.00120093480390459,-0.00713481994020902));
#30557=CARTESIAN_POINT('',(0.00603877277129507,-0.00056351123230199,-0.00706237712774675));
#30558=CARTESIAN_POINT('',(0.0058874283800451,-0.00145603076804085,-0.0070261553821569));
#30559=CARTESIAN_POINT('',(0.00521772867503515,-0.00309111034753677,-0.00695371221359457));
#30560=CARTESIAN_POINT('',(0.00469983671428812,-0.00383355477573512,-0.006917490762375));
#30561=CARTESIAN_POINT('',(0.00339487724234326,-0.00502489458107331,-0.00684504722052831));
#30562=CARTESIAN_POINT('',(0.00260957621096805,-0.00547478182307112,-0.00680882595343965));
#30563=CARTESIAN_POINT('',(0.00092041814236392,-0.00599381202091195,-0.00673638234560783));
#30564=CARTESIAN_POINT('',(1.83375614742641E-5,-0.00606458992025192,-0.00670016104386784));
#30565=CARTESIAN_POINT('',(-0.00173071492951204,-0.00581193305766056,-0.00662771758843784));
#30566=CARTESIAN_POINT('',(-0.00257620837226887,-0.00548990002742911,-0.00659149611352898));
#30567=CARTESIAN_POINT('',(-0.00404964797548944,-0.00451412418156432,-0.00651905292494602));
#30568=CARTESIAN_POINT('',(-0.00467595690530402,-0.00386119324726373,-0.00648283122816474));
#30569=CARTESIAN_POINT('',(-0.00559115555681467,-0.002349428843539,-0.00641038830900865));
#30570=CARTESIAN_POINT('',(-0.00587789203904983,-0.00149118157195279,-0.00637416643478492));
#30571=CARTESIAN_POINT('',(-0.00605911465610112,0.000266602775729709,-0.0063017236757112));
#30572=CARTESIAN_POINT('',(-0.0059513219293497,0.00116523579237788,-0.00626550175839094));
#30573=CARTESIAN_POINT('',(-0.00536345215233749,0.00283155478525354,-0.00619305894592869));
#30574=CARTESIAN_POINT('',(-0.0048820757275079,0.00359821832558035,-0.00615683720033756));
#30575=CARTESIAN_POINT('',(-0.00363763601144603,0.0048525519013342,-0.00608439403177752));
#30576=CARTESIAN_POINT('',(-0.00287504504674204,0.00534029243944514,-0.00604817258055424));
#30577=CARTESIAN_POINT('',(-0.00121351369403187,0.00594156053203358,-0.0059757290387129));
#30578=CARTESIAN_POINT('',(-0.00031582575033843,0.00605668045273254,-0.00593950777162106));
#30579=CARTESIAN_POINT('',(0.00144337707403289,0.00588978902177064,-0.00586706416378998));
#30580=CARTESIAN_POINT('',(0.00230387638884796,0.00560996798136351,-0.00583084286204893));
#30581=CARTESIAN_POINT('',(0.00382310259116669,0.00470721006662557,-0.00575839940662044));
#30582=CARTESIAN_POINT('',(0.00448099997245725,0.00408613400848599,-0.0057221779317101));
#30583=CARTESIAN_POINT('',(0.00546886741435594,0.00262077375143485,-0.00564973474312865));
#30584=CARTESIAN_POINT('',(0.00579763556459787,0.00177786617410278,-0.00561351304634461));
#30585=CARTESIAN_POINT('',(0.00606464167597621,3.0946622268693E-5,-0.00554107012719234));
#30586=CARTESIAN_POINT('',(0.00600111463141991,-0.000871699766989554,-0.0055048482529664));
#30587=CARTESIAN_POINT('',(0.00549586755062006,-0.00256503164149915,-0.0054324054938933));
#30588=CARTESIAN_POINT('',(0.00505238808936695,-0.00335400980216068,-0.00539618357657267));
#30589=CARTESIAN_POINT('',(0.00387159456299719,-0.00466851979026632,-0.00532374076411039));
#30590=CARTESIAN_POINT('',(0.00313347130158231,-0.00519260976097808,-0.00528751901851862));
#30591=CARTESIAN_POINT('',(0.00150374624036927,-0.00587523641664796,-0.00521507584996011));
#30592=CARTESIAN_POINT('',(0.000612553833171035,-0.00603401898911497,-0.00517885439873749));
#30593=CARTESIAN_POINT('',(-0.00115259631366817,-0.00595367775238131,-0.0051064108568931));
#30594=CARTESIAN_POINT('',(-0.00202600631781078,-0.00571650438740787,-0.00507018958980372));
#30595=CARTESIAN_POINT('',(-0.00358743121515375,-0.00488909903513752,-0.00499774598197099));
#30596=CARTESIAN_POINT('',(-0.00427534604366103,-0.00430127927179586,-0.00496152468023219));
#30597=CARTESIAN_POINT('',(-0.00533345753983033,-0.00288585701391166,-0.00488908122480065));
#30598=CARTESIAN_POINT('',(-0.00570359994720922,-0.00206029112764941,-0.00485285974989415));
#30599=CARTESIAN_POINT('',(-0.00605550136479229,-0.000328434275016135,-0.00478041656130811));
#30600=CARTESIAN_POINT('',(-0.00603667676488204,0.000576124907666373,-0.00474419486452637));
#30601=CARTESIAN_POINT('',(-0.00561484107607947,0.00229224694171347,-0.00467175194537411));
#30602=CARTESIAN_POINT('',(-0.00521072192140026,0.00310187271838521,-0.00463553007114899));
#30603=CARTESIAN_POINT('',(-0.00409592443071614,0.00447295769191944,-0.00456308731207436));
#30604=CARTESIAN_POINT('',(-0.00338427396279826,0.00503216622374612,-0.00452686539475448));
#30605=CARTESIAN_POINT('',(-0.00179032179752601,0.00579474497743666,-0.00445442258229221));
#30606=CARTESIAN_POINT('',(-0.000907824274979335,0.0059964734313974,-0.00441820083669967));
#30607=CARTESIAN_POINT('',(0.00085907526431096,0.00600346944667221,-0.0043457576681427));
#30608=CARTESIAN_POINT('',(0.00174319314868342,0.00580912084621372,-0.00430953621691928));
#30609=CARTESIAN_POINT('',(0.00334323398092361,0.00505940150514661,-0.00423709267507489));
#30610=CARTESIAN_POINT('',(0.00405939728986873,0.00450604234934388,-0.00420087140798552));
#30611=CARTESIAN_POINT('',(0.00518533147391094,0.00314408804019501,-0.00412842780015279));
#30612=CARTESIAN_POINT('',(0.00559593301943005,0.00233775978429005,-0.00409220649841479));
#30613=CARTESIAN_POINT('',(0.00603184192596878,0.000625158391192479,-0.00401976304298171));
#30614=CARTESIAN_POINT('',(0.00605787853326322,-0.000279212400785085,-0.00398354156807523));
#30615=CARTESIAN_POINT('',(0.00572024012569162,-0.00201390634250648,-0.00391109837949073));
#30616=CARTESIAN_POINT('',(0.00535668865032563,-0.00284240619482649,-0.0038748766827105));
#30617=CARTESIAN_POINT('',(0.00431023182100872,-0.0042664666880893,-0.00380243376355363));
#30618=CARTESIAN_POINT('',(0.00362704403415923,-0.00485981366695353,-0.00376621188933157));
#30619=CARTESIAN_POINT('',(0.00207241394588276,-0.00569991648120711,-0.0036937691302554));
#30620=CARTESIAN_POINT('',(0.00120093480390449,-0.00594422095445802,-0.00365754721293706));
#30621=CARTESIAN_POINT('',(-0.000563511232301889,-0.00603877277129467,-0.00358510440047326));
#30622=CARTESIAN_POINT('',(-0.00145603076803988,-0.00588742838004119,-0.00354888265488379));
#30623=CARTESIAN_POINT('',(-0.00309111034753821,-0.00521772867503886,-0.00347643948632222));
#30624=CARTESIAN_POINT('',(-0.00383355477573305,-0.00469983671428823,-0.00344021803510188));
#30625=CARTESIAN_POINT('',(-0.005024894581076,-0.00339487724234243,-0.00336777449325594));
#30626=CARTESIAN_POINT('',(-0.00547478182306962,-0.00260957621096737,-0.00333155322616581));
#30627=CARTESIAN_POINT('',(-0.00599381202091404,-0.000920418142362637,-0.00325910961833615));
#30628=CARTESIAN_POINT('',(-0.00606458992025173,-1.83375614733508E-5,-0.00322288831659661));
#30629=CARTESIAN_POINT('',(-0.00581193305766033,0.00173071492951357,-0.00315044486116353));
#30630=CARTESIAN_POINT('',(-0.00548990002742595,0.00257620837226724,-0.00311422338625548));
#30631=CARTESIAN_POINT('',(-0.00451412418156716,0.00404964797549147,-0.00304178019767404));
#30632=CARTESIAN_POINT('',(-0.00386119324726109,0.00467595690530463,-0.00300555850089079));
#30633=CARTESIAN_POINT('',(-0.00234942884353807,0.00559115555681618,-0.00293311558173699));
#30634=CARTESIAN_POINT('',(-0.00149118157195182,0.00587789203904661,-0.00289689370751264));
#30635=CARTESIAN_POINT('',(0.000266602775729427,0.0060591146561044,-0.00282445094843801));
#30636=CARTESIAN_POINT('',(0.00116523579237932,0.00595132192934975,-0.00278822903111813));
#30637=CARTESIAN_POINT('',(0.00283155478525638,0.00536345215233592,-0.00271578621865587));
#30638=CARTESIAN_POINT('',(0.00359821832558002,0.00488207572750747,-0.00267956447306408));
#30639=CARTESIAN_POINT('',(0.00485255190133472,0.00363763601144627,-0.00260712130450557));
#30640=CARTESIAN_POINT('',(0.00534029243944329,0.0028750450467383,-0.00257089985328367));
#30641=CARTESIAN_POINT('',(0.00594156053203786,0.00121351369402893,-0.00249845631143773));
#30642=CARTESIAN_POINT('',(0.00605668045272946,0.00031582575033894,-0.00246223504434917));
#30643=CARTESIAN_POINT('',(0.00588978902177369,-0.00144337707403387,-0.00238979143651642));
#30644=CARTESIAN_POINT('',(0.00560996798136092,-0.00230387638884949,-0.00235357013477837));
#30645=CARTESIAN_POINT('',(0.00470721006662452,-0.00382310259117127,-0.00228112667934528));
#30646=CARTESIAN_POINT('',(0.00408613400848635,-0.00448099997246406,-0.00224490520443801));
#30647=CARTESIAN_POINT('',(0.00262077375142909,-0.00546886741435278,-0.00217246201585504));
#30648=CARTESIAN_POINT('',(0.00177786617409953,-0.00579763556459878,-0.00213624031907329));
#30649=CARTESIAN_POINT('',(3.09466222649569E-5,-0.00606464167597636,-0.00206379739991795));
#30650=CARTESIAN_POINT('',(-0.000871699766989641,-0.00600111463142063,-0.00202757552569444));
#30651=CARTESIAN_POINT('',(-0.0025650316414994,-0.00549586755061925,-0.00195513276661981));
#30652=CARTESIAN_POINT('',(-0.00335400980216594,-0.0050523880893681,-0.00191891084930058));
#30653=CARTESIAN_POINT('',(-0.00466851979026617,-0.00387159456299146,-0.00184646803683676));
#30654=CARTESIAN_POINT('',(-0.00519260976097701,-0.00313347130158175,-0.0018102462912459));
#30655=CARTESIAN_POINT('',(-0.00587523641664912,-0.00150374624036962,-0.0017378031226874));
#30656=CARTESIAN_POINT('',(-0.00603401898911557,-0.00061255383316749,-0.00170158167146463));
#30657=CARTESIAN_POINT('',(-0.00595367775238039,0.00115259631367158,-0.00162913812962024));
#30658=CARTESIAN_POINT('',(-0.00571650438740898,0.00202600631781163,-0.00159291686253176));
#30659=CARTESIAN_POINT('',(-0.00488909903513646,0.00358743121515282,-0.00152047325469751));
#30660=CARTESIAN_POINT('',(-0.0043012792717929,0.0042753460436607,-0.00148425195295939));
#30661=CARTESIAN_POINT('',(-0.00288585701391163,0.00533345753983288,-0.00141180849752786));
#30662=CARTESIAN_POINT('',(-0.00206029112764908,0.00570359994721081,-0.00137558702261988));
#30663=CARTESIAN_POINT('',(-0.000328434275016096,0.00605550136479076,-0.00130314383403692));
#30664=CARTESIAN_POINT('',(0.000576124907667665,0.00603667676488167,-0.00126692213725589));
#30665=CARTESIAN_POINT('',(0.00229224694171486,0.00561484107607917,-0.00119447921809904));
#30666=CARTESIAN_POINT('',(0.00310187271838672,0.00521072192140026,-0.00115825734387622));
#30667=CARTESIAN_POINT('',(0.00447295769191957,0.00409592443071479,-0.00108581458480161));
#30668=CARTESIAN_POINT('',(0.00503216622374031,0.00338427396279337,-0.00104959266748173));
#30669=CARTESIAN_POINT('',(0.005794744977443,0.0017903217975298,-0.000977149855019475));
#30670=CARTESIAN_POINT('',(0.00599647343139357,0.000907824274979128,-0.000940928109428471));
#30671=CARTESIAN_POINT('',(0.00600346944667604,-0.000859075264311266,-0.000868484940868442));
#30672=CARTESIAN_POINT('',(0.00580912084621264,-0.0017431931486827,-0.0008322634896458));
#30673=CARTESIAN_POINT('',(0.00505940150514784,-0.00334323398092403,-0.000759819947802938));
#30674=CARTESIAN_POINT('',(0.00450604234934318,-0.00405939728986845,-0.000723598680712034));
#30675=CARTESIAN_POINT('',(0.00314408804019546,-0.00518533147391142,-0.000651155072880834));
#30676=CARTESIAN_POINT('',(0.00233775978428977,-0.00559593301942972,-0.000614933771140532));
#30677=CARTESIAN_POINT('',(0.000625158391192401,-0.00603184192596921,-0.000542490315710523));
#30678=CARTESIAN_POINT('',(-0.000279212400785806,-0.00605787853326039,-0.000506268840800958));
#30679=CARTESIAN_POINT('',(-0.00201390634250717,-0.00572024012569417,-0.000433825652219523));
#30680=CARTESIAN_POINT('',(-0.00284240619482663,-0.00535668865032544,-0.000397603955437035));
#30681=CARTESIAN_POINT('',(-0.00426646668808866,-0.0043102318210093,-0.000325161036281701));
#30682=CARTESIAN_POINT('',(-0.00485981366695287,-0.00362704403415734,-0.000288939162058086));
#30683=CARTESIAN_POINT('',(-0.00569991648120799,-0.00207241394588432,-0.000216496402983457));
#30684=CARTESIAN_POINT('',(-0.0059442209544565,-0.00120093480390377,-0.000180274485662048));
#30685=CARTESIAN_POINT('',(-0.00603877277129622,0.000563511232301556,-0.000107831673202851));
#30686=CARTESIAN_POINT('',(-0.00588742838004495,0.00145603076804102,-7.16099276087707E-5));
#30687=CARTESIAN_POINT('',(-0.00521772867503495,0.00309111034753743,8.33240948196383E-7));
#30688=CARTESIAN_POINT('',(-0.00469983671428809,0.00383355477573433,3.70546921731411E-5));
#30689=CARTESIAN_POINT('',(-0.00339487724234229,0.00502489458107499,0.000109498234014469));
#30690=CARTESIAN_POINT('',(-0.00260957621096751,0.00547478182307082,0.000145719501104603));
#30691=CARTESIAN_POINT('',(-0.000920418142362202,0.00599381202091294,0.000218163108938871));
#30692=CARTESIAN_POINT('',(-1.83375614725771E-5,0.00606458992025286,0.00025438441067611));
#30693=CARTESIAN_POINT('',(0.00173071492951319,0.00581193305765916,0.000326827866109187));
#30694=CARTESIAN_POINT('',(0.00257620837226795,0.00548990002742626,0.000363049341015702));
#30695=CARTESIAN_POINT('',(0.00404964797549103,0.0045141241815667,0.000435492529600207));
#30696=CARTESIAN_POINT('',(0.00467595690530011,0.00386119324726,0.000471714226381924));
#30697=CARTESIAN_POINT('',(0.00559115555682087,0.00234942884353889,0.000544157145535723));
#30698=CARTESIAN_POINT('',(0.00587789203904666,0.00149118157195146,0.000580379019759321));
#30699=CARTESIAN_POINT('',(0.00605911465610445,-0.000266602775729979,0.000652821778835484));
#30700=CARTESIAN_POINT('',(0.00595132192935104,-0.0011652357923806,0.000689043696154603));
#30701=CARTESIAN_POINT('',(0.00536345215233414,-0.0028315547852565,0.000761486508616866));
#30702=CARTESIAN_POINT('',(0.00488207572750542,-0.00359821832557824,0.000797708254208643));
#30703=CARTESIAN_POINT('',(0.00363763601144815,-0.00485255190133669,0.000870151422767143));
#30704=CARTESIAN_POINT('',(0.0028750450467372,-0.00534029243944135,0.000906372873988264));
#30705=CARTESIAN_POINT('',(0.00121351369403036,-0.00594156053203968,0.000978816415835729));
#30706=CARTESIAN_POINT('',(0.000315825750338376,-0.00605668045273214,0.00101503768292201));
#30707=CARTESIAN_POINT('',(-0.0014433770740335,-0.00588978902177103,0.00108748129075781));
#30708=CARTESIAN_POINT('',(-0.0023038763888485,-0.00560996798135989,0.00112370259249429));
#30709=CARTESIAN_POINT('',(-0.00382310259117005,-0.0047072100666267,0.00119614604792737));
#30710=CARTESIAN_POINT('',(-0.00448099997246035,-0.00408613400848585,0.00123236752283539));
#30711=CARTESIAN_POINT('',(-0.00546886741435506,-0.00262077375143265,0.00130481071141683));
#30712=CARTESIAN_POINT('',(-0.00579763556459847,-0.0017778661740996,0.00134103240820018));
#30713=CARTESIAN_POINT('',(-0.00606464167597601,-3.09466222654928E-5,0.00141347532735398));
#30714=CARTESIAN_POINT('',(-0.00600111463141992,0.000871699766980109,0.00144969720157956));
#30715=CARTESIAN_POINT('',(-0.00549586755062015,0.00256503164149748,0.00152213996065112));
#30716=CARTESIAN_POINT('',(-0.00505238808936944,0.00335400980220972,0.00155836187797583));
#30717=CARTESIAN_POINT('',(-0.00387159456298909,0.00466851979024306,0.00163080469043323));
#30718=CARTESIAN_POINT('',(-0.00313347130160139,0.00519260976081515,0.00166702643602028));
#30719=CARTESIAN_POINT('',(-0.00150374624037983,0.00587523641686614,0.00173946960459158));
#30720=CARTESIAN_POINT('',(-0.000612553833165579,0.00603401898939451,0.00177569105583878));
#30721=CARTESIAN_POINT('',(0.00115259631371467,0.0059536777513449,0.00184813459759908));
#30722=CARTESIAN_POINT('',(0.00202600631845691,0.00571650438746742,0.00188435586467389));
#30723=CARTESIAN_POINT('',(0.00358743121405334,0.00488909903965777,0.00195679947282889));
#30724=CARTESIAN_POINT('',(0.00427534604012664,0.00430127926719982,0.0019930207743065));
#30725=CARTESIAN_POINT('',(0.00533345754995747,0.00288585699514267,0.00206546422868242));
#30726=CARTESIAN_POINT('',(0.00570359995483104,0.0020602911659135,0.00210168570590789));
#30727=CARTESIAN_POINT('',(0.00605550130478085,0.000328434353748034,0.00217412889706531));
#30728=CARTESIAN_POINT('',(0.00603667678110669,-0.000576125165779344,0.00221035058020653));
#30729=CARTESIAN_POINT('',(0.0056148413322424,-0.00229224724916889,0.00228279349810771));
#30730=CARTESIAN_POINT('',(0.00521072173073282,-0.00310187120641182,0.00231901543922011));
#30731=CARTESIAN_POINT('',(0.00409592363987556,-0.00447295679573389,0.00239145815903209));
#30732=CARTESIAN_POINT('',(0.00338427466196768,-0.00503217385805823,0.00242767978760003));
#30733=CARTESIAN_POINT('',(0.00179032336308774,-0.00579474532206606,0.00250012295961856));
#30734=CARTESIAN_POINT('',(0.000907823357868306,-0.00599643245723689,0.00253634580897236));
#30735=CARTESIAN_POINT('',(-0.00154620346649854,-0.00600624349949343,0.00263695810271456));
#30736=CARTESIAN_POINT('',(-0.00311036825890238,-0.00536525626263524,0.00270138359384264));
#30737=CARTESIAN_POINT('',(-0.00534036428216497,-0.00315440800084661,0.00283011272614596));
#30738=CARTESIAN_POINT('',(-0.005993747924043,-0.00158510314530943,0.00289494802175126));
#30739=CARTESIAN_POINT('',(-0.00599994287806968,-2.43712307521179E-5,0.00295892997067846));
#30740=CARTESIAN_POINT('',(-2.02817453607845E-19,-2.44158234687783E-19,
0.022618891118261));
#30741=CARTESIAN_POINT('',(0.00365907271966709,-0.00718133456002582,0.065));
#30742=CARTESIAN_POINT('',(-0.0226621510894003,-0.0205926679525846,0.065));
#30743=CARTESIAN_POINT('',(-0.0222081605896608,-0.0214836744767729,0.065));
#30744=CARTESIAN_POINT('',(-0.0226621510894003,-0.0205926679525846,0.064));
#30745=CARTESIAN_POINT('',(0.00365907271966709,-0.00718133456002582,0.064));
#30746=CARTESIAN_POINT('',(-0.00364987616131558,-0.0109054300239403,0.064));
#30747=CARTESIAN_POINT('',(-0.00356046479940298,-0.0119821988972063,0.065));
#30748=CARTESIAN_POINT('',(-0.00356046479940298,-0.0119821988972063,0.0647249369217302));
#30749=CARTESIAN_POINT('',(-0.00358442462146283,-0.0117264212762759,0.064195847752999));
#30750=CARTESIAN_POINT('',(-0.00362978387837724,-0.0111757204745938,0.064));
#30751=CARTESIAN_POINT('',(-0.00364987616131558,-0.0109054300239404,0.064));
#30752=CARTESIAN_POINT('',(-0.00356046479940298,-0.0119821988972063,0.065));
#30753=CARTESIAN_POINT('',(0.00411306321940664,-0.00807234108421418,0.065));
#30754=CARTESIAN_POINT('',(0.,0.,0.065));
#30755=CARTESIAN_POINT('',(0.00294272257781457,-0.0111171212024526,0.065));
#30756=CARTESIAN_POINT('',(0.00294272257781457,-0.0111171212024526,0.064));
#30757=CARTESIAN_POINT('',(0.00319861149762453,-0.0120838273939702,0.065));
#30758=CARTESIAN_POINT('',(0.,0.,0.065));
#30759=CARTESIAN_POINT('',(0.,0.,0.064));
#30760=CARTESIAN_POINT('',(-0.0217541700899212,-0.0223746810009613,0.065));
#30761=CARTESIAN_POINT('',(-0.0227486623307711,-0.0206394619419116,0.065));
#30762=CARTESIAN_POINT('',(-0.0222514162103461,-0.0215070714714365,0.065));
#30763=CARTESIAN_POINT('',(-0.0227486623307711,-0.0206394619419116,0.064));
#30764=CARTESIAN_POINT('',(-0.0217541700899212,-0.0223746810009613,0.064));
#30765=CARTESIAN_POINT('',(-0.0217541700899212,-0.0223746810009613,0.065));
#30766=CARTESIAN_POINT('',(0.0034545004174345,-0.0130505335854878,0.065));
#30767=CARTESIAN_POINT('',(0.0043624814169136,-0.0112685205371111,0.065));
#30768=CARTESIAN_POINT('',(0.0043624814169136,-0.0112685205371111,0.064));
#30769=CARTESIAN_POINT('',(0.00390849091717405,-0.0121595270612994,0.065));
#30770=CARTESIAN_POINT('',(0.0034545004174345,-0.0130505335854878,0.065));
#30771=CARTESIAN_POINT('',(0.0034545004174345,-0.0130505335854878,0.064));
#30772=CARTESIAN_POINT('',(-0.0217541700899212,-0.0223746810009613,0.064));
#30773=CARTESIAN_POINT('',(-0.0217541700899212,-0.0223746810009613,0.066));
#30774=CARTESIAN_POINT('',(-0.0222081605896608,-0.0214836744767729,0.066));
#30775=CARTESIAN_POINT('',(-0.0222514162103461,-0.0215070714714365,0.066));
#30776=CARTESIAN_POINT('',(-0.0222514162103461,-0.0215070714714365,0.064));
#30777=CARTESIAN_POINT('',(-0.0222081605896608,-0.0214836744767729,0.064));
#30778=CARTESIAN_POINT('',(-0.0036590727196671,-0.00718133456002582,0.065));
#30779=CARTESIAN_POINT('',(0.0226621510894002,-0.0205926679525846,0.065));
#30780=CARTESIAN_POINT('',(0.0226621510894002,-0.0205926679525846,0.064));
#30781=CARTESIAN_POINT('',(0.0222081605896607,-0.0214836744767729,0.065));
#30782=CARTESIAN_POINT('',(0.0222307621135331,-0.0214951905283833,0.065));
#30783=CARTESIAN_POINT('',(0.00401445529914253,-0.011091192373018,0.064));
#30784=CARTESIAN_POINT('',(0.0034545004174345,-0.0130505335854878,0.064));
#30785=CARTESIAN_POINT('',(0.0034545004174345,-0.0130505335854878,0.066));
#30786=CARTESIAN_POINT('',(0.00390849091717405,-0.0121595270612994,0.066));
#30787=CARTESIAN_POINT('',(0.00319861149762453,-0.0120838273939702,0.066));
#30788=CARTESIAN_POINT('',(0.00319861149762453,-0.0120838273939702,0.064));
#30789=CARTESIAN_POINT('',(0.00390849091717405,-0.0121595270612994,0.064));
#30790=CARTESIAN_POINT('',(-0.0217541700899212,-0.0223746810009613,0.066));
#30791=CARTESIAN_POINT('',(-0.0217541700899212,-0.0223746810009613,0.067));
#30792=CARTESIAN_POINT('',(-0.0226621510894003,-0.0205926679525846,0.067));
#30793=CARTESIAN_POINT('',(-0.0227486623307711,-0.0206394619419116,0.067));
#30794=CARTESIAN_POINT('',(-0.0227486623307711,-0.0206394619419116,0.066));
#30795=CARTESIAN_POINT('',(-0.0226621510894003,-0.0205926679525846,0.066));
#30796=CARTESIAN_POINT('',(-0.0302541271933658,-0.00765232343563852,0.065));
#30797=CARTESIAN_POINT('',(-0.0291648491233358,-0.00932966457152937,0.065));
#30798=CARTESIAN_POINT('',(-0.0297094881583508,-0.00849099400358394,0.065));
#30799=CARTESIAN_POINT('',(-0.0291648491233358,-0.00932966457152937,0.064));
#30800=CARTESIAN_POINT('',(-0.0302541271933658,-0.00765232343563852,0.064));
#30801=CARTESIAN_POINT('',(-0.0292486295275229,-0.00938118850960592,0.064));
#30802=CARTESIAN_POINT('',(-0.0292486295275229,-0.00938118850960592,0.065));
#30803=CARTESIAN_POINT('',(-0.0297513783604443,-0.00851675597262222,0.065));
#30804=CARTESIAN_POINT('',(-0.0302541271933658,-0.00765232343563852,0.065));
#30805=CARTESIAN_POINT('',(0.0217541700899211,-0.0223746810009612,0.065));
#30806=CARTESIAN_POINT('',(0.022748662330771,-0.0206394619419116,0.065));
#30807=CARTESIAN_POINT('',(0.022748662330771,-0.0206394619419116,0.064));
#30808=CARTESIAN_POINT('',(0.022251416210346,-0.0215070714714364,0.065));
#30809=CARTESIAN_POINT('',(0.0217541700899211,-0.0223746810009612,0.065));
#30810=CARTESIAN_POINT('',(0.0217541700899211,-0.0223746810009612,0.064));
#30811=CARTESIAN_POINT('',(0.0034545004174345,-0.0130505335854878,0.066));
#30812=CARTESIAN_POINT('',(0.0034545004174345,-0.0130505335854878,0.067));
#30813=CARTESIAN_POINT('',(0.0043624814169136,-0.0112685205371111,0.067));
#30814=CARTESIAN_POINT('',(0.00294272257781457,-0.0111171212024526,0.067));
#30815=CARTESIAN_POINT('',(0.00294272257781457,-0.0111171212024526,0.066));
#30816=CARTESIAN_POINT('',(0.0043624814169136,-0.0112685205371111,0.066));
#30817=CARTESIAN_POINT('',(0.00365907271966709,-0.00718133456002582,0.066));
#30818=CARTESIAN_POINT('',(-0.00356046479940298,-0.0119821988972063,0.066));
#30819=CARTESIAN_POINT('',(-0.00356046479940298,-0.0119821988972063,0.0662750630782698));
#30820=CARTESIAN_POINT('',(-0.00358442462146302,-0.0117264212762759,0.066804152247001));
#30821=CARTESIAN_POINT('',(-0.00362978387837688,-0.0111757204745937,0.067));
#30822=CARTESIAN_POINT('',(-0.00364987616131558,-0.0109054300239404,0.067));
#30823=CARTESIAN_POINT('',(-0.00356046479940298,-0.0119821988972063,0.066));
#30824=CARTESIAN_POINT('',(-0.00364987616131558,-0.0109054300239403,0.067));
#30825=CARTESIAN_POINT('',(-0.00401445529914253,-0.011091192373018,0.067));
#30826=CARTESIAN_POINT('',(-0.0222307621135331,-0.0214951905283833,0.066));
#30827=CARTESIAN_POINT('',(-0.0302541271933658,-0.00765232343563852,0.064));
#30828=CARTESIAN_POINT('',(-0.0302541271933658,-0.00765232343563852,0.066));
#30829=CARTESIAN_POINT('',(-0.0297513783604443,-0.00851675597262222,0.066));
#30830=CARTESIAN_POINT('',(-0.0297094881583508,-0.00849099400358394,0.066));
#30831=CARTESIAN_POINT('',(-0.0297094881583508,-0.00849099400358394,0.067));
#30832=CARTESIAN_POINT('',(-0.0297513783604443,-0.00851675597262222,0.064));
#30833=CARTESIAN_POINT('',(-0.00438968180222396,0.00675951720953923,0.065));
#30834=CARTESIAN_POINT('',(-0.0119400657566617,0.00185624053797081,0.065));
#30835=CARTESIAN_POINT('',(-0.0124847047916767,0.00269491110591624,0.065));
#30836=CARTESIAN_POINT('',(-0.0119400657566617,0.00185624053797081,0.064));
#30837=CARTESIAN_POINT('',(-0.011612482002865,0.00206897591509449,0.064));
#30838=CARTESIAN_POINT('',(-0.0297307621135331,-0.00850480947161671,0.065));
#30839=CARTESIAN_POINT('',(0.0259807621135331,-0.015,0.065));
#30840=CARTESIAN_POINT('',(0.029248629527523,-0.00938118850960603,0.065));
#30841=CARTESIAN_POINT('',(0.029248629527523,-0.00938118850960603,0.064));
#30842=CARTESIAN_POINT('',(0.0297513783604445,-0.00851675597262234,0.065));
#30843=CARTESIAN_POINT('',(0.0259807621135331,-0.015,0.065));
#30844=CARTESIAN_POINT('',(0.0259807621135331,-0.015,0.064));
#30845=CARTESIAN_POINT('',(0.0217541700899211,-0.0223746810009612,0.064));
#30846=CARTESIAN_POINT('',(0.0217541700899211,-0.0223746810009612,0.066));
#30847=CARTESIAN_POINT('',(0.022251416210346,-0.0215070714714364,0.066));
#30848=CARTESIAN_POINT('',(0.0222081605896607,-0.0214836744767729,0.066));
#30849=CARTESIAN_POINT('',(0.0222081605896607,-0.0214836744767729,0.067));
#30850=CARTESIAN_POINT('',(0.022251416210346,-0.0215070714714364,0.064));
#30851=CARTESIAN_POINT('',(-0.0036590727196671,-0.00718133456002582,0.066));
#30852=CARTESIAN_POINT('',(0.0226621510894002,-0.0205926679525846,0.066));
#30853=CARTESIAN_POINT('',(0.0226621510894002,-0.0205926679525846,0.067));
#30854=CARTESIAN_POINT('',(-0.0036590727196671,-0.00718133456002582,0.067));
#30855=CARTESIAN_POINT('',(-0.00411306321940666,-0.00807234108421419,0.066));
#30856=CARTESIAN_POINT('',(0.,0.,0.066));
#30857=CARTESIAN_POINT('',(0.,0.,0.067));
#30858=CARTESIAN_POINT('',(0.,0.,0.066));
#30859=CARTESIAN_POINT('',(-0.0302541271933658,-0.00765232343563852,0.066));
#30860=CARTESIAN_POINT('',(-0.0302541271933658,-0.00765232343563852,0.067));
#30861=CARTESIAN_POINT('',(-0.0292486295275229,-0.00938118850960592,0.067));
#30862=CARTESIAN_POINT('',(-0.0291648491233358,-0.00932966457152937,0.067));
#30863=CARTESIAN_POINT('',(-0.0291648491233358,-0.00932966457152937,0.066));
#30864=CARTESIAN_POINT('',(-0.0292486295275229,-0.00938118850960592,0.066));
#30865=CARTESIAN_POINT('',(-0.0130293438266917,0.00353358167386167,0.065));
#30866=CARTESIAN_POINT('',(-0.0110990706671818,0.00301008809254883,0.065));
#30867=CARTESIAN_POINT('',(-0.0120642072469368,0.00327183488320525,0.065));
#30868=CARTESIAN_POINT('',(-0.0110990706671818,0.00301008809254883,0.064));
#30869=CARTESIAN_POINT('',(-0.0130293438266917,0.00353358167386167,0.064));
#30870=CARTESIAN_POINT('',(-0.0130293438266917,0.00353358167386167,0.065));
#30871=CARTESIAN_POINT('',(0.030254127193366,-0.00765232343563865,0.065));
#30872=CARTESIAN_POINT('',(0.029164849123336,-0.0093296645715295,0.065));
#30873=CARTESIAN_POINT('',(0.029164849123336,-0.0093296645715295,0.064));
#30874=CARTESIAN_POINT('',(0.029709488158351,-0.00849099400358408,0.065));
#30875=CARTESIAN_POINT('',(0.030254127193366,-0.00765232343563865,0.065));
#30876=CARTESIAN_POINT('',(0.030254127193366,-0.00765232343563865,0.064));
#30877=CARTESIAN_POINT('',(0.0217541700899211,-0.0223746810009612,0.066));
#30878=CARTESIAN_POINT('',(0.022748662330771,-0.0206394619419116,0.066));
#30879=CARTESIAN_POINT('',(0.022748662330771,-0.0206394619419116,0.067));
#30880=CARTESIAN_POINT('',(0.0217541700899211,-0.0223746810009612,0.067));
#30881=CARTESIAN_POINT('',(-0.00438968180222396,0.00675951720953923,0.066));
#30882=CARTESIAN_POINT('',(-0.0119400657566617,0.00185624053797081,0.066));
#30883=CARTESIAN_POINT('',(-0.0119400657566617,0.00185624053797081,0.067));
#30884=CARTESIAN_POINT('',(-0.0124847047916767,0.00269491110591624,0.066));
#30885=CARTESIAN_POINT('',(-0.00493432083723898,0.00759818777748466,0.066));
#30886=CARTESIAN_POINT('',(-0.00438968180222396,0.00675951720953923,0.067));
#30887=CARTESIAN_POINT('',(-0.0130293438266917,0.00353358167386167,0.064));
#30888=CARTESIAN_POINT('',(-0.0130293438266917,0.00353358167386167,0.066));
#30889=CARTESIAN_POINT('',(-0.0120642072469368,0.00327183488320525,0.066));
#30890=CARTESIAN_POINT('',(-0.0120642072469368,0.00327183488320525,0.064));
#30891=CARTESIAN_POINT('',(-0.0124847047916767,0.00269491110591624,0.064));
#30892=CARTESIAN_POINT('',(0.,0.,0.065));
#30893=CARTESIAN_POINT('',(-0.00815634808936724,0.00810703310990374,0.065));
#30894=CARTESIAN_POINT('',(-0.00886559574931222,0.00881199251076493,0.065));
#30895=CARTESIAN_POINT('',(-0.00815634808936724,0.00810703310990374,0.064));
#30896=CARTESIAN_POINT('',(0.,0.,0.064));
#30897=CARTESIAN_POINT('',(0.,0.,0.065));
#30898=CARTESIAN_POINT('',(0.00438968180222396,0.00675951720953923,0.065));
#30899=CARTESIAN_POINT('',(0.0119400657566616,0.00185624053797081,0.065));
#30900=CARTESIAN_POINT('',(0.0119400657566616,0.00185624053797081,0.064));
#30901=CARTESIAN_POINT('',(0.0124847047916767,0.00269491110591624,0.065));
#30902=CARTESIAN_POINT('',(0.00493432083723899,0.00759818777748466,0.065));
#30903=CARTESIAN_POINT('',(0.00438968180222396,0.00675951720953923,0.064));
#30904=CARTESIAN_POINT('',(0.030254127193366,-0.00765232343563865,0.064));
#30905=CARTESIAN_POINT('',(0.030254127193366,-0.00765232343563865,0.066));
#30906=CARTESIAN_POINT('',(0.029709488158351,-0.00849099400358408,0.066));
#30907=CARTESIAN_POINT('',(0.0297513783604445,-0.00851675597262234,0.066));
#30908=CARTESIAN_POINT('',(0.0297513783604445,-0.00851675597262234,0.064));
#30909=CARTESIAN_POINT('',(0.029709488158351,-0.00849099400358408,0.064));
#30910=CARTESIAN_POINT('',(0.0259807621135331,-0.015,0.066));
#30911=CARTESIAN_POINT('',(0.029248629527523,-0.00938118850960603,0.066));
#30912=CARTESIAN_POINT('',(0.029248629527523,-0.00938118850960603,0.067));
#30913=CARTESIAN_POINT('',(0.0259807621135331,-0.015,0.067));
#30914=CARTESIAN_POINT('',(0.0259807621135331,-0.015,0.066));
#30915=CARTESIAN_POINT('',(-0.0130293438266917,0.00353358167386167,0.066));
#30916=CARTESIAN_POINT('',(-0.0130293438266917,0.00353358167386167,0.067));
#30917=CARTESIAN_POINT('',(-0.0110990706671818,0.00301008809254883,0.067));
#30918=CARTESIAN_POINT('',(-0.0110990706671818,0.00301008809254883,0.066));
#30919=CARTESIAN_POINT('',(-0.0095748434092572,0.00951695191162613,0.065));
#30920=CARTESIAN_POINT('',(-0.00757758433974805,0.00941227999914025,0.065));
#30921=CARTESIAN_POINT('',(-0.00857621387450262,0.00946461595538319,0.065));
#30922=CARTESIAN_POINT('',(-0.00757758433974805,0.00941227999914025,0.064));
#30923=CARTESIAN_POINT('',(-0.0095748434092572,0.00951695191162613,0.064));
#30924=CARTESIAN_POINT('',(-0.0095748434092572,0.00951695191162613,0.065));
#30925=CARTESIAN_POINT('',(0.0130293438266917,0.00353358167386167,0.065));
#30926=CARTESIAN_POINT('',(0.0110990706671818,0.00301008809254883,0.065));
#30927=CARTESIAN_POINT('',(0.0110990706671818,0.00301008809254883,0.064));
#30928=CARTESIAN_POINT('',(0.0120642072469368,0.00327183488320525,0.065));
#30929=CARTESIAN_POINT('',(0.0130293438266917,0.00353358167386167,0.065));
#30930=CARTESIAN_POINT('',(0.0130293438266917,0.00353358167386167,0.064));
#30931=CARTESIAN_POINT('',(0.030254127193366,-0.00765232343563865,0.066));
#30932=CARTESIAN_POINT('',(0.029164849123336,-0.0093296645715295,0.066));
#30933=CARTESIAN_POINT('',(0.029164849123336,-0.0093296645715295,0.067));
#30934=CARTESIAN_POINT('',(0.030254127193366,-0.00765232343563865,0.067));
#30935=CARTESIAN_POINT('',(0.,0.,0.066));
#30936=CARTESIAN_POINT('',(-0.00815634808936724,0.00810703310990374,0.066));
#30937=CARTESIAN_POINT('',(-0.00815634808936724,0.00810703310990374,0.067));
#30938=CARTESIAN_POINT('',(-0.00886559574931222,0.00881199251076493,0.066));
#30939=CARTESIAN_POINT('',(0.,0.,0.066));
#30940=CARTESIAN_POINT('',(0.,0.,0.067));
#30941=CARTESIAN_POINT('',(-0.0095748434092572,0.00951695191162613,0.064));
#30942=CARTESIAN_POINT('',(-0.0095748434092572,0.00951695191162613,0.066));
#30943=CARTESIAN_POINT('',(-0.00857621387450262,0.00946461595538319,0.066));
#30944=CARTESIAN_POINT('',(-0.00857621387450262,0.00946461595538319,0.064));
#30945=CARTESIAN_POINT('',(-0.00886559574931222,0.00881199251076493,0.064));
#30946=CARTESIAN_POINT('',(-0.00804875452189106,0.000421817350486591,0.065));
#30947=CARTESIAN_POINT('',(-0.00650269803393578,0.029922332524114,0.065));
#30948=CARTESIAN_POINT('',(-0.00750132756869036,0.029974668480357,0.065));
#30949=CARTESIAN_POINT('',(-0.00650269803393578,0.029922332524114,0.064));
#30950=CARTESIAN_POINT('',(-0.00804875452189106,0.000421817350486591,0.064));
#30951=CARTESIAN_POINT('',(-0.00904738405664563,0.000474153306729528,0.065));
#30952=CARTESIAN_POINT('',(0.,0.,0.065));
#30953=CARTESIAN_POINT('',(0.00815634808936724,0.00810703310990373,0.065));
#30954=CARTESIAN_POINT('',(0.00815634808936724,0.00810703310990373,0.064));
#30955=CARTESIAN_POINT('',(0.00886559574931222,0.00881199251076493,0.065));
#30956=CARTESIAN_POINT('',(0.,0.,0.065));
#30957=CARTESIAN_POINT('',(0.,0.,0.064));
#30958=CARTESIAN_POINT('',(0.0130293438266917,0.00353358167386167,0.064));
#30959=CARTESIAN_POINT('',(0.0130293438266917,0.00353358167386167,0.066));
#30960=CARTESIAN_POINT('',(0.0120642072469368,0.00327183488320525,0.066));
#30961=CARTESIAN_POINT('',(0.0124847047916767,0.00269491110591624,0.066));
#30962=CARTESIAN_POINT('',(0.0124847047916767,0.00269491110591624,0.064));
#30963=CARTESIAN_POINT('',(0.0120642072469368,0.00327183488320525,0.064));
#30964=CARTESIAN_POINT('',(0.00438968180222396,0.00675951720953923,0.066));
#30965=CARTESIAN_POINT('',(0.0119400657566616,0.00185624053797081,0.066));
#30966=CARTESIAN_POINT('',(0.0119400657566616,0.00185624053797081,0.067));
#30967=CARTESIAN_POINT('',(0.011612482002865,0.00206897591509449,0.067));
#30968=CARTESIAN_POINT('',(0.0297307621135331,-0.00850480947161673,0.066));
#30969=CARTESIAN_POINT('',(-0.0095748434092572,0.00951695191162613,0.066));
#30970=CARTESIAN_POINT('',(-0.0095748434092572,0.00951695191162613,0.067));
#30971=CARTESIAN_POINT('',(-0.00757758433974805,0.00941227999914025,0.067));
#30972=CARTESIAN_POINT('',(-0.00757758433974805,0.00941227999914025,0.066));
#30973=CARTESIAN_POINT('',(-0.00849995710344493,0.0300270044365999,0.065));
#30974=CARTESIAN_POINT('',(-0.00649996719675201,0.0300206504515176,0.065));
#30975=CARTESIAN_POINT('',(-0.00749996215009847,0.0300238274440587,0.065));
#30976=CARTESIAN_POINT('',(-0.00649996719675201,0.0300206504515176,0.064));
#30977=CARTESIAN_POINT('',(-0.00849995710344493,0.0300270044365999,0.064));
#30978=CARTESIAN_POINT('',(-0.00849995710344493,0.0300270044365999,0.065));
#30979=CARTESIAN_POINT('',(0.0095748434092572,0.00951695191162612,0.065));
#30980=CARTESIAN_POINT('',(0.00757758433974805,0.00941227999914025,0.065));
#30981=CARTESIAN_POINT('',(0.00757758433974805,0.00941227999914025,0.064));
#30982=CARTESIAN_POINT('',(0.00857621387450262,0.00946461595538318,0.065));
#30983=CARTESIAN_POINT('',(0.0095748434092572,0.00951695191162612,0.065));
#30984=CARTESIAN_POINT('',(0.0095748434092572,0.00951695191162612,0.064));
#30985=CARTESIAN_POINT('',(0.0130293438266917,0.00353358167386167,0.066));
#30986=CARTESIAN_POINT('',(0.0110990706671818,0.00301008809254883,0.066));
#30987=CARTESIAN_POINT('',(0.0110990706671818,0.00301008809254883,0.067));
#30988=CARTESIAN_POINT('',(0.0130293438266917,0.00353358167386167,0.067));
#30989=CARTESIAN_POINT('',(-0.00804875452189106,0.000421817350486591,0.066));
#30990=CARTESIAN_POINT('',(-0.00650269803393578,0.029922332524114,0.066));
#30991=CARTESIAN_POINT('',(-0.00650269803393578,0.029922332524114,0.067));
#30992=CARTESIAN_POINT('',(-0.00750132756869036,0.029974668480357,0.066));
#30993=CARTESIAN_POINT('',(-0.0075,0.03,0.066));
#30994=CARTESIAN_POINT('',(-0.0075980267037225,0.00902221645792347,0.067));
#30995=CARTESIAN_POINT('',(-0.00849995710344493,0.0300270044365999,0.064));
#30996=CARTESIAN_POINT('',(-0.00849995710344493,0.0300270044365999,0.066));
#30997=CARTESIAN_POINT('',(-0.00749996215009847,0.0300238274440587,0.066));
#30998=CARTESIAN_POINT('',(-0.00749996215009847,0.0300238274440587,0.064));
#30999=CARTESIAN_POINT('',(-0.00750132756869036,0.029974668480357,0.064));
#31000=CARTESIAN_POINT('',(0.,0.03,0.065));
#31001=CARTESIAN_POINT('',(0.00649996719675201,0.0300206504515176,0.065));
#31002=CARTESIAN_POINT('',(0.00749996215009847,0.0300238274440587,0.065));
#31003=CARTESIAN_POINT('',(0.00649996719675201,0.0300206504515176,0.064));
#31004=CARTESIAN_POINT('',(0.,0.03,0.064));
#31005=CARTESIAN_POINT('',(0.,0.03,0.065));
#31006=CARTESIAN_POINT('',(0.00804875452189106,0.000421817350486591,0.065));
#31007=CARTESIAN_POINT('',(0.00650269803393578,0.029922332524114,0.065));
#31008=CARTESIAN_POINT('',(0.00650269803393578,0.029922332524114,0.064));
#31009=CARTESIAN_POINT('',(0.00750132756869036,0.029974668480357,0.065));
#31010=CARTESIAN_POINT('',(0.0075,0.03,0.065));
#31011=CARTESIAN_POINT('',(0.0075980267037225,0.00902221645792347,0.064));
#31012=CARTESIAN_POINT('',(0.0095748434092572,0.00951695191162612,0.064));
#31013=CARTESIAN_POINT('',(0.0095748434092572,0.00951695191162612,0.066));
#31014=CARTESIAN_POINT('',(0.00857621387450262,0.00946461595538318,0.066));
#31015=CARTESIAN_POINT('',(0.00886559574931222,0.00881199251076493,0.066));
#31016=CARTESIAN_POINT('',(0.00886559574931222,0.00881199251076493,0.064));
#31017=CARTESIAN_POINT('',(0.00857621387450262,0.00946461595538318,0.064));
#31018=CARTESIAN_POINT('',(0.,0.,0.066));
#31019=CARTESIAN_POINT('',(0.00815634808936724,0.00810703310990373,0.066));
#31020=CARTESIAN_POINT('',(0.00815634808936724,0.00810703310990373,0.067));
#31021=CARTESIAN_POINT('',(0.,0.,0.067));
#31022=CARTESIAN_POINT('',(0.,0.,0.066));
#31023=CARTESIAN_POINT('',(-0.00849995710344493,0.0300270044365999,0.066));
#31024=CARTESIAN_POINT('',(-0.00849995710344493,0.0300270044365999,0.067));
#31025=CARTESIAN_POINT('',(-0.00649996719675201,0.0300206504515176,0.067));
#31026=CARTESIAN_POINT('',(-0.00649996719675201,0.0300206504515176,0.066));
#31027=CARTESIAN_POINT('',(0.00849995710344493,0.0300270044365999,0.065));
#31028=CARTESIAN_POINT('',(0.00849995710344493,0.0300270044365999,0.065));
#31029=CARTESIAN_POINT('',(0.00849995710344493,0.0300270044365999,0.064));
#31030=CARTESIAN_POINT('',(0.0095748434092572,0.00951695191162612,0.066));
#31031=CARTESIAN_POINT('',(0.00757758433974805,0.00941227999914025,0.066));
#31032=CARTESIAN_POINT('',(0.00757758433974805,0.00941227999914025,0.067));
#31033=CARTESIAN_POINT('',(0.0095748434092572,0.00951695191162612,0.067));
#31034=CARTESIAN_POINT('',(0.,0.03,0.066));
#31035=CARTESIAN_POINT('',(0.00649996719675201,0.0300206504515176,0.066));
#31036=CARTESIAN_POINT('',(0.00649996719675201,0.0300206504515176,0.067));
#31037=CARTESIAN_POINT('',(0.00749996215009847,0.0300238274440587,0.066));
#31038=CARTESIAN_POINT('',(0.,0.03,0.066));
#31039=CARTESIAN_POINT('',(0.,0.03,0.067));
#31040=CARTESIAN_POINT('',(0.00849995710344493,0.0300270044365999,0.064));
#31041=CARTESIAN_POINT('',(0.00849995710344493,0.0300270044365999,0.066));
#31042=CARTESIAN_POINT('',(0.00750132756869036,0.029974668480357,0.066));
#31043=CARTESIAN_POINT('',(0.00750132756869036,0.029974668480357,0.067));
#31044=CARTESIAN_POINT('',(0.00749996215009847,0.0300238274440587,0.064));
#31045=CARTESIAN_POINT('',(0.00804875452189106,0.000421817350486591,0.066));
#31046=CARTESIAN_POINT('',(0.00650269803393578,0.029922332524114,0.066));
#31047=CARTESIAN_POINT('',(0.00650269803393578,0.029922332524114,0.067));
#31048=CARTESIAN_POINT('',(0.00804875452189106,0.000421817350486591,0.067));
#31049=CARTESIAN_POINT('',(0.00904738405664563,0.000474153306729528,0.066));
#31050=CARTESIAN_POINT('',(0.00849995710344493,0.0300270044365999,0.066));
#31051=CARTESIAN_POINT('',(0.00849995710344493,0.0300270044365999,0.067));
#31052=CARTESIAN_POINT('',(-0.024761562113538,-0.0149999999999972,0.066269998));
#31053=CARTESIAN_POINT('',(0.,0.03,0.066269998));
#31054=CARTESIAN_POINT('',(-0.00277876,0.03,0.066269998));
#31055=CARTESIAN_POINT('',(0.,0.03,0.066269998));
#31056=CARTESIAN_POINT('',(-0.0012192,0.03,0.066269998));
#31057=CARTESIAN_POINT('',(-0.024761562113538,-0.0149999999999972,0.066269998));
#31058=CARTESIAN_POINT('',(0.0259807621135283,-0.0150000000000028,0.066269998));
#31059=CARTESIAN_POINT('',(0.0232020021135283,-0.0150000000000028,0.066269998));
#31060=CARTESIAN_POINT('',(0.0259807621135283,-0.0150000000000028,0.066269998));
#31061=CARTESIAN_POINT('',(0.0247615621135283,-0.0150000000000028,0.066269998));
#31062=CARTESIAN_POINT('',(-0.024761562113538,-0.0149999999999972,0.066269998));
#31063=CARTESIAN_POINT('',(-0.025980762113538,-0.0149999999999972,0.066269998));
#31064=CARTESIAN_POINT('',(-0.028759522113538,-0.0149999999999972,0.066269998));
#31065=CARTESIAN_POINT('',(-0.025980762113538,-0.0149999999999972,0.066269998));
#31066=CARTESIAN_POINT('',(-0.027199962113538,-0.0149999999999972,0.066269998));
#31067=CARTESIAN_POINT('',(-0.00753201094464286,0.,0.0662062500024776));
#31068=CARTESIAN_POINT('',(-0.00753201094464286,0.00244729870815628,0.0661155357167633));
#31069=CARTESIAN_POINT('',(-0.00609352485603417,0.00442720495336657,0.066024821431049));
#31070=CARTESIAN_POINT('',(-0.00465503876742549,0.00640711119857685,0.0659341071453347));
#31071=CARTESIAN_POINT('',(-0.00232751938371274,0.00716336808970901,0.0658433928596205));
#31072=CARTESIAN_POINT('',(-4.84937169161726E-19,0.00791962498084115,0.0657526785739062));
#31073=CARTESIAN_POINT('',(0.00232751938371274,0.00716336808970901,0.0656619642881919));
#31074=CARTESIAN_POINT('',(0.00465503876742549,0.00640711119857685,0.0655712500024775));
#31075=CARTESIAN_POINT('',(0.00609352485603417,0.00442720495336657,0.0654805357167633));
#31076=CARTESIAN_POINT('',(0.00753201094464286,0.00244729870815628,0.065389821431049));
#31077=CARTESIAN_POINT('',(0.00753201094464286,9.22405309449971E-19,0.0652991071453347));
#31078=CARTESIAN_POINT('',(0.00753201094464286,-0.00244729870815628,0.0652083928596204));
#31079=CARTESIAN_POINT('',(0.00609352485603417,-0.00442720495336657,0.0651176785739062));
#31080=CARTESIAN_POINT('',(0.00465503876742549,-0.00640711119857685,0.0650269642881918));
#31081=CARTESIAN_POINT('',(0.00232751938371274,-0.00716336808970901,0.0649362500024776));
#31082=CARTESIAN_POINT('',(1.45481150748518E-18,-0.00791962498084115,0.0648455357167633));
#31083=CARTESIAN_POINT('',(-0.00232751938371274,-0.00716336808970901,0.064754821431049));
#31084=CARTESIAN_POINT('',(-0.00465503876742549,-0.00640711119857685,0.0646641071453347));
#31085=CARTESIAN_POINT('',(-0.00609352485603417,-0.00442720495336658,0.0645733928596205));
#31086=CARTESIAN_POINT('',(-0.00753201094464286,-0.00244729870815628,0.0644826785739061));
#31087=CARTESIAN_POINT('',(-0.00753201094464286,0.,0.0643919642881919));
#31088=CARTESIAN_POINT('',(-0.00753201094464286,0.00244729870815628,0.0643012500024776));
#31089=CARTESIAN_POINT('',(-0.00609352485603417,0.00442720495336657,0.0642105357167633));
#31090=CARTESIAN_POINT('',(-0.00465503876742549,0.00640711119857685,0.064119821431049));
#31091=CARTESIAN_POINT('',(-0.00232751938371274,0.00716336808970901,0.0640291071453348));
#31092=CARTESIAN_POINT('',(-4.84937169161726E-19,0.00791962498084115,0.0639383928596205));
#31093=CARTESIAN_POINT('',(0.00232751938371274,0.00716336808970901,0.0638476785739062));
#31094=CARTESIAN_POINT('',(0.00465503876742549,0.00640711119857685,0.0637569642881919));
#31095=CARTESIAN_POINT('',(0.00609352485603417,0.00442720495336657,0.0636662500024776));
#31096=CARTESIAN_POINT('',(0.00753201094464286,0.00244729870815628,0.0635755357167633));
#31097=CARTESIAN_POINT('',(0.00753201094464286,9.22405309449971E-19,0.063484821431049));
#31098=CARTESIAN_POINT('',(0.00753201094464286,-0.00244729870815628,0.0633941071453348));
#31099=CARTESIAN_POINT('',(0.00609352485603417,-0.00442720495336657,0.0633033928596205));
#31100=CARTESIAN_POINT('',(0.00534171614397317,-0.00546198087230006,0.0632559820498473));
#31101=CARTESIAN_POINT('',(0.0042904607332246,-0.00619056827495487,0.0632061437275364));
#31102=CARTESIAN_POINT('',(-0.00655,0.,0.0656392857192409));
#31103=CARTESIAN_POINT('',(-0.00655,0.00212822401032553,0.0655485714335265));
#31104=CARTESIAN_POINT('',(-0.00529906131315591,0.0038499934025157,0.0654578571478123));
#31105=CARTESIAN_POINT('',(-0.00404812262631181,0.00557176279470586,0.065367142862098));
#31106=CARTESIAN_POINT('',(-0.0020240613131559,0.00622942018173326,0.0652764285763837));
#31107=CARTESIAN_POINT('',(-4.21711875003113E-19,0.00688707756876065,0.0651857142906694));
#31108=CARTESIAN_POINT('',(0.0020240613131559,0.00622942018173326,0.0650950000049552));
#31109=CARTESIAN_POINT('',(0.00404812262631181,0.00557176279470586,0.0650042857192408));
#31110=CARTESIAN_POINT('',(0.00529906131315591,0.0038499934025157,0.0649135714335266));
#31111=CARTESIAN_POINT('',(0.00655,0.00212822401032553,0.0648228571478123));
#31112=CARTESIAN_POINT('',(0.00655,8.02143653441516E-19,0.064732142862098));
#31113=CARTESIAN_POINT('',(0.00655,-0.00212822401032553,0.0646414285763837));
#31114=CARTESIAN_POINT('',(0.00529906131315591,-0.0038499934025157,0.0645507142906695));
#31115=CARTESIAN_POINT('',(0.00404812262631181,-0.00557176279470586,0.0644600000049551));
#31116=CARTESIAN_POINT('',(0.0020240613131559,-0.00622942018173326,0.0643692857192409));
#31117=CARTESIAN_POINT('',(1.26513562500934E-18,-0.00688707756876065,0.0642785714335266));
#31118=CARTESIAN_POINT('',(-0.0020240613131559,-0.00622942018173326,0.0641878571478123));
#31119=CARTESIAN_POINT('',(-0.00404812262631181,-0.00557176279470586,0.064097142862098));
#31120=CARTESIAN_POINT('',(-0.00529906131315591,-0.0038499934025157,0.0640064285763837));
#31121=CARTESIAN_POINT('',(-0.00655,-0.00212822401032553,0.0639157142906694));
#31122=CARTESIAN_POINT('',(-0.00655,0.,0.0638250000049552));
#31123=CARTESIAN_POINT('',(-0.00655,0.00212822401032553,0.0637342857192409));
#31124=CARTESIAN_POINT('',(-0.00529906131315591,0.0038499934025157,0.0636435714335266));
#31125=CARTESIAN_POINT('',(-0.00404812262631181,0.00557176279470586,0.0635528571478123));
#31126=CARTESIAN_POINT('',(-0.0020240613131559,0.00622942018173326,0.063462142862098));
#31127=CARTESIAN_POINT('',(-4.21711875003113E-19,0.00688707756876065,0.0633714285763838));
#31128=CARTESIAN_POINT('',(0.0020240613131559,0.00622942018173326,0.0632807142906695));
#31129=CARTESIAN_POINT('',(0.00404812262631181,0.00557176279470586,0.0631900000049551));
#31130=CARTESIAN_POINT('',(0.00529906131315591,0.0038499934025157,0.0630992857192409));
#31131=CARTESIAN_POINT('',(0.00655,0.00212822401032553,0.0630085714335265));
#31132=CARTESIAN_POINT('',(0.00655,8.02143653441516E-19,0.0629178571478123));
#31133=CARTESIAN_POINT('',(0.00655,-0.00212822401032553,0.062827142862098));
#31134=CARTESIAN_POINT('',(0.00529906131315591,-0.0038499934025157,0.0627364285763837));
#31135=CARTESIAN_POINT('',(0.00464527215907854,-0.00474985697398794,0.0626890177666106));
#31136=CARTESIAN_POINT('',(0.00373107766427357,-0.00538345237400303,0.0626391794442997));
#31137=CARTESIAN_POINT('',(-0.00704100547232143,0.,0.0659227678608592));
#31138=CARTESIAN_POINT('',(-0.00753201094464286,0.,0.0662062500024776));
#31139=CARTESIAN_POINT('',(-0.00655,0.,0.0656392857192409));
#31140=CARTESIAN_POINT('',(-0.00655,0.,0.0656392857192409));
#31141=CARTESIAN_POINT('',(-0.00655,0.00212822401032553,0.0655485714335265));
#31142=CARTESIAN_POINT('',(-0.00529906131315591,0.0038499934025157,0.0654578571478123));
#31143=CARTESIAN_POINT('',(-0.00404812262631181,0.00557176279470586,0.065367142862098));
#31144=CARTESIAN_POINT('',(-0.0020240613131559,0.00622942018173326,0.0652764285763837));
#31145=CARTESIAN_POINT('',(-4.21711875003113E-19,0.00688707756876065,0.0651857142906694));
#31146=CARTESIAN_POINT('',(0.0020240613131559,0.00622942018173326,0.0650950000049552));
#31147=CARTESIAN_POINT('',(0.00404812262631181,0.00557176279470586,0.0650042857192408));
#31148=CARTESIAN_POINT('',(0.00529906131315591,0.0038499934025157,0.0649135714335266));
#31149=CARTESIAN_POINT('',(0.00654999999999999,0.00212822401032555,0.0648228571478123));
#31150=CARTESIAN_POINT('',(0.00655,8.02143653441516E-19,0.064732142862098));
#31151=CARTESIAN_POINT('',(0.00655,8.02143653441516E-19,0.064732142862098));
#31152=CARTESIAN_POINT('',(0.00655,8.02143653441517E-19,0.064732142862098));
#31153=CARTESIAN_POINT('',(0.00655000000000001,-0.00212822401032553,0.0646414285763838));
#31154=CARTESIAN_POINT('',(0.00529906131315591,-0.0038499934025157,0.0645507142906695));
#31155=CARTESIAN_POINT('',(0.00404812262631181,-0.00557176279470586,0.0644600000049551));
#31156=CARTESIAN_POINT('',(0.0020240613131559,-0.00622942018173326,0.0643692857192409));
#31157=CARTESIAN_POINT('',(1.26513562500934E-18,-0.00688707756876065,0.0642785714335266));
#31158=CARTESIAN_POINT('',(-0.0020240613131559,-0.00622942018173326,0.0641878571478123));
#31159=CARTESIAN_POINT('',(-0.00404812262631181,-0.00557176279470586,0.064097142862098));
#31160=CARTESIAN_POINT('',(-0.00529906131315591,-0.0038499934025157,0.0640064285763837));
#31161=CARTESIAN_POINT('',(-0.00654999999999999,-0.00212822401032555,0.0639157142906695));
#31162=CARTESIAN_POINT('',(-0.00655,0.,0.0638250000049552));
#31163=CARTESIAN_POINT('',(-0.00655,0.,0.0638250000049552));
#31164=CARTESIAN_POINT('',(-0.00655,0.,0.0638250000049552));
#31165=CARTESIAN_POINT('',(-0.00655000000000001,0.00212822401032553,0.0637342857192409));
#31166=CARTESIAN_POINT('',(-0.00529906131315591,0.0038499934025157,0.0636435714335266));
#31167=CARTESIAN_POINT('',(-0.00404812262631181,0.00557176279470586,0.0635528571478123));
#31168=CARTESIAN_POINT('',(-0.0020240613131559,0.00622942018173326,0.063462142862098));
#31169=CARTESIAN_POINT('',(-4.21711875003113E-19,0.00688707756876065,0.0633714285763838));
#31170=CARTESIAN_POINT('',(0.0020240613131559,0.00622942018173326,0.0632807142906695));
#31171=CARTESIAN_POINT('',(0.00404812262631181,0.00557176279470586,0.0631900000049551));
#31172=CARTESIAN_POINT('',(0.00529906131315591,0.0038499934025157,0.0630992857192409));
#31173=CARTESIAN_POINT('',(0.00654999999999999,0.00212822401032556,0.0630085714335266));
#31174=CARTESIAN_POINT('',(0.00655,8.02143653441516E-19,0.0629178571478123));
#31175=CARTESIAN_POINT('',(0.00655,8.02143653441516E-19,0.0629178571478123));
#31176=CARTESIAN_POINT('',(0.00655,8.02143653441517E-19,0.0629178571478123));
#31177=CARTESIAN_POINT('',(0.00655000000000002,-0.00212822401032552,0.062827142862098));
#31178=CARTESIAN_POINT('',(0.00529906131315591,-0.0038499934025157,0.0627364285763837));
#31179=CARTESIAN_POINT('',(0.00464527215907854,-0.00474985697398794,0.0626890177666106));
#31180=CARTESIAN_POINT('',(0.00373107766427357,-0.00538345237400303,0.0626391794442997));
#31181=CARTESIAN_POINT('',(0.00373107766427358,-0.00538345237400303,0.0626391794442997));
#31182=CARTESIAN_POINT('',(0.00401076919874908,-0.00578701032447895,0.0629226615859181));
#31183=CARTESIAN_POINT('',(0.0042904607332246,-0.00619056827495487,0.0632061437275364));
#31184=CARTESIAN_POINT('',(-0.00753201094464286,0.,0.0662062500024776));
#31185=CARTESIAN_POINT('',(-0.00753201094464286,0.00244729870815628,0.0661155357167633));
#31186=CARTESIAN_POINT('',(-0.00609352485603417,0.00442720495336657,0.066024821431049));
#31187=CARTESIAN_POINT('',(-0.00465503876742549,0.00640711119857685,0.0659341071453347));
#31188=CARTESIAN_POINT('',(-0.00232751938371274,0.00716336808970901,0.0658433928596205));
#31189=CARTESIAN_POINT('',(-4.84937169161726E-19,0.00791962498084115,0.0657526785739062));
#31190=CARTESIAN_POINT('',(0.00232751938371274,0.00716336808970901,0.0656619642881919));
#31191=CARTESIAN_POINT('',(0.00465503876742549,0.00640711119857685,0.0655712500024775));
#31192=CARTESIAN_POINT('',(0.00609352485603417,0.00442720495336657,0.0654805357167633));
#31193=CARTESIAN_POINT('',(0.00753201094464286,0.00244729870815628,0.065389821431049));
#31194=CARTESIAN_POINT('',(0.00753201094464286,9.22405309449971E-19,0.0652991071453347));
#31195=CARTESIAN_POINT('',(0.00753201094464286,-0.00244729870815628,0.0652083928596204));
#31196=CARTESIAN_POINT('',(0.00609352485603417,-0.00442720495336657,0.0651176785739062));
#31197=CARTESIAN_POINT('',(0.00465503876742549,-0.00640711119857685,0.0650269642881918));
#31198=CARTESIAN_POINT('',(0.00232751938371274,-0.00716336808970901,0.0649362500024776));
#31199=CARTESIAN_POINT('',(1.45481150748518E-18,-0.00791962498084115,0.0648455357167633));
#31200=CARTESIAN_POINT('',(-0.00232751938371274,-0.00716336808970901,0.064754821431049));
#31201=CARTESIAN_POINT('',(-0.00465503876742549,-0.00640711119857685,0.0646641071453347));
#31202=CARTESIAN_POINT('',(-0.00609352485603417,-0.00442720495336658,0.0645733928596205));
#31203=CARTESIAN_POINT('',(-0.00753201094464286,-0.00244729870815628,0.0644826785739061));
#31204=CARTESIAN_POINT('',(-0.00753201094464286,0.,0.0643919642881919));
#31205=CARTESIAN_POINT('',(-0.00753201094464286,0.00244729870815628,0.0643012500024776));
#31206=CARTESIAN_POINT('',(-0.00609352485603417,0.00442720495336657,0.0642105357167633));
#31207=CARTESIAN_POINT('',(-0.00465503876742549,0.00640711119857685,0.064119821431049));
#31208=CARTESIAN_POINT('',(-0.00232751938371274,0.00716336808970901,0.0640291071453348));
#31209=CARTESIAN_POINT('',(-4.84937169161726E-19,0.00791962498084115,0.0639383928596205));
#31210=CARTESIAN_POINT('',(0.00232751938371274,0.00716336808970901,0.0638476785739062));
#31211=CARTESIAN_POINT('',(0.00465503876742549,0.00640711119857685,0.0637569642881919));
#31212=CARTESIAN_POINT('',(0.00609352485603417,0.00442720495336657,0.0636662500024776));
#31213=CARTESIAN_POINT('',(0.00753201094464286,0.00244729870815628,0.0635755357167633));
#31214=CARTESIAN_POINT('',(0.00753201094464286,9.22405309449971E-19,0.063484821431049));
#31215=CARTESIAN_POINT('',(0.00753201094464286,-0.00244729870815628,0.0633941071453348));
#31216=CARTESIAN_POINT('',(0.00609352485603417,-0.00442720495336657,0.0633033928596205));
#31217=CARTESIAN_POINT('',(0.00534171614397317,-0.00546198087230006,0.0632559820498473));
#31218=CARTESIAN_POINT('',(0.0042904607332246,-0.00619056827495487,0.0632061437275364));
#31219=CARTESIAN_POINT('',(-0.00655,0.,0.067));
#31220=CARTESIAN_POINT('',(-0.00655,0.000701436451549039,0.0669701016874316));
#31221=CARTESIAN_POINT('',(-0.00643426444377327,0.00142116428632275,0.0669378208348473));
#31222=CARTESIAN_POINT('',(-0.00597275524955853,0.00278310287089703,0.0668733773348871));
#31223=CARTESIAN_POINT('',(-0.00563065184170616,0.00341964341195903,0.0668419312518172));
#31224=CARTESIAN_POINT('',(-0.00477526447734829,0.00453817699069122,0.0667814502995436));
#31225=CARTESIAN_POINT('',(-0.00424468348110516,0.00504002014029157,0.0667489920151821));
#31226=CARTESIAN_POINT('',(-0.00305067784563627,0.00584059119879621,0.0666846094693261));
#31227=CARTESIAN_POINT('',(-0.00239715639327556,0.00613638840539808,0.0666538642150764));
#31228=CARTESIAN_POINT('',(-0.00103349869292125,0.00650642005156875,0.0665927478677392));
#31229=CARTESIAN_POINT('',(-0.000306008953235865,0.00658216137226912,0.0665601432664502));
#31230=CARTESIAN_POINT('',(0.00112780996837254,0.00649203623567304,0.0664958824367649));
#31231=CARTESIAN_POINT('',(0.00182250228407492,0.00633113339858685,0.0664657019759955));
#31232=CARTESIAN_POINT('',(0.00313452003775661,0.00579478634800822,0.0664040010301873));
#31233=CARTESIAN_POINT('',(0.00375876413031788,0.00541195045606427,0.0663712817114677));
#31234=CARTESIAN_POINT('',(0.00484143708566559,0.00446967587994929,0.0663072029772139));
#31235=CARTESIAN_POINT('',(0.00529358804533871,0.00392244160944412,0.0662774495781941));
#31236=CARTESIAN_POINT('',(0.00601170596849487,0.00269573995808473,0.0662152165673029));
#31237=CARTESIAN_POINT('',(0.00627453396340782,0.00201157756744779,0.06618241451258));
#31238=CARTESIAN_POINT('',(0.00656107801575611,0.000607022272226752,0.0661185776819682));
#31239=CARTESIAN_POINT('',(0.0065878793671143,-0.000100163932046034,0.0660891123253293));
#31240=CARTESIAN_POINT('',(0.00641225008508753,-0.00151434349314421,0.0660264013812344));
#31241=CARTESIAN_POINT('',(0.00620457950132945,-0.00221761186551469,0.0659935488484532));
#31242=CARTESIAN_POINT('',(0.00557935079068769,-0.00350506118760313,0.0659300129741499));
#31243=CARTESIAN_POINT('',(0.00517180671586844,-0.00408226252975466,0.0659006957696452));
#31244=CARTESIAN_POINT('',(0.00417062794027762,-0.00510081509681702,0.065837562474521));
#31245=CARTESIAN_POINT('',(0.00357788920975624,-0.0055327564608861,0.0658046918907707));
#31246=CARTESIAN_POINT('',(0.00230128976425064,-0.00617387647055902,0.0657415150903395));
#31247=CARTESIAN_POINT('',(0.00162702620582906,-0.00638491943224267,0.0657122056990415));
#31248=CARTESIAN_POINT('',(0.000210210709061308,-0.00658560717690332,0.0656487069280592));
#31249=CARTESIAN_POINT('',(-0.000522891642424388,-0.00656787931369974,0.0656158507809958));
#31250=CARTESIAN_POINT('',(-0.00192323933262137,-0.00630171443485821,0.0655530900634018));
#31251=CARTESIAN_POINT('',(-0.00258802439270498,-0.00605955334672256,0.0655236481227066));
#31252=CARTESIAN_POINT('',(-0.00383705340244455,-0.00535659203279485,0.0654598418785206));
#31253=CARTESIAN_POINT('',(-0.00440786581130166,-0.00489679911834568,0.0654270326073568));
#31254=CARTESIAN_POINT('',(-0.0053558302752271,-0.00383705677294902,0.0653647437065981));
#31255=CARTESIAN_POINT('',(-0.00573802192101622,-0.00323921158083279,0.0653350292553776));
#31256=CARTESIAN_POINT('',(-0.00630322602799729,-0.00192008564169453,0.0652709744953718));
#31257=CARTESIAN_POINT('',(-0.0064764665607443,-0.00120850232220196,0.0652382443822136));
#31258=CARTESIAN_POINT('',(-0.0065850576225975,0.000205214722369539,0.0651764815990629));
#31259=CARTESIAN_POINT('',(-0.00652537124758188,0.000915383751165133,0.0651463555003048));
#31260=CARTESIAN_POINT('',(-0.00599520854117729,0.00300392474447296,0.0650499901863294));
#31261=CARTESIAN_POINT('',(-0.00518902617595735,0.00424768704264818,0.064989819431178));
#31262=CARTESIAN_POINT('',(-0.00293340872055775,0.00603025299180784,0.0648610754305156));
#31263=CARTESIAN_POINT('',(-0.00153837411298647,0.0065271503636305,0.0648010896365284));
#31264=CARTESIAN_POINT('',(0.0013372471140284,0.00657130557324581,0.0646722101782343));
#31265=CARTESIAN_POINT('',(0.00274646451239923,0.00611779082991373,0.0646122946360618));
#31266=CARTESIAN_POINT('',(0.00505663061694785,0.00440464740475223,0.0644834016045714));
#31267=CARTESIAN_POINT('',(0.0058999096091617,0.00318752875836041,0.0644234413835539));
#31268=CARTESIAN_POINT('',(0.00669251592029745,0.000423678696913489,0.0642946567060896));
#31269=CARTESIAN_POINT('',(0.00662198505842965,-0.00105646913312049,0.0642345370163344));
#31270=CARTESIAN_POINT('',(0.00583433321739773,-0.00306253721515266,0.0641381209631122));
#31271=CARTESIAN_POINT('',(0.00546807180147761,-0.00367486321330173,0.0641078844342977));
#31272=CARTESIAN_POINT('',(0.00478388959737474,-0.0044880265747629,0.0640616555909692));
#31273=CARTESIAN_POINT('',(0.00453140912573415,-0.00474317143712696,0.0640457796654875));
#31274=CARTESIAN_POINT('',(0.00398596617037514,-0.00520993451354128,0.0640137066350069));
#31275=CARTESIAN_POINT('',(0.00368819903290208,-0.00541317002599699,0.0639975561488288));
#31276=CARTESIAN_POINT('',(0.00339274889905633,-0.00561793598932939,0.0639814493565187));
#31277=CARTESIAN_POINT('',(-0.00687733698154762,0.,0.0668110119055878));
#31278=CARTESIAN_POINT('',(-0.00687733698154762,0.000736490816556296,0.0667811135930194));
#31279=CARTESIAN_POINT('',(-0.00675581752797234,0.00149218713025683,0.066748832740435));
#31280=CARTESIAN_POINT('',(-0.0062712443602323,0.00292218874770557,0.0666843892404749));
#31281=CARTESIAN_POINT('',(-0.00591204429636411,0.00359054047340023,0.0666529431574049));
#31282=CARTESIAN_POINT('',(-0.00501390885293711,0.00476497289265484,0.0665924622051313));
#31283=CARTESIAN_POINT('',(-0.00445681201214791,0.00529189570970565,0.0665600039207699));
#31284=CARTESIAN_POINT('',(-0.00320313581169196,0.00613247539627217,0.0664956213749138));
#31285=CARTESIAN_POINT('',(-0.00251695455175989,0.00644305510131057,0.0664648761206642));
#31286=CARTESIAN_POINT('',(-0.00108514790552801,0.00683157912032622,0.066403759773327));
#31287=CARTESIAN_POINT('',(-0.000321301784850946,0.00691110562198788,0.0663711551720379));
#31288=CARTESIAN_POINT('',(0.00118417239750328,0.00681647647162464,0.0663068943423526));
#31289=CARTESIAN_POINT('',(0.00191358203927076,0.00664753249728436,0.0662767138815832));
#31290=CARTESIAN_POINT('',(0.00329116802672757,0.00608438144295026,0.0662150129357751));
#31291=CARTESIAN_POINT('',(0.00394660878753432,0.00568241328454874,0.0661822936170555));
#31292=CARTESIAN_POINT('',(0.00508338844474566,0.00469304843125292,0.0661182148828016));
#31293=CARTESIAN_POINT('',(0.00555813569912768,0.00411846606696049,0.0660884614837819));
#31294=CARTESIAN_POINT('',(0.00631214164569776,0.0028304598635682,0.0660262284728907));
#31295=CARTESIAN_POINT('',(0.00658810449901086,0.00211210638104738,0.0659934264181678));
#31296=CARTESIAN_POINT('',(0.0068889686223784,0.000637358278077574,0.065929589587556));
#31297=CARTESIAN_POINT('',(0.00691710937426408,-0.00010516963573701,0.0659001242309171));
#31298=CARTESIAN_POINT('',(0.00673270299925258,-0.00159002297834605,0.0658374132868221));
#31299=CARTESIAN_POINT('',(0.00651465405487715,-0.00232843726617145,0.065804560754041));
#31300=CARTESIAN_POINT('',(0.00585817946959136,-0.00368022701192217,0.0657410248797377));
#31301=CARTESIAN_POINT('',(0.00543026833411577,-0.00428627405561341,0.0657117076752329));
#31302=CARTESIAN_POINT('',(0.0043790555373965,-0.00535572890097344,0.0656485743801088));
#31303=CARTESIAN_POINT('',(0.0037566946226163,-0.00580925658295397,0.0656157037963585));
#31304=CARTESIAN_POINT('',(0.00241629697724243,-0.00648241663671485,0.0655525269959273));
#31305=CARTESIAN_POINT('',(0.00170833702218249,-0.00670400649397932,0.0655232176046293));
#31306=CARTESIAN_POINT('',(0.000220716012724379,-0.00691472363109353,0.065459718833647));
#31307=CARTESIAN_POINT('',(-0.000549023210654567,-0.00689610981594638,0.0654268626865835));
#31308=CARTESIAN_POINT('',(-0.0020193534330693,-0.00661664331755768,0.0653641019689896));
#31309=CARTESIAN_POINT('',(-0.00271736120077821,-0.00636238020199629,0.0653346600282944));
#31310=CARTESIAN_POINT('',(-0.00402881057477939,-0.00562428831789364,0.0652708537841083));
#31311=CARTESIAN_POINT('',(-0.00462814939752127,-0.00514151720119214,0.0652380445129446));
#31312=CARTESIAN_POINT('',(-0.00562348849140636,-0.0040288141137252,0.0651757556121858));
#31313=CARTESIAN_POINT('',(-0.00602478020737951,-0.00340109154136163,0.0651460411609653));
#31314=CARTESIAN_POINT('',(-0.00661823045273271,-0.00201604213608617,0.0650819864009596));
#31315=CARTESIAN_POINT('',(-0.00680012870045241,-0.00126889736072759,0.0650492562878014));
#31316=CARTESIAN_POINT('',(-0.00691414661274989,0.000215470351039704,0.0649874935046507));
#31317=CARTESIAN_POINT('',(-0.00685147740447671,0.000961130156365764,0.0649573674058926));
#31318=CARTESIAN_POINT('',(-0.00629481975760744,0.00315404621907631,0.0648610020919172));
#31319=CARTESIAN_POINT('',(-0.00544834833864581,0.00445996567701449,0.0648008313367658));
#31320=CARTESIAN_POINT('',(-0.00308000614899025,0.00633161555857225,0.0646720873361034));
#31321=CARTESIAN_POINT('',(-0.00161525453109883,0.00685334543204856,0.0646121015421161));
#31322=CARTESIAN_POINT('',(0.00140407618790463,0.00689970730319593,0.0644832220838221));
#31323=CARTESIAN_POINT('',(0.00288371938314982,0.00642352810991429,0.0644233065416496));
#31324=CARTESIAN_POINT('',(0.005309336296788,0.00462477015074507,0.0642944135101592));
#31325=CARTESIAN_POINT('',(0.00619475825082075,0.00334682586406391,0.0642344532891416));
#31326=CARTESIAN_POINT('',(0.00702697515087906,0.000444852087110999,0.0641056686116773));
#31327=CARTESIAN_POINT('',(0.00695291950131206,-0.0011092662960417,0.0640455489219221));
#31328=CARTESIAN_POINT('',(0.00612590467155436,-0.00321558785452446,0.0639491328687));
#31329=CARTESIAN_POINT('',(0.00574133930046712,-0.00385851491281968,0.0639188963398855));
#31330=CARTESIAN_POINT('',(0.00502296501430019,-0.00471231620408937,0.063872667496557));
#31331=CARTESIAN_POINT('',(0.00475786680289066,-0.00498021195944635,0.0638567915710753));
#31332=CARTESIAN_POINT('',(0.00418516527491888,-0.00547030157273569,0.0638247185405946));
#31333=CARTESIAN_POINT('',(0.00387251719149399,-0.00568369380262507,0.0638085680544166));
#31334=CARTESIAN_POINT('',(0.00356230190421146,-0.00589869296784463,0.0637924612621064));
#31335=CARTESIAN_POINT('',(-0.00720467396309524,0.,0.0666220238111755));
#31336=CARTESIAN_POINT('',(-0.00720467396309524,0.000771545181563554,0.0665921254986072));
#31337=CARTESIAN_POINT('',(-0.00707737061217141,0.0015632099741909,0.0665598446460228));
#31338=CARTESIAN_POINT('',(-0.00656973347090607,0.00306127462451411,0.0664954011460626));
#31339=CARTESIAN_POINT('',(-0.00619343675102207,0.00376143753484143,0.0664639550629926));
#31340=CARTESIAN_POINT('',(-0.00525255322852593,0.00499176879461846,0.066403474110719));
#31341=CARTESIAN_POINT('',(-0.00466894054319066,0.00554377127911973,0.0663710158263576));
#31342=CARTESIAN_POINT('',(-0.00335559377774765,0.00642435959374813,0.0663066332805016));
#31343=CARTESIAN_POINT('',(-0.00263675271024423,0.00674972179722307,0.066275888026252));
#31344=CARTESIAN_POINT('',(-0.00113679711813476,0.00715673818908369,0.0662147716789148));
#31345=CARTESIAN_POINT('',(-0.000336594616466026,0.00724004987170665,0.0661821670776257));
#31346=CARTESIAN_POINT('',(0.00124053482663403,0.00714091670757624,0.0661179062479404));
#31347=CARTESIAN_POINT('',(0.00200466179446659,0.00696393159598188,0.066087725787171));
#31348=CARTESIAN_POINT('',(0.00344781601569853,0.00637397653789229,0.0660260248413628));
#31349=CARTESIAN_POINT('',(0.00413445344475077,0.00595287611303322,0.0659933055226432));
#31350=CARTESIAN_POINT('',(0.00532533980382573,0.00491642098255655,0.0659292267883894));
#31351=CARTESIAN_POINT('',(0.00582268335291664,0.00431449052447686,0.0658994733893697));
#31352=CARTESIAN_POINT('',(0.00661257732290065,0.00296517976905168,0.0658372403784784));
#31353=CARTESIAN_POINT('',(0.00690167503461391,0.00221263519464696,0.0658044383237555));
#31354=CARTESIAN_POINT('',(0.0072168592290007,0.000667694283928396,0.0657406014931437));
#31355=CARTESIAN_POINT('',(0.00724633938141386,-0.000110175339427985,0.0657111361365049));
#31356=CARTESIAN_POINT('',(0.00705315591341762,-0.0016657024635479,0.0656484251924099));
#31357=CARTESIAN_POINT('',(0.00682472860842485,-0.00243926266682821,0.0656155726596287));
#31358=CARTESIAN_POINT('',(0.00613700814849502,-0.00385539283624122,0.0655520367853255));
#31359=CARTESIAN_POINT('',(0.00568872995236311,-0.00449028558147216,0.0655227195808207));
#31360=CARTESIAN_POINT('',(0.00458748313451537,-0.00561064270512987,0.0654595862856965));
#31361=CARTESIAN_POINT('',(0.00393550003547636,-0.00608575670502184,0.0654267157019463));
#31362=CARTESIAN_POINT('',(0.00253130419023423,-0.00679095680287067,0.0653635389015151));
#31363=CARTESIAN_POINT('',(0.00178964783853592,-0.00702309355571597,0.0653342295102171));
#31364=CARTESIAN_POINT('',(0.000231221316387449,-0.00724384008528374,0.0652707307392347));
#31365=CARTESIAN_POINT('',(-0.000575154778884747,-0.00722434031819303,0.0652378745921713));
#31366=CARTESIAN_POINT('',(-0.00211546753351723,-0.00693157220025716,0.0651751138745773));
#31367=CARTESIAN_POINT('',(-0.00284669800885144,-0.00666520705727002,0.0651456719338822));
#31368=CARTESIAN_POINT('',(-0.00422056774711423,-0.00589198460299243,0.0650818656896961));
#31369=CARTESIAN_POINT('',(-0.00484843298374087,-0.0053862352840386,0.0650490564185323));
#31370=CARTESIAN_POINT('',(-0.00589114670758562,-0.00422057145450138,0.0649867675177736));
#31371=CARTESIAN_POINT('',(-0.00631153849374279,-0.00356297150189047,0.0649570530665531));
#31372=CARTESIAN_POINT('',(-0.00693323487746813,-0.0021119986304778,0.0648929983065474));
#31373=CARTESIAN_POINT('',(-0.00712379084016052,-0.00132929239925322,0.0648602681933891));
#31374=CARTESIAN_POINT('',(-0.00724323560290229,0.000225725979709869,0.0647985054102385));
#31375=CARTESIAN_POINT('',(-0.00717758356137153,0.0010068765615664,0.0647683793114804));
#31376=CARTESIAN_POINT('',(-0.00659443097403759,0.00330416769367967,0.0646720139975049));
#31377=CARTESIAN_POINT('',(-0.00570767050133428,0.00467224431138081,0.0646118432423536));
#31378=CARTESIAN_POINT('',(-0.00322660357742274,0.00663297812533666,0.0644830992416911));
#31379=CARTESIAN_POINT('',(-0.0016921349492112,0.00717954050046661,0.0644231134477039));
#31380=CARTESIAN_POINT('',(0.00147090526178086,0.00722810903314606,0.0642942339894098));
#31381=CARTESIAN_POINT('',(0.00302097425390042,0.00672926538991485,0.0642343184472374));
#31382=CARTESIAN_POINT('',(0.00556204197662814,0.00484489289673792,0.064105425415747));
#31383=CARTESIAN_POINT('',(0.00648960689247979,0.00350612296976741,0.0640454651947294));
#31384=CARTESIAN_POINT('',(0.00736143438146067,0.000466025477308509,0.0639166805172651));
#31385=CARTESIAN_POINT('',(0.00728385394419447,-0.00116206345896291,0.0638565608275099));
#31386=CARTESIAN_POINT('',(0.006417476125711,-0.00336863849389627,0.0637601447742877));
#31387=CARTESIAN_POINT('',(0.00601460679945664,-0.00404216661233763,0.0637299082454732));
#31388=CARTESIAN_POINT('',(0.00526204043122564,-0.00493660583341584,0.0636836794021448));
#31389=CARTESIAN_POINT('',(0.00498432448004717,-0.00521725248176574,0.0636678034766631));
#31390=CARTESIAN_POINT('',(0.00438436437946263,-0.00573066863193009,0.0636357304461824));
#31391=CARTESIAN_POINT('',(0.0040568353500859,-0.00595421757925314,0.0636195799600043));
#31392=CARTESIAN_POINT('',(0.00373185490936659,-0.00617944994635986,0.0636034731676942));
#31393=CARTESIAN_POINT('',(-0.00753201094464286,0.,0.0664330357167633));
#31394=CARTESIAN_POINT('',(-0.00753201094464286,0.000806599546570811,0.0664031374041949));
#31395=CARTESIAN_POINT('',(-0.00739892369637049,0.00163423281812497,0.0663708565516105));
#31396=CARTESIAN_POINT('',(-0.00686822258157983,0.00320036050132265,0.0663064130516504));
#31397=CARTESIAN_POINT('',(-0.00647482920568002,0.00393233459628263,0.0662749669685803));
#31398=CARTESIAN_POINT('',(-0.00549119760411474,0.00521856469658208,0.0662144860163068));
#31399=CARTESIAN_POINT('',(-0.0048810690742334,0.00579564684853382,0.0661820277319454));
#31400=CARTESIAN_POINT('',(-0.00350805174380334,0.00671624379122409,0.0661176451860894));
#31401=CARTESIAN_POINT('',(-0.00275655086872857,0.00705638849313556,0.0660868999318397));
#31402=CARTESIAN_POINT('',(-0.00118844633074152,0.00748189725784116,0.0660257835845025));
#31403=CARTESIAN_POINT('',(-0.000351887448081106,0.00756899412142541,0.0659931789832135));
#31404=CARTESIAN_POINT('',(0.00129689725576478,0.00746535694352784,0.0659289181535282));
#31405=CARTESIAN_POINT('',(0.00209574154966243,0.0072803306946794,0.0658987376927588));
#31406=CARTESIAN_POINT('',(0.00360446400466949,0.00666357163283433,0.0658370367469506));
#31407=CARTESIAN_POINT('',(0.00432229810196721,0.0062233389415177,0.065804317428231));
#31408=CARTESIAN_POINT('',(0.0055672911629058,0.00513979353386018,0.0657402386939771));
#31409=CARTESIAN_POINT('',(0.00608723100670561,0.00451051498199323,0.0657104852949574));
#31410=CARTESIAN_POINT('',(0.00691301300010353,0.00309989967453515,0.0656482522840662));
#31411=CARTESIAN_POINT('',(0.00721524557021695,0.00231316400824654,0.0656154502293433));
#31412=CARTESIAN_POINT('',(0.007544749835623,0.000698030289779218,0.0655516133987315));
#31413=CARTESIAN_POINT('',(0.00757556938856363,-0.000115181043118961,0.0655221480420927));
#31414=CARTESIAN_POINT('',(0.00737360882758266,-0.00174138194874975,0.0654594370979977));
#31415=CARTESIAN_POINT('',(0.00713480316197254,-0.00255008806748497,0.0654265845652165));
#31416=CARTESIAN_POINT('',(0.00641583682739869,-0.00403055866056026,0.0653630486909132));
#31417=CARTESIAN_POINT('',(0.00594719157061045,-0.00469429710733092,0.0653337314864085));
#31418=CARTESIAN_POINT('',(0.00479591073163425,-0.0058655565092863,0.0652705981912843));
#31419=CARTESIAN_POINT('',(0.00411430544833643,-0.00636225682708971,0.065237727607534));
#31420=CARTESIAN_POINT('',(0.00264631140322602,-0.0070994969690265,0.0651745508071028));
#31421=CARTESIAN_POINT('',(0.00187095865488935,-0.00734218061745262,0.0651452414158048));
#31422=CARTESIAN_POINT('',(0.00024172662005052,-0.00757295653947395,0.0650817426448225));
#31423=CARTESIAN_POINT('',(-0.000601286347114926,-0.00755257082043967,0.065048886497759));
#31424=CARTESIAN_POINT('',(-0.00221158163396516,-0.00724650108295663,0.0649861257801651));
#31425=CARTESIAN_POINT('',(-0.00297603481692467,-0.00696803391254375,0.06495668383947));
#31426=CARTESIAN_POINT('',(-0.00441232491944907,-0.00615968088809122,0.0648928775952838));
#31427=CARTESIAN_POINT('',(-0.00506871656996048,-0.00563095336688506,0.0648600683241201));
#31428=CARTESIAN_POINT('',(-0.00615880492376489,-0.00441232879527757,0.0647977794233614));
#31429=CARTESIAN_POINT('',(-0.00659829678010608,-0.00372485146241931,0.0647680649721409));
#31430=CARTESIAN_POINT('',(-0.00724823930220355,-0.00220795512486944,0.0647040102121351));
#31431=CARTESIAN_POINT('',(-0.00744745297986863,-0.00138968743777885,0.0646712800989769));
#31432=CARTESIAN_POINT('',(-0.00757232459305469,0.000235981608380033,0.0646095173158262));
#31433=CARTESIAN_POINT('',(-0.00750368971826635,0.00105262296676703,0.0645793912170681));
#31434=CARTESIAN_POINT('',(-0.00689404219046773,0.00345428916828302,0.0644830259030927));
#31435=CARTESIAN_POINT('',(-0.00596699266402274,0.00488452294574713,0.0644228551479413));
#31436=CARTESIAN_POINT('',(-0.00337320100585524,0.00693434069210107,0.0642941111472789));
#31437=CARTESIAN_POINT('',(-0.00176901536732356,0.00750573556888466,0.0642341253532916));
#31438=CARTESIAN_POINT('',(0.0015377343356571,0.00755651076309619,0.0641052458949976));
#31439=CARTESIAN_POINT('',(0.00315822912465102,0.00703500266991541,0.0640453303528252));
#31440=CARTESIAN_POINT('',(0.00581474765646829,0.00506501564273076,0.0639164373213348));
#31441=CARTESIAN_POINT('',(0.00678445553413884,0.00366542007547091,0.0638564771003172));
#31442=CARTESIAN_POINT('',(0.00769589361204228,0.00048719886750602,0.0637276924228528));
#31443=CARTESIAN_POINT('',(0.00761478838707688,-0.00121486062188411,0.0636675727330976));
#31444=CARTESIAN_POINT('',(0.00670904757986764,-0.00352168913326807,0.0635711566798755));
#31445=CARTESIAN_POINT('',(0.00628787429844615,-0.00422581831185558,0.063540920151061));
#31446=CARTESIAN_POINT('',(0.00550111584815108,-0.00516089546274231,0.0634946913077325));
#31447=CARTESIAN_POINT('',(0.00521078215720368,-0.00545429300408513,0.0634788153822508));
#31448=CARTESIAN_POINT('',(0.00458356348400637,-0.0059910356911245,0.0634467423517701));
#31449=CARTESIAN_POINT('',(0.00424115350867781,-0.00622474135588122,0.0634305918655921));
#31450=CARTESIAN_POINT('',(0.00390140791452173,-0.0064602069248751,0.0634144850732819));
#31451=CARTESIAN_POINT('',(-0.00704100547232143,0.,0.0667165178583817));
#31452=CARTESIAN_POINT('',(-0.00655,0.,0.067));
#31453=CARTESIAN_POINT('',(-0.00753201094464286,0.,0.0664330357167633));
#31454=CARTESIAN_POINT('',(-0.00753201094464286,0.,0.0664330357167633));
#31455=CARTESIAN_POINT('',(-0.00753201094464286,0.00244729870815628,0.066342321431049));
#31456=CARTESIAN_POINT('',(-0.00609352485603417,0.00442720495336657,0.0662516071453347));
#31457=CARTESIAN_POINT('',(-0.00465503876742549,0.00640711119857685,0.0661608928596204));
#31458=CARTESIAN_POINT('',(-0.00232751938371274,0.00716336808970901,0.0660701785739062));
#31459=CARTESIAN_POINT('',(-4.84937169161726E-19,0.00791962498084115,0.0659794642881919));
#31460=CARTESIAN_POINT('',(0.00232751938371274,0.00716336808970901,0.0658887500024776));
#31461=CARTESIAN_POINT('',(0.00465503876742549,0.00640711119857685,0.0657980357167633));
#31462=CARTESIAN_POINT('',(0.00609352485603417,0.00442720495336657,0.065707321431049));
#31463=CARTESIAN_POINT('',(0.00753201094464286,0.00244729870815628,0.0656166071453347));
#31464=CARTESIAN_POINT('',(0.00753201094464286,9.22405309449971E-19,0.0655258928596205));
#31465=CARTESIAN_POINT('',(0.00753201094464286,-0.00244729870815628,0.0654351785739062));
#31466=CARTESIAN_POINT('',(0.00609352485603417,-0.00442720495336657,0.0653444642881919));
#31467=CARTESIAN_POINT('',(0.00465503876742549,-0.00640711119857685,0.0652537500024776));
#31468=CARTESIAN_POINT('',(0.00232751938371274,-0.00716336808970901,0.0651630357167633));
#31469=CARTESIAN_POINT('',(1.45481150748518E-18,-0.00791962498084115,0.0650723214310489));
#31470=CARTESIAN_POINT('',(-0.00232751938371274,-0.00716336808970901,0.0649816071453347));
#31471=CARTESIAN_POINT('',(-0.00465503876742549,-0.00640711119857685,0.0648908928596204));
#31472=CARTESIAN_POINT('',(-0.00609352485603417,-0.00442720495336658,0.0648001785739062));
#31473=CARTESIAN_POINT('',(-0.00753201094464286,-0.00244729870815628,0.0647094642881918));
#31474=CARTESIAN_POINT('',(-0.00753201094464286,0.,0.0646187500024776));
#31475=CARTESIAN_POINT('',(-0.00753201094464286,0.00244729870815628,0.0645280357167632));
#31476=CARTESIAN_POINT('',(-0.00609352485603417,0.00442720495336657,0.064437321431049));
#31477=CARTESIAN_POINT('',(-0.00465503876742549,0.00640711119857685,0.0643466071453347));
#31478=CARTESIAN_POINT('',(-0.00232751938371274,0.00716336808970901,0.0642558928596204));
#31479=CARTESIAN_POINT('',(-4.84937169161726E-19,0.00791962498084115,0.0641651785739061));
#31480=CARTESIAN_POINT('',(0.00232751938371274,0.00716336808970901,0.0640744642881919));
#31481=CARTESIAN_POINT('',(0.00465503876742549,0.00640711119857685,0.0639837500024776));
#31482=CARTESIAN_POINT('',(0.00609352485603417,0.00442720495336657,0.0638930357167633));
#31483=CARTESIAN_POINT('',(0.00753201094464286,0.00244729870815628,0.063802321431049));
#31484=CARTESIAN_POINT('',(0.00753201094464286,9.22405309449971E-19,0.0637116071453347));
#31485=CARTESIAN_POINT('',(0.00753201094464286,-0.00244729870815628,0.0636208928596204));
#31486=CARTESIAN_POINT('',(0.00609352485603417,-0.00442720495336657,0.0635301785739062));
#31487=CARTESIAN_POINT('',(0.00534171654646512,-0.00546198031831741,0.0634827677895151));
#31488=CARTESIAN_POINT('',(0.00429046182728509,-0.00619056751670065,0.0634329294936898));
#31489=CARTESIAN_POINT('',(0.00429046182728508,-0.00619056751670066,0.0634329294936898));
#31490=CARTESIAN_POINT('',(0.00401076826589901,-0.00578701097100319,0.063716411528697));
#31491=CARTESIAN_POINT('',(0.00373107470451293,-0.00538345442530572,0.0639998935637042));
#31492=CARTESIAN_POINT('',(0.00655,8.02143653441517E-19,0.0642785714285715));
#31493=CARTESIAN_POINT('',(0.00655000000000002,-0.00212822401032552,0.0641878571428572));
#31494=CARTESIAN_POINT('',(0.00529906131315591,-0.0038499934025157,0.0640971428571429));
#31495=CARTESIAN_POINT('',(0.00464527107021772,-0.00474985847267627,0.0640497319684088));
#31496=CARTESIAN_POINT('',(0.00373107470451293,-0.00538345442530572,0.0639998935637043));
#31497=CARTESIAN_POINT('',(0.00655,8.02143653441516E-19,0.0642785714285715));
#31498=CARTESIAN_POINT('',(-0.00655,0.,0.0651857142857143));
#31499=CARTESIAN_POINT('',(-0.00655000000000001,0.00212822401032553,0.065095));
#31500=CARTESIAN_POINT('',(-0.00529906131315591,0.0038499934025157,0.0650042857142857));
#31501=CARTESIAN_POINT('',(-0.00404812262631181,0.00557176279470586,0.0649135714285714));
#31502=CARTESIAN_POINT('',(-0.0020240613131559,0.00622942018173326,0.0648228571428572));
#31503=CARTESIAN_POINT('',(-4.21711875003113E-19,0.00688707756876065,0.0647321428571428));
#31504=CARTESIAN_POINT('',(0.0020240613131559,0.00622942018173326,0.0646414285714286));
#31505=CARTESIAN_POINT('',(0.00404812262631181,0.00557176279470586,0.0645507142857142));
#31506=CARTESIAN_POINT('',(0.00529906131315591,0.0038499934025157,0.06446));
#31507=CARTESIAN_POINT('',(0.00654999999999999,0.00212822401032556,0.0643692857142857));
#31508=CARTESIAN_POINT('',(0.00655,8.02143653441516E-19,0.0642785714285714));
#31509=CARTESIAN_POINT('',(-0.00655,0.,0.0651857142857143));
#31510=CARTESIAN_POINT('',(0.00655,8.02143653441517E-19,0.0660928571428572));
#31511=CARTESIAN_POINT('',(0.00655000000000001,-0.00212822401032553,0.0660021428571429));
#31512=CARTESIAN_POINT('',(0.00529906131315591,-0.0038499934025157,0.0659114285714286));
#31513=CARTESIAN_POINT('',(0.00404812262631181,-0.00557176279470586,0.0658207142857143));
#31514=CARTESIAN_POINT('',(0.0020240613131559,-0.00622942018173326,0.06573));
#31515=CARTESIAN_POINT('',(1.26513562500934E-18,-0.00688707756876065,0.0656392857142857));
#31516=CARTESIAN_POINT('',(-0.0020240613131559,-0.00622942018173326,0.0655485714285714));
#31517=CARTESIAN_POINT('',(-0.00404812262631181,-0.00557176279470586,0.0654578571428572));
#31518=CARTESIAN_POINT('',(-0.00529906131315591,-0.0038499934025157,0.0653671428571429));
#31519=CARTESIAN_POINT('',(-0.00654999999999999,-0.00212822401032555,0.0652764285714286));
#31520=CARTESIAN_POINT('',(-0.00655,0.,0.0651857142857143));
#31521=CARTESIAN_POINT('',(0.00655,8.02143653441516E-19,0.0660928571428572));
#31522=CARTESIAN_POINT('',(-0.00655,0.,0.067));
#31523=CARTESIAN_POINT('',(-0.00655,0.00212822401032553,0.0669092857142857));
#31524=CARTESIAN_POINT('',(-0.00529906131315591,0.0038499934025157,0.0668185714285715));
#31525=CARTESIAN_POINT('',(-0.00404812262631181,0.00557176279470586,0.0667278571428571));
#31526=CARTESIAN_POINT('',(-0.0020240613131559,0.00622942018173326,0.0666371428571429));
#31527=CARTESIAN_POINT('',(-4.21711875003113E-19,0.00688707756876065,0.0665464285714285));
#31528=CARTESIAN_POINT('',(0.0020240613131559,0.00622942018173326,0.0664557142857143));
#31529=CARTESIAN_POINT('',(0.00404812262631181,0.00557176279470586,0.066365));
#31530=CARTESIAN_POINT('',(0.00529906131315591,0.0038499934025157,0.0662742857142857));
#31531=CARTESIAN_POINT('',(0.00654999999999999,0.00212822401032555,0.0661835714285715));
#31532=CARTESIAN_POINT('',(0.00655,8.02143653441516E-19,0.0660928571428572));
#31533=CARTESIAN_POINT('',(-3.90312782094781E-18,0.,0.0657884338054059));
#31534=CARTESIAN_POINT('',(-0.00753201094464286,0.,0.0663196428596204));
#31535=CARTESIAN_POINT('',(0.00429046128025484,-0.00619056789582776,0.0633195366106131));
#31536=CARTESIAN_POINT('',(0.0042904607332246,-0.00619056827495487,0.0632628401561078));
#31537=CARTESIAN_POINT('',(0.00373107721004495,-0.00538345487953476,0.0639998935637042));
#31538=CARTESIAN_POINT('',(-0.00753201094464286,0.,0.0663196428596204));
#31539=CARTESIAN_POINT('',(-0.00655,0.,0.0663196428596204));
#31540=CARTESIAN_POINT('',(0.,0.,0.062));
#31541=CARTESIAN_POINT('',(0.,0.,0.062));
#31542=CARTESIAN_POINT('',(0.00655,0.,0.062));
#31543=CARTESIAN_POINT('',(0.,0.,0.062));
#31544=CARTESIAN_POINT('',(0.00855,0.,0.062));
#31545=CARTESIAN_POINT('',(0.,0.,0.064));
#31546=CARTESIAN_POINT('',(-0.025980762113538,-0.0149999999999972,0.064));
#31547=CARTESIAN_POINT('',(-0.028759522113538,-0.0149999999999972,0.064));
#31548=CARTESIAN_POINT('',(0.0259807621135283,-0.0150000000000028,0.064));
#31549=CARTESIAN_POINT('',(0.0232020021135283,-0.0150000000000028,0.064));
#31550=CARTESIAN_POINT('',(0.,0.03,0.064));
#31551=CARTESIAN_POINT('',(-0.00277876,0.03,0.064));
#31552=CARTESIAN_POINT('',(-0.0259807621135331,-0.015,0.064));
#31553=CARTESIAN_POINT('',(0.,0.,0.064));
#31554=CARTESIAN_POINT('',(-0.01055,0.,0.064));
#31555=CARTESIAN_POINT('',(0.,0.,0.064));
#31556=CARTESIAN_POINT('',(-0.00493432083723898,0.00759818777748466,0.064));
#31557=CARTESIAN_POINT('',(-0.0259807621135331,-0.015,0.064));
#31558=CARTESIAN_POINT('',(-0.0259807621135331,-0.015,0.065));
#31559=CARTESIAN_POINT('',(-0.0259807621135331,-0.015,0.066));
#31560=CARTESIAN_POINT('',(0.00411306321940664,-0.00807234108421418,0.064));
#31561=CARTESIAN_POINT('',(-0.00356046479940298,-0.0119821988972063,0.064));
#31562=CARTESIAN_POINT('',(0.,0.,0.064));
#31563=CARTESIAN_POINT('',(-0.00411306321940666,-0.00807234108421419,0.064));
#31564=CARTESIAN_POINT('',(0.00493432083723899,0.00759818777748466,0.064));
#31565=CARTESIAN_POINT('',(0.,0.,0.064));
#31566=CARTESIAN_POINT('',(0.00904738405664563,0.000474153306729528,0.064));
#31567=CARTESIAN_POINT('',(0.,0.03,0.064));
#31568=CARTESIAN_POINT('',(-0.00904738405664563,0.000474153306729528,0.064));
#31569=CARTESIAN_POINT('',(0.,0.,0.067));
#31570=CARTESIAN_POINT('',(-0.0259807621135331,-0.015,0.067));
#31571=CARTESIAN_POINT('',(0.,0.03,0.067));
#31572=CARTESIAN_POINT('',(-0.0012192,0.03,0.067));
#31573=CARTESIAN_POINT('',(0.0259807621135283,-0.0150000000000028,0.067));
#31574=CARTESIAN_POINT('',(0.0247615621135283,-0.0150000000000028,0.067));
#31575=CARTESIAN_POINT('',(-0.025980762113538,-0.0149999999999972,0.067));
#31576=CARTESIAN_POINT('',(-0.027199962113538,-0.0149999999999972,0.067));
#31577=CARTESIAN_POINT('',(0.,0.,0.067));
#31578=CARTESIAN_POINT('',(0.,0.,0.064));
#31579=CARTESIAN_POINT('',(0.0259807621135331,-0.015,0.064));
#31580=CARTESIAN_POINT('',(-0.025980762113538,-0.0149999999999972,0.064));
#31581=CARTESIAN_POINT('',(-0.025980762113538,-0.0149999999999972,0.064));
#31582=CARTESIAN_POINT('',(0.0259807621135283,-0.0150000000000028,0.064));
#31583=CARTESIAN_POINT('',(0.0259807621135283,-0.0150000000000028,0.064));
#31584=CARTESIAN_POINT('',(0.,0.03,0.064));
#31585=CARTESIAN_POINT('',(0.,0.03,0.064));
#31586=CARTESIAN_POINT('',(-0.0259807621135331,-0.015,0.066));
#31587=CARTESIAN_POINT('',(-0.0259807621135331,-0.015,0.065));
#31588=CARTESIAN_POINT('',(0.,0.,0.063));
#31589=CARTESIAN_POINT('',(0.,0.,0.063));
#31590=CARTESIAN_POINT('',(-0.00955,0.,0.063));
#31591=CARTESIAN_POINT('',(0.,0.,0.063));
#31592=CARTESIAN_POINT('',(6.70275947721334E-18,0.,0.0107004836836099));
#31593=CARTESIAN_POINT('',(0.0019558,0.00019685,-0.00019685));
#31594=CARTESIAN_POINT('',(0.00464692103339967,-6.71076465535595E-18,0.00190886483457572));
#31595=CARTESIAN_POINT('',(0.000213232602987236,0.000372238276972069,-0.00156035241129895));
#31596=CARTESIAN_POINT('',(0.000213232602987236,-0.000372238276972058,-0.00156035241129895));
#31597=CARTESIAN_POINT('',(0.,-0.000393699999999994,-0.0017272));
#31598=CARTESIAN_POINT('',(0.0019558,-0.00019685,-0.00019685));
#31599=CARTESIAN_POINT('',(0.0019558,0.00019685,-0.00019685));
#31600=CARTESIAN_POINT('',(0.0019558,0.00019685,-0.00019685));
#31601=CARTESIAN_POINT('',(0.,0.000393700000000006,-0.0017272));
#31602=CARTESIAN_POINT('',(0.00220737593360996,-0.000171529045643153,-5.98890461932643E-19));
#31603=CARTESIAN_POINT('',(0.00222429738224716,-0.000169825912825772,-0.000169825912825772));
#31604=CARTESIAN_POINT('',(2.49715212940994E-5,-0.000391186632597021,-0.000391186632597022));
#31605=CARTESIAN_POINT('',(0.0061181923658055,0.000222092088766138,7.75430383431664E-19));
#31606=CARTESIAN_POINT('',(0.00220737593360996,0.000171529045643153,5.98890461932643E-19));
#31607=CARTESIAN_POINT('',(0.00222429738224716,0.000169825912825773,-0.000169825912825772));
#31608=CARTESIAN_POINT('',(2.49715212940986E-5,0.000391186632597024,-0.000391186632597022));
#31609=CARTESIAN_POINT('',(0.0061181923658055,-0.000222092088766138,-8.02590401435484E-19));
#31610=CARTESIAN_POINT('',(0.0019558,-0.00019685,0.00019685));
#31611=CARTESIAN_POINT('',(0.00464692103339967,6.88160638279209E-18,-0.00190886483457572));
#31612=CARTESIAN_POINT('',(0.000213232602987235,-0.000372238276972069,0.00156035241129894));
#31613=CARTESIAN_POINT('',(0.000213232602987237,0.000372238276972058,0.00156035241129895));
#31614=CARTESIAN_POINT('',(0.,0.000393699999999994,0.0017272));
#31615=CARTESIAN_POINT('',(0.0019558,0.00019685,0.00019685));
#31616=CARTESIAN_POINT('',(0.0019558,-0.00019685,0.00019685));
#31617=CARTESIAN_POINT('',(0.0019558,-0.00019685,0.00019685));
#31618=CARTESIAN_POINT('',(0.,-0.000393700000000006,0.0017272));
#31619=CARTESIAN_POINT('',(0.00220737593360996,-0.000171529045643153,-5.98890461932643E-19));
#31620=CARTESIAN_POINT('',(0.00222429738224716,-0.000169825912825773,0.000169825912825772));
#31621=CARTESIAN_POINT('',(2.49715212940986E-5,-0.000391186632597024,0.000391186632597022));
#31622=CARTESIAN_POINT('',(0.0061181923658055,0.000222092088766138,7.75430383431664E-19));
#31623=CARTESIAN_POINT('',(0.00220737593360996,0.000171529045643153,5.98890461932643E-19));
#31624=CARTESIAN_POINT('',(0.00222429738224716,0.000169825912825772,0.000169825912825772));
#31625=CARTESIAN_POINT('',(2.49715212940994E-5,0.000391186632597021,0.000391186632597022));
#31626=CARTESIAN_POINT('',(0.0061181923658055,-0.000222092088766138,-8.02590401435484E-19));
#31627=CARTESIAN_POINT('',(0.0019558,-0.00019685,-0.00019685));
#31628=CARTESIAN_POINT('',(0.,-0.0017272,-0.0003937));
#31629=CARTESIAN_POINT('',(0.000213232602987236,-0.00156035241129895,-0.000372238276972064));
#31630=CARTESIAN_POINT('',(0.00464692103339967,0.00190886483457572,2.62839141558061E-19));
#31631=CARTESIAN_POINT('',(0.000213232602987236,-0.00156035241129895,0.000372238276972064));
#31632=CARTESIAN_POINT('',(0.,-0.0017272,0.0003937));
#31633=CARTESIAN_POINT('',(0.0019558,-0.00019685,-0.00019685));
#31634=CARTESIAN_POINT('',(0.0019558,0.00019685,0.00019685));
#31635=CARTESIAN_POINT('',(0.00464692103339967,-0.00190886483457572,0.));
#31636=CARTESIAN_POINT('',(0.000213232602987235,0.00156035241129895,0.000372238276972064));
#31637=CARTESIAN_POINT('',(0.000213232602987235,0.00156035241129895,-0.000372238276972064));
#31638=CARTESIAN_POINT('',(0.,0.0017272,-0.0003937));
#31639=CARTESIAN_POINT('',(0.0019558,0.00019685,0.00019685));
#31640=CARTESIAN_POINT('',(0.,0.0017272,0.0003937));
#31641=CARTESIAN_POINT('',(0.0019558,0.00019685,0.00019685));
#31642=CARTESIAN_POINT('',(0.0014986,0.0012573,0.));
#31643=CARTESIAN_POINT('',(0.0014986,0.,0.));
#31644=CARTESIAN_POINT('',(0.0014986,0.,0.0012573));
#31645=CARTESIAN_POINT('',(0.0014986,0.,0.));
#31646=CARTESIAN_POINT('',(0.0014986,0.,0.0026416));
#31647=CARTESIAN_POINT('',(0.0078486,0.0012573,0.));
#31648=CARTESIAN_POINT('',(0.0078486,0.,0.));
#31649=CARTESIAN_POINT('',(0.0078486,0.,0.0012573));
#31650=CARTESIAN_POINT('',(0.00220737593360996,0.,0.000171529045643153));
#31651=CARTESIAN_POINT('',(0.0061181923658055,2.16840434497101E-19,-0.000222092088766138));
#31652=CARTESIAN_POINT('',(0.00220737593360996,0.,0.000171529045643153));
#31653=CARTESIAN_POINT('',(0.0061181923658055,2.16840434497101E-19,-0.000222092088766138));
#31654=CARTESIAN_POINT('',(0.00220737593360996,0.,-0.000171529045643153));
#31655=CARTESIAN_POINT('',(0.0061181923658055,1.89680416493284E-19,0.000222092088766138));
#31656=CARTESIAN_POINT('',(0.00220737593360996,0.,-0.000171529045643153));
#31657=CARTESIAN_POINT('',(0.0061181923658055,1.89680416493284E-19,0.000222092088766138));
#31658=CARTESIAN_POINT('',(0.00614054579032417,2.16840434497101E-19,0.));
#31659=CARTESIAN_POINT('',(0.0005588,0.,0.));
#31660=CARTESIAN_POINT('',(0.0005588,0.,0.00255937815401834));
#31661=CARTESIAN_POINT('',(-0.0254,0.,0.));
#31662=CARTESIAN_POINT('',(0.0014986,0.,0.));
#31663=CARTESIAN_POINT('',(-1.38777878078145E-16,0.043,0.083));
#31664=CARTESIAN_POINT('',(-0.043,1.38777878078145E-17,0.083));
#31665=CARTESIAN_POINT('',(0.,0.03,0.1));
#31666=CARTESIAN_POINT('',(0.,0.03,0.1));
#31667=CARTESIAN_POINT('',(-0.004,0.03,0.1));
#31668=CARTESIAN_POINT('',(0.,0.03,0.1));
#31669=CARTESIAN_POINT('',(-0.0012192,0.03,0.1));
#31670=CARTESIAN_POINT('',(0.,0.03,0.067));
#31671=CARTESIAN_POINT('',(0.,0.03,0.067));
#31672=CARTESIAN_POINT('',(-0.004,0.03,0.067));
#31673=CARTESIAN_POINT('',(0.,0.03,0.067));
#31674=CARTESIAN_POINT('',(-0.0012192,0.03,0.067));
#31675=CARTESIAN_POINT('',(0.,0.03,0.067));
#31676=CARTESIAN_POINT('',(0.,0.03,0.064));
#31677=CARTESIAN_POINT('',(0.,0.03,0.0936825692667184));
#31678=CARTESIAN_POINT('',(0.0012192,0.03,0.0936825692667184));
#31679=CARTESIAN_POINT('',(0.,0.03,0.0936825692667184));
#31680=CARTESIAN_POINT('',(-2.60208521396521E-18,0.03,0.09295));
#31681=CARTESIAN_POINT('',(0.,0.03,0.0733174307332816));
#31682=CARTESIAN_POINT('',(0.,0.03,0.0733174307332816));
#31683=CARTESIAN_POINT('',(-0.0012192,0.03,0.0733174307332816));
#31684=CARTESIAN_POINT('',(-2.60208521396521E-18,0.03,0.07405));
#31685=CARTESIAN_POINT('',(0.,0.03,0.064));
#31686=CARTESIAN_POINT('',(-0.0290496459001986,0.0374911997085303,0.0107004836836099));
#31687=CARTESIAN_POINT('',(0.,0.03,0.11392908368361));
#31688=CARTESIAN_POINT('',(0.,0.0100000000000245,0.054000001));
#31689=CARTESIAN_POINT('',(0.,0.,0.054000001));
#31690=CARTESIAN_POINT('',(-0.0045499999999755,0.,0.054000001));
#31691=CARTESIAN_POINT('',(0.,0.,0.054000001));
#31692=CARTESIAN_POINT('',(-0.0080000000000245,0.,0.054000001));
#31693=CARTESIAN_POINT('',(0.,0.0140000000000245,0.056000001));
#31694=CARTESIAN_POINT('',(0.,0.,0.056000001));
#31695=CARTESIAN_POINT('',(-0.0140000000000245,0.,0.056000001));
#31696=CARTESIAN_POINT('',(0.,0.,0.056000001));
#31697=CARTESIAN_POINT('',(-0.0045499999999755,0.,0.056000001));
#31698=CARTESIAN_POINT('',(0.,0.0120000000000245,0.050900001));
#31699=CARTESIAN_POINT('',(0.,0.,0.050900001));
#31700=CARTESIAN_POINT('',(-0.0120000000000245,0.,0.050900001));
#31701=CARTESIAN_POINT('',(0.,0.,0.050900001));
#31702=CARTESIAN_POINT('',(-0.0140000000000245,0.,0.050900001));
#31703=CARTESIAN_POINT('',(0.,0.0100000000000245,0.054000001));
#31704=CARTESIAN_POINT('',(0.,0.,0.054000001));
#31705=CARTESIAN_POINT('',(-0.0100000000000245,0.,0.054000001));
#31706=CARTESIAN_POINT('',(0.,0.,0.054000001));
#31707=CARTESIAN_POINT('',(-0.0120000000000245,0.,0.054000001));
#31708=CARTESIAN_POINT('',(0.,0.0080000000000245,0.04185765489));
#31709=CARTESIAN_POINT('',(0.,0.,0.04185765489));
#31710=CARTESIAN_POINT('',(-0.0080000000000245,0.,0.04185765489));
#31711=CARTESIAN_POINT('',(0.,0.,0.04185765489));
#31712=CARTESIAN_POINT('',(-0.00906043638285393,0.,0.04185765489));
#31713=CARTESIAN_POINT('',(0.,0.,0.04185765489));
#31714=CARTESIAN_POINT('',(0.,0.,0.0447833821488957));
#31715=CARTESIAN_POINT('',(-0.0100000000000245,0.,0.0447833821488957));
#31716=CARTESIAN_POINT('',(0.,0.,0.));
#31717=CARTESIAN_POINT('',(0.,0.,0.));
#31718=CARTESIAN_POINT('',(0.,0.,0.));
#31719=CARTESIAN_POINT('',(0.,0.,0.));
#31720=CARTESIAN_POINT('',(0.,0.,0.));
#31721=CARTESIAN_POINT('',(0.,0.,-0.000100001));
#31722=CARTESIAN_POINT('',(-0.008264,0.0303108891324553,0.083));
#31723=CARTESIAN_POINT('',(-0.00826400000000004,0.0327856678737492,0.0831322916666668));
#31724=CARTESIAN_POINT('',(-0.00950138937064697,0.0349288891324553,0.0832645833333334));
#31725=CARTESIAN_POINT('',(-0.0107387787412939,0.0370721103911615,0.0833968750000001));
#31726=CARTESIAN_POINT('',(-0.012882,0.0383094997618084,0.0835291666666667));
#31727=CARTESIAN_POINT('',(-0.0150252212587062,0.0395468891324554,0.0836614583333334));
#31728=CARTESIAN_POINT('',(-0.0175,0.0395468891324554,0.08379375));
#31729=CARTESIAN_POINT('',(-0.0199747787412939,0.0395468891324554,0.0839260416666667));
#31730=CARTESIAN_POINT('',(-0.022118,0.0383094997618084,0.0840583333333334));
#31731=CARTESIAN_POINT('',(-0.0242612212587062,0.0370721103911615,0.084190625));
#31732=CARTESIAN_POINT('',(-0.0254986106293531,0.0349288891324553,0.0843229166666667));
#31733=CARTESIAN_POINT('',(-0.0267360000000001,0.0327856678737492,0.0844552083333334));
#31734=CARTESIAN_POINT('',(-0.026736,0.0303108891324553,0.0845875));
#31735=CARTESIAN_POINT('',(-0.0267360000000001,0.0278361103911615,0.0847197916666667));
#31736=CARTESIAN_POINT('',(-0.0254986106293531,0.0256928891324554,0.0848520833333334));
#31737=CARTESIAN_POINT('',(-0.0242612212587062,0.0235496678737492,0.0849843750000001));
#31738=CARTESIAN_POINT('',(-0.022118,0.0223122785031023,0.0851166666666667));
#31739=CARTESIAN_POINT('',(-0.0199747787412939,0.0210748891324554,0.0852489583333334));
#31740=CARTESIAN_POINT('',(-0.0175,0.0210748891324553,0.08538125));
#31741=CARTESIAN_POINT('',(-0.0150252212587062,0.0210748891324553,0.0855135416666667));
#31742=CARTESIAN_POINT('',(-0.012882,0.0223122785031023,0.0856458333333334));
#31743=CARTESIAN_POINT('',(-0.0107387787412939,0.0235496678737492,0.0857781250000001));
#31744=CARTESIAN_POINT('',(-0.00950138937064697,0.0256928891324554,0.0859104166666667));
#31745=CARTESIAN_POINT('',(-0.00826400000000005,0.0278361103911615,0.0860427083333334));
#31746=CARTESIAN_POINT('',(-0.008264,0.0303108891324553,0.086175));
#31747=CARTESIAN_POINT('',(-0.00826400000000004,0.0327856678737492,0.0863072916666667));
#31748=CARTESIAN_POINT('',(-0.00950138937064697,0.0349288891324553,0.0864395833333334));
#31749=CARTESIAN_POINT('',(-0.0107387787412939,0.0370721103911615,0.086571875));
#31750=CARTESIAN_POINT('',(-0.012882,0.0383094997618084,0.0867041666666667));
#31751=CARTESIAN_POINT('',(-0.0150252212587062,0.0395468891324554,0.0868364583333334));
#31752=CARTESIAN_POINT('',(-0.0175,0.0395468891324554,0.08696875));
#31753=CARTESIAN_POINT('',(-0.0199747787412939,0.0395468891324554,0.0871010416666667));
#31754=CARTESIAN_POINT('',(-0.022118,0.0383094997618084,0.0872333333333334));
#31755=CARTESIAN_POINT('',(-0.0242612212587062,0.0370721103911615,0.087365625));
#31756=CARTESIAN_POINT('',(-0.0254986106293531,0.0349288891324553,0.0874979166666667));
#31757=CARTESIAN_POINT('',(-0.0267360000000001,0.0327856678737492,0.0876302083333334));
#31758=CARTESIAN_POINT('',(-0.026736,0.0303108891324553,0.0877625));
#31759=CARTESIAN_POINT('',(-0.0267360000000001,0.0278361103911615,0.0878947916666667));
#31760=CARTESIAN_POINT('',(-0.0254986106293531,0.0256928891324554,0.0880270833333334));
#31761=CARTESIAN_POINT('',(-0.0242612212587062,0.0235496678737492,0.088159375));
#31762=CARTESIAN_POINT('',(-0.022118,0.0223122785031023,0.0882916666666667));
#31763=CARTESIAN_POINT('',(-0.0199747787412939,0.0210748891324554,0.0884239583333334));
#31764=CARTESIAN_POINT('',(-0.0175,0.0210748891324553,0.08855625));
#31765=CARTESIAN_POINT('',(-0.0150252212587062,0.0210748891324553,0.0886885416666667));
#31766=CARTESIAN_POINT('',(-0.012882,0.0223122785031023,0.0888208333333334));
#31767=CARTESIAN_POINT('',(-0.0107387787412939,0.0235496678737492,0.088953125));
#31768=CARTESIAN_POINT('',(-0.00950138937064697,0.0256928891324554,0.0890854166666667));
#31769=CARTESIAN_POINT('',(-0.00826400000000005,0.0278361103911615,0.0892177083333334));
#31770=CARTESIAN_POINT('',(-0.008264,0.0303108891324553,0.08935));
#31771=CARTESIAN_POINT('',(-0.00826400000000004,0.0327856678737492,0.0894822916666667));
#31772=CARTESIAN_POINT('',(-0.00950138937064697,0.0349288891324553,0.0896145833333333));
#31773=CARTESIAN_POINT('',(-0.0107387787412939,0.0370721103911615,0.0897468750000001));
#31774=CARTESIAN_POINT('',(-0.012882,0.0383094997618084,0.0898791666666667));
#31775=CARTESIAN_POINT('',(-0.0150252212587062,0.0395468891324554,0.0900114583333334));
#31776=CARTESIAN_POINT('',(-0.0175,0.0395468891324554,0.09014375));
#31777=CARTESIAN_POINT('',(-0.0199747787412939,0.0395468891324554,0.0902760416666667));
#31778=CARTESIAN_POINT('',(-0.022118,0.0383094997618084,0.0904083333333334));
#31779=CARTESIAN_POINT('',(-0.0242612212587062,0.0370721103911615,0.0905406250000001));
#31780=CARTESIAN_POINT('',(-0.0254986106293531,0.0349288891324553,0.0906729166666667));
#31781=CARTESIAN_POINT('',(-0.0267360000000001,0.0327856678737492,0.0908052083333334));
#31782=CARTESIAN_POINT('',(-0.026736,0.0303108891324553,0.0909375));
#31783=CARTESIAN_POINT('',(-0.00826400000000005,0.0303108891324554,0.0832047959597733));
#31784=CARTESIAN_POINT('',(-0.00826400000000005,0.0327856678737492,0.08333708762644));
#31785=CARTESIAN_POINT('',(-0.00950138937064697,0.0349288891324553,0.0834693792931066));
#31786=CARTESIAN_POINT('',(-0.0107387787412939,0.0370721103911615,0.0836016709597733));
#31787=CARTESIAN_POINT('',(-0.0128820000000001,0.0383094997618084,0.08373396262644));
#31788=CARTESIAN_POINT('',(-0.0150252212587062,0.0395468891324554,0.0838662542931067));
#31789=CARTESIAN_POINT('',(-0.0175000000000001,0.0395468891324553,0.0839985459597733));
#31790=CARTESIAN_POINT('',(-0.0199747787412939,0.0395468891324554,0.08413083762644));
#31791=CARTESIAN_POINT('',(-0.022118,0.0383094997618084,0.0842631292931066));
#31792=CARTESIAN_POINT('',(-0.0242612212587062,0.0370721103911614,0.0843954209597733));
#31793=CARTESIAN_POINT('',(-0.0254986106293531,0.0349288891324553,0.08452771262644));
#31794=CARTESIAN_POINT('',(-0.026736,0.0327856678737492,0.0846600042931067));
#31795=CARTESIAN_POINT('',(-0.026736,0.0303108891324554,0.0847922959597733));
#31796=CARTESIAN_POINT('',(-0.026736,0.0278361103911615,0.08492458762644));
#31797=CARTESIAN_POINT('',(-0.0254986106293531,0.0256928891324553,0.0850568792931066));
#31798=CARTESIAN_POINT('',(-0.0242612212587062,0.0235496678737492,0.0851891709597732));
#31799=CARTESIAN_POINT('',(-0.022118,0.0223122785031022,0.08532146262644));
#31800=CARTESIAN_POINT('',(-0.0199747787412939,0.0210748891324554,0.0854537542931067));
#31801=CARTESIAN_POINT('',(-0.0175000000000001,0.0210748891324553,0.0855860459597733));
#31802=CARTESIAN_POINT('',(-0.0150252212587062,0.0210748891324553,0.0857183376264399));
#31803=CARTESIAN_POINT('',(-0.0128820000000001,0.0223122785031022,0.0858506292931066));
#31804=CARTESIAN_POINT('',(-0.0107387787412939,0.0235496678737492,0.0859829209597734));
#31805=CARTESIAN_POINT('',(-0.00950138937064697,0.0256928891324553,0.08611521262644));
#31806=CARTESIAN_POINT('',(-0.00826400000000005,0.0278361103911615,0.0862475042931066));
#31807=CARTESIAN_POINT('',(-0.00826400000000005,0.0303108891324554,0.0863797959597733));
#31808=CARTESIAN_POINT('',(-0.00826400000000005,0.0327856678737492,0.08651208762644));
#31809=CARTESIAN_POINT('',(-0.00950138937064697,0.0349288891324553,0.0866443792931067));
#31810=CARTESIAN_POINT('',(-0.0107387787412939,0.0370721103911615,0.0867766709597732));
#31811=CARTESIAN_POINT('',(-0.0128820000000001,0.0383094997618084,0.08690896262644));
#31812=CARTESIAN_POINT('',(-0.0150252212587062,0.0395468891324554,0.0870412542931066));
#31813=CARTESIAN_POINT('',(-0.0175000000000001,0.0395468891324553,0.0871735459597733));
#31814=CARTESIAN_POINT('',(-0.0199747787412939,0.0395468891324554,0.08730583762644));
#31815=CARTESIAN_POINT('',(-0.022118,0.0383094997618084,0.0874381292931067));
#31816=CARTESIAN_POINT('',(-0.0242612212587062,0.0370721103911614,0.0875704209597733));
#31817=CARTESIAN_POINT('',(-0.0254986106293531,0.0349288891324553,0.08770271262644));
#31818=CARTESIAN_POINT('',(-0.026736,0.0327856678737492,0.0878350042931066));
#31819=CARTESIAN_POINT('',(-0.026736,0.0303108891324554,0.0879672959597733));
#31820=CARTESIAN_POINT('',(-0.026736,0.0278361103911615,0.0880995876264399));
#31821=CARTESIAN_POINT('',(-0.0254986106293531,0.0256928891324553,0.0882318792931067));
#31822=CARTESIAN_POINT('',(-0.0242612212587062,0.0235496678737492,0.0883641709597733));
#31823=CARTESIAN_POINT('',(-0.022118,0.0223122785031022,0.08849646262644));
#31824=CARTESIAN_POINT('',(-0.0199747787412939,0.0210748891324554,0.0886287542931066));
#31825=CARTESIAN_POINT('',(-0.0175000000000001,0.0210748891324553,0.0887610459597734));
#31826=CARTESIAN_POINT('',(-0.0150252212587062,0.0210748891324553,0.08889333762644));
#31827=CARTESIAN_POINT('',(-0.0128820000000001,0.0223122785031022,0.0890256292931067));
#31828=CARTESIAN_POINT('',(-0.0107387787412939,0.0235496678737492,0.0891579209597733));
#31829=CARTESIAN_POINT('',(-0.00950138937064697,0.0256928891324553,0.0892902126264399));
#31830=CARTESIAN_POINT('',(-0.00826400000000005,0.0278361103911615,0.0894225042931066));
#31831=CARTESIAN_POINT('',(-0.00826400000000005,0.0303108891324554,0.0895547959597733));
#31832=CARTESIAN_POINT('',(-0.00826400000000005,0.0327856678737492,0.08968708762644));
#31833=CARTESIAN_POINT('',(-0.00950138937064697,0.0349288891324553,0.0898193792931067));
#31834=CARTESIAN_POINT('',(-0.0107387787412939,0.0370721103911615,0.0899516709597733));
#31835=CARTESIAN_POINT('',(-0.0128820000000001,0.0383094997618084,0.09008396262644));
#31836=CARTESIAN_POINT('',(-0.0150252212587062,0.0395468891324554,0.0902162542931066));
#31837=CARTESIAN_POINT('',(-0.0175000000000001,0.0395468891324553,0.0903485459597733));
#31838=CARTESIAN_POINT('',(-0.0199747787412939,0.0395468891324554,0.09048083762644));
#31839=CARTESIAN_POINT('',(-0.022118,0.0383094997618084,0.0906131292931066));
#31840=CARTESIAN_POINT('',(-0.0242612212587062,0.0370721103911614,0.0907454209597733));
#31841=CARTESIAN_POINT('',(-0.0254986106293531,0.0349288891324553,0.0908777126264399));
#31842=CARTESIAN_POINT('',(-0.026736,0.0327856678737492,0.0910100042931066));
#31843=CARTESIAN_POINT('',(-0.026736,0.0303108891324554,0.0911422959597733));
#31844=CARTESIAN_POINT('',(-0.00834237202082059,0.0303108891324554,0.0833940027553488));
#31845=CARTESIAN_POINT('',(-0.00834237202082058,0.0327646681540611,0.0835262944220155));
#31846=CARTESIAN_POINT('',(-0.00956926153162349,0.0348897031220451,0.0836585860886822));
#31847=CARTESIAN_POINT('',(-0.0107961510424264,0.037014738090029,0.0837908777553489));
#31848=CARTESIAN_POINT('',(-0.0129211860104103,0.0382416276008319,0.0839231694220155));
#31849=CARTESIAN_POINT('',(-0.0150462209783942,0.0394685171116348,0.0840554610886822));
#31850=CARTESIAN_POINT('',(-0.0175000000000001,0.0394685171116348,0.0841877527553489));
#31851=CARTESIAN_POINT('',(-0.0199537790216058,0.0394685171116348,0.0843200444220155));
#31852=CARTESIAN_POINT('',(-0.0220788139895898,0.0382416276008319,0.0844523360886822));
#31853=CARTESIAN_POINT('',(-0.0242038489575737,0.037014738090029,0.0845846277553489));
#31854=CARTESIAN_POINT('',(-0.0254307384683766,0.0348897031220451,0.0847169194220155));
#31855=CARTESIAN_POINT('',(-0.0266576279791795,0.0327646681540611,0.0848492110886822));
#31856=CARTESIAN_POINT('',(-0.0266576279791795,0.0303108891324554,0.0849815027553489));
#31857=CARTESIAN_POINT('',(-0.0266576279791795,0.0278571101108495,0.0851137944220155));
#31858=CARTESIAN_POINT('',(-0.0254307384683766,0.0257320751428656,0.0852460860886822));
#31859=CARTESIAN_POINT('',(-0.0242038489575737,0.0236070401748817,0.0853783777553489));
#31860=CARTESIAN_POINT('',(-0.0220788139895898,0.0223801506640788,0.0855106694220155));
#31861=CARTESIAN_POINT('',(-0.0199537790216058,0.0211532611532759,0.0856429610886822));
#31862=CARTESIAN_POINT('',(-0.0175000000000001,0.0211532611532759,0.0857752527553489));
#31863=CARTESIAN_POINT('',(-0.0150462209783943,0.0211532611532759,0.0859075444220155));
#31864=CARTESIAN_POINT('',(-0.0129211860104103,0.0223801506640788,0.0860398360886822));
#31865=CARTESIAN_POINT('',(-0.0107961510424264,0.0236070401748817,0.0861721277553489));
#31866=CARTESIAN_POINT('',(-0.00956926153162349,0.0257320751428656,0.0863044194220156));
#31867=CARTESIAN_POINT('',(-0.00834237202082059,0.0278571101108495,0.0864367110886822));
#31868=CARTESIAN_POINT('',(-0.00834237202082059,0.0303108891324554,0.0865690027553489));
#31869=CARTESIAN_POINT('',(-0.00834237202082058,0.0327646681540611,0.0867012944220156));
#31870=CARTESIAN_POINT('',(-0.00956926153162349,0.0348897031220451,0.0868335860886822));
#31871=CARTESIAN_POINT('',(-0.0107961510424264,0.037014738090029,0.0869658777553489));
#31872=CARTESIAN_POINT('',(-0.0129211860104103,0.0382416276008319,0.0870981694220156));
#31873=CARTESIAN_POINT('',(-0.0150462209783942,0.0394685171116348,0.0872304610886822));
#31874=CARTESIAN_POINT('',(-0.0175000000000001,0.0394685171116348,0.0873627527553488));
#31875=CARTESIAN_POINT('',(-0.0199537790216058,0.0394685171116348,0.0874950444220156));
#31876=CARTESIAN_POINT('',(-0.0220788139895898,0.0382416276008319,0.0876273360886822));
#31877=CARTESIAN_POINT('',(-0.0242038489575737,0.037014738090029,0.0877596277553488));
#31878=CARTESIAN_POINT('',(-0.0254307384683766,0.0348897031220451,0.0878919194220156));
#31879=CARTESIAN_POINT('',(-0.0266576279791795,0.0327646681540611,0.0880242110886821));
#31880=CARTESIAN_POINT('',(-0.0266576279791795,0.0303108891324554,0.0881565027553489));
#31881=CARTESIAN_POINT('',(-0.0266576279791795,0.0278571101108495,0.0882887944220156));
#31882=CARTESIAN_POINT('',(-0.0254307384683766,0.0257320751428656,0.0884210860886821));
#31883=CARTESIAN_POINT('',(-0.0242038489575737,0.0236070401748817,0.0885533777553488));
#31884=CARTESIAN_POINT('',(-0.0220788139895898,0.0223801506640788,0.0886856694220155));
#31885=CARTESIAN_POINT('',(-0.0199537790216058,0.0211532611532759,0.0888179610886821));
#31886=CARTESIAN_POINT('',(-0.0175000000000001,0.0211532611532759,0.0889502527553488));
#31887=CARTESIAN_POINT('',(-0.0150462209783943,0.0211532611532759,0.0890825444220155));
#31888=CARTESIAN_POINT('',(-0.0129211860104103,0.0223801506640788,0.0892148360886822));
#31889=CARTESIAN_POINT('',(-0.0107961510424264,0.0236070401748817,0.0893471277553488));
#31890=CARTESIAN_POINT('',(-0.00956926153162349,0.0257320751428656,0.0894794194220155));
#31891=CARTESIAN_POINT('',(-0.00834237202082059,0.0278571101108495,0.0896117110886821));
#31892=CARTESIAN_POINT('',(-0.00834237202082059,0.0303108891324554,0.0897440027553488));
#31893=CARTESIAN_POINT('',(-0.00834237202082058,0.0327646681540611,0.0898762944220156));
#31894=CARTESIAN_POINT('',(-0.00956926153162349,0.0348897031220451,0.0900085860886822));
#31895=CARTESIAN_POINT('',(-0.0107961510424264,0.037014738090029,0.0901408777553488));
#31896=CARTESIAN_POINT('',(-0.0129211860104103,0.0382416276008319,0.0902731694220155));
#31897=CARTESIAN_POINT('',(-0.0150462209783942,0.0394685171116348,0.0904054610886822));
#31898=CARTESIAN_POINT('',(-0.0175000000000001,0.0394685171116348,0.0905377527553489));
#31899=CARTESIAN_POINT('',(-0.0199537790216058,0.0394685171116348,0.0906700444220155));
#31900=CARTESIAN_POINT('',(-0.0220788139895898,0.0382416276008319,0.0908023360886822));
#31901=CARTESIAN_POINT('',(-0.0242038489575737,0.037014738090029,0.0909346277553488));
#31902=CARTESIAN_POINT('',(-0.0254307384683766,0.0348897031220451,0.0910669194220155));
#31903=CARTESIAN_POINT('',(-0.0266576279791795,0.0327646681540611,0.0911992110886822));
#31904=CARTESIAN_POINT('',(-0.0266576279791795,0.0303108891324554,0.0913315027553488));
#31905=CARTESIAN_POINT('',(-0.0084871846327359,0.0303108891324553,0.0835388153672642));
#31906=CARTESIAN_POINT('',(-0.0084871846327359,0.0327258657316446,0.0836711070339308));
#31907=CARTESIAN_POINT('',(-0.00969467293233051,0.0348172968160874,0.0838033987005975));
#31908=CARTESIAN_POINT('',(-0.0109021612319251,0.0369087279005302,0.0839356903672642));
#31909=CARTESIAN_POINT('',(-0.012993592316368,0.0381162162001248,0.0840679820339308));
#31910=CARTESIAN_POINT('',(-0.0150850234008108,0.0393237044997195,0.0842002737005975));
#31911=CARTESIAN_POINT('',(-0.0175,0.0393237044997195,0.0843325653672642));
#31912=CARTESIAN_POINT('',(-0.0199149765991893,0.0393237044997195,0.0844648570339309));
#31913=CARTESIAN_POINT('',(-0.0220064076836321,0.0381162162001248,0.0845971487005975));
#31914=CARTESIAN_POINT('',(-0.024097838768075,0.0369087279005303,0.0847294403672642));
#31915=CARTESIAN_POINT('',(-0.0253053270676696,0.0348172968160874,0.0848617320339308));
#31916=CARTESIAN_POINT('',(-0.0265128153672642,0.0327258657316446,0.0849940237005975));
#31917=CARTESIAN_POINT('',(-0.0265128153672642,0.0303108891324553,0.0851263153672642));
#31918=CARTESIAN_POINT('',(-0.0265128153672642,0.0278959125332661,0.0852586070339309));
#31919=CARTESIAN_POINT('',(-0.0253053270676696,0.0258044814488233,0.0853908987005975));
#31920=CARTESIAN_POINT('',(-0.024097838768075,0.0237130503643804,0.0855231903672642));
#31921=CARTESIAN_POINT('',(-0.0220064076836321,0.0225055620647858,0.0856554820339308));
#31922=CARTESIAN_POINT('',(-0.0199149765991893,0.0212980737651912,0.0857877737005975));
#31923=CARTESIAN_POINT('',(-0.0175,0.0212980737651912,0.0859200653672642));
#31924=CARTESIAN_POINT('',(-0.0150850234008108,0.0212980737651912,0.0860523570339309));
#31925=CARTESIAN_POINT('',(-0.012993592316368,0.0225055620647858,0.0861846487005975));
#31926=CARTESIAN_POINT('',(-0.0109021612319251,0.0237130503643804,0.0863169403672642));
#31927=CARTESIAN_POINT('',(-0.00969467293233052,0.0258044814488233,0.0864492320339308));
#31928=CARTESIAN_POINT('',(-0.0084871846327359,0.0278959125332661,0.0865815237005975));
#31929=CARTESIAN_POINT('',(-0.0084871846327359,0.0303108891324553,0.0867138153672642));
#31930=CARTESIAN_POINT('',(-0.0084871846327359,0.0327258657316446,0.0868461070339309));
#31931=CARTESIAN_POINT('',(-0.00969467293233051,0.0348172968160874,0.0869783987005975));
#31932=CARTESIAN_POINT('',(-0.0109021612319251,0.0369087279005302,0.0871106903672642));
#31933=CARTESIAN_POINT('',(-0.012993592316368,0.0381162162001248,0.0872429820339308));
#31934=CARTESIAN_POINT('',(-0.0150850234008108,0.0393237044997195,0.0873752737005975));
#31935=CARTESIAN_POINT('',(-0.0175,0.0393237044997195,0.0875075653672642));
#31936=CARTESIAN_POINT('',(-0.0199149765991893,0.0393237044997195,0.0876398570339308));
#31937=CARTESIAN_POINT('',(-0.0220064076836321,0.0381162162001248,0.0877721487005975));
#31938=CARTESIAN_POINT('',(-0.024097838768075,0.0369087279005303,0.0879044403672642));
#31939=CARTESIAN_POINT('',(-0.0253053270676696,0.0348172968160874,0.0880367320339308));
#31940=CARTESIAN_POINT('',(-0.0265128153672642,0.0327258657316446,0.0881690237005976));
#31941=CARTESIAN_POINT('',(-0.0265128153672642,0.0303108891324553,0.0883013153672642));
#31942=CARTESIAN_POINT('',(-0.0265128153672642,0.0278959125332661,0.0884336070339309));
#31943=CARTESIAN_POINT('',(-0.0253053270676696,0.0258044814488233,0.0885658987005975));
#31944=CARTESIAN_POINT('',(-0.024097838768075,0.0237130503643804,0.0886981903672642));
#31945=CARTESIAN_POINT('',(-0.0220064076836321,0.0225055620647858,0.0888304820339308));
#31946=CARTESIAN_POINT('',(-0.0199149765991893,0.0212980737651912,0.0889627737005975));
#31947=CARTESIAN_POINT('',(-0.0175,0.0212980737651912,0.0890950653672642));
#31948=CARTESIAN_POINT('',(-0.0150850234008108,0.0212980737651912,0.0892273570339309));
#31949=CARTESIAN_POINT('',(-0.012993592316368,0.0225055620647858,0.0893596487005975));
#31950=CARTESIAN_POINT('',(-0.0109021612319251,0.0237130503643804,0.0894919403672642));
#31951=CARTESIAN_POINT('',(-0.00969467293233052,0.0258044814488233,0.0896242320339308));
#31952=CARTESIAN_POINT('',(-0.0084871846327359,0.0278959125332661,0.0897565237005975));
#31953=CARTESIAN_POINT('',(-0.0084871846327359,0.0303108891324553,0.0898888153672642));
#31954=CARTESIAN_POINT('',(-0.0084871846327359,0.0327258657316446,0.0900211070339309));
#31955=CARTESIAN_POINT('',(-0.00969467293233051,0.0348172968160874,0.0901533987005975));
#31956=CARTESIAN_POINT('',(-0.0109021612319251,0.0369087279005302,0.0902856903672642));
#31957=CARTESIAN_POINT('',(-0.012993592316368,0.0381162162001248,0.0904179820339308));
#31958=CARTESIAN_POINT('',(-0.0150850234008108,0.0393237044997195,0.0905502737005975));
#31959=CARTESIAN_POINT('',(-0.0175,0.0393237044997195,0.0906825653672642));
#31960=CARTESIAN_POINT('',(-0.0199149765991893,0.0393237044997195,0.0908148570339309));
#31961=CARTESIAN_POINT('',(-0.0220064076836321,0.0381162162001248,0.0909471487005975));
#31962=CARTESIAN_POINT('',(-0.024097838768075,0.0369087279005303,0.0910794403672642));
#31963=CARTESIAN_POINT('',(-0.0253053270676696,0.0348172968160874,0.0912117320339308));
#31964=CARTESIAN_POINT('',(-0.0265128153672642,0.0327258657316446,0.0913440237005975));
#31965=CARTESIAN_POINT('',(-0.0265128153672642,0.0303108891324553,0.0914763153672642));
#31966=CARTESIAN_POINT('',(-0.009026,0.0303108891324553,0.083));
#31967=CARTESIAN_POINT('',(-0.008264,0.0303108891324553,0.083));
#31968=CARTESIAN_POINT('',(-0.0084871846327359,0.0303108891324553,0.0835388153672642));
#31969=CARTESIAN_POINT('',(-0.0084871846327359,0.0303108891324553,0.0835388153672642));
#31970=CARTESIAN_POINT('',(-0.0084871846327359,0.0327258657316446,0.0836711070339308));
#31971=CARTESIAN_POINT('',(-0.00969467293233051,0.0348172968160874,0.0838033987005975));
#31972=CARTESIAN_POINT('',(-0.0109021612319251,0.0369087279005302,0.0839356903672642));
#31973=CARTESIAN_POINT('',(-0.012993592316368,0.0381162162001248,0.0840679820339308));
#31974=CARTESIAN_POINT('',(-0.0150850234008108,0.0393237044997195,0.0842002737005975));
#31975=CARTESIAN_POINT('',(-0.0175,0.0393237044997195,0.0843325653672642));
#31976=CARTESIAN_POINT('',(-0.0199149765991893,0.0393237044997195,0.0844648570339309));
#31977=CARTESIAN_POINT('',(-0.0220064076836321,0.0381162162001248,0.0845971487005975));
#31978=CARTESIAN_POINT('',(-0.024097838768075,0.0369087279005303,0.0847294403672642));
#31979=CARTESIAN_POINT('',(-0.0253053270676696,0.0348172968160874,0.0848617320339308));
#31980=CARTESIAN_POINT('',(-0.0265128153672642,0.0327258657316446,0.0849940237005975));
#31981=CARTESIAN_POINT('',(-0.0265128153672642,0.0303108891324553,0.0851263153672642));
#31982=CARTESIAN_POINT('',(-0.0265128153672642,0.0278959125332661,0.0852586070339309));
#31983=CARTESIAN_POINT('',(-0.0253053270676696,0.0258044814488233,0.0853908987005975));
#31984=CARTESIAN_POINT('',(-0.024097838768075,0.0237130503643804,0.0855231903672642));
#31985=CARTESIAN_POINT('',(-0.0220064076836321,0.0225055620647858,0.0856554820339308));
#31986=CARTESIAN_POINT('',(-0.0199149765991893,0.0212980737651912,0.0857877737005975));
#31987=CARTESIAN_POINT('',(-0.0175,0.0212980737651912,0.0859200653672642));
#31988=CARTESIAN_POINT('',(-0.0150850234008108,0.0212980737651912,0.0860523570339309));
#31989=CARTESIAN_POINT('',(-0.012993592316368,0.0225055620647858,0.0861846487005975));
#31990=CARTESIAN_POINT('',(-0.0109021612319251,0.0237130503643804,0.0863169403672642));
#31991=CARTESIAN_POINT('',(-0.00969467293233052,0.0258044814488233,0.0864492320339308));
#31992=CARTESIAN_POINT('',(-0.00848718463273591,0.0278959125332661,0.0865815237005975));
#31993=CARTESIAN_POINT('',(-0.0084871846327359,0.0303108891324553,0.0867138153672642));
#31994=CARTESIAN_POINT('',(-0.0084871846327359,0.0327258657316446,0.0868461070339309));
#31995=CARTESIAN_POINT('',(-0.00969467293233051,0.0348172968160874,0.0869783987005975));
#31996=CARTESIAN_POINT('',(-0.0109021612319251,0.0369087279005302,0.0871106903672642));
#31997=CARTESIAN_POINT('',(-0.012993592316368,0.0381162162001248,0.0872429820339308));
#31998=CARTESIAN_POINT('',(-0.0150850234008108,0.0393237044997195,0.0873752737005975));
#31999=CARTESIAN_POINT('',(-0.0175,0.0393237044997195,0.0875075653672642));
#32000=CARTESIAN_POINT('',(-0.0199149765991893,0.0393237044997195,0.0876398570339309));
#32001=CARTESIAN_POINT('',(-0.0220064076836321,0.0381162162001248,0.0877721487005975));
#32002=CARTESIAN_POINT('',(-0.024097838768075,0.0369087279005303,0.0879044403672641));
#32003=CARTESIAN_POINT('',(-0.0253053270676696,0.0348172968160874,0.0880367320339308));
#32004=CARTESIAN_POINT('',(-0.0265128153672642,0.0327258657316446,0.0881690237005976));
#32005=CARTESIAN_POINT('',(-0.0265128153672642,0.0303108891324553,0.0883013153672642));
#32006=CARTESIAN_POINT('',(-0.0265128153672642,0.0278959125332661,0.0884336070339309));
#32007=CARTESIAN_POINT('',(-0.0253053270676696,0.0258044814488233,0.0885658987005975));
#32008=CARTESIAN_POINT('',(-0.024097838768075,0.0237130503643804,0.0886981903672642));
#32009=CARTESIAN_POINT('',(-0.0220064076836321,0.0225055620647858,0.0888304820339308));
#32010=CARTESIAN_POINT('',(-0.0199149765991893,0.0212980737651912,0.0889627737005975));
#32011=CARTESIAN_POINT('',(-0.0175,0.0212980737651912,0.0890950653672642));
#32012=CARTESIAN_POINT('',(-0.0150850234008108,0.0212980737651912,0.0892273570339309));
#32013=CARTESIAN_POINT('',(-0.012993592316368,0.0225055620647858,0.0893596487005975));
#32014=CARTESIAN_POINT('',(-0.0109021612319251,0.0237130503643804,0.0894919403672642));
#32015=CARTESIAN_POINT('',(-0.00969467293233052,0.0258044814488233,0.0896242320339308));
#32016=CARTESIAN_POINT('',(-0.00848718463273591,0.0278959125332661,0.0897565237005975));
#32017=CARTESIAN_POINT('',(-0.0084871846327359,0.0303108891324553,0.0898888153672642));
#32018=CARTESIAN_POINT('',(-0.0084871846327359,0.0327258657316446,0.0900211070339309));
#32019=CARTESIAN_POINT('',(-0.00969467293233051,0.0348172968160874,0.0901533987005975));
#32020=CARTESIAN_POINT('',(-0.0109021612319251,0.0369087279005302,0.0902856903672642));
#32021=CARTESIAN_POINT('',(-0.012993592316368,0.0381162162001248,0.0904179820339308));
#32022=CARTESIAN_POINT('',(-0.0150850234008108,0.0393237044997195,0.0905502737005975));
#32023=CARTESIAN_POINT('',(-0.0175,0.0393237044997195,0.0906825653672642));
#32024=CARTESIAN_POINT('',(-0.0199149765991893,0.0393237044997195,0.0908148570339309));
#32025=CARTESIAN_POINT('',(-0.0220064076836321,0.0381162162001248,0.0909471487005975));
#32026=CARTESIAN_POINT('',(-0.024097838768075,0.0369087279005303,0.0910794403672642));
#32027=CARTESIAN_POINT('',(-0.0253053270676696,0.0348172968160874,0.0912117320339308));
#32028=CARTESIAN_POINT('',(-0.0265128153672642,0.0327258657316446,0.0913440237005975));
#32029=CARTESIAN_POINT('',(-0.0265128153672642,0.0303108891324553,0.0914763153672642));
#32030=CARTESIAN_POINT('',(-0.0265128153672642,0.0303108891324553,0.0914763153672642));
#32031=CARTESIAN_POINT('',(-0.025974,0.0303108891324553,0.0909375));
#32032=CARTESIAN_POINT('',(-0.026736,0.0303108891324553,0.0909375));
#32033=CARTESIAN_POINT('',(-0.008264,0.0303108891324553,0.08935));
#32034=CARTESIAN_POINT('',(-0.00826400000000002,0.0327856678737492,0.0894822916666667));
#32035=CARTESIAN_POINT('',(-0.00950138937064697,0.0349288891324553,0.0896145833333333));
#32036=CARTESIAN_POINT('',(-0.0107387787412939,0.0370721103911615,0.0897468750000001));
#32037=CARTESIAN_POINT('',(-0.012882,0.0383094997618084,0.0898791666666667));
#32038=CARTESIAN_POINT('',(-0.0150252212587062,0.0395468891324554,0.0900114583333334));
#32039=CARTESIAN_POINT('',(-0.0175,0.0395468891324554,0.09014375));
#32040=CARTESIAN_POINT('',(-0.0199747787412939,0.0395468891324554,0.0902760416666667));
#32041=CARTESIAN_POINT('',(-0.022118,0.0383094997618084,0.0904083333333334));
#32042=CARTESIAN_POINT('',(-0.0242612212587062,0.0370721103911615,0.0905406250000001));
#32043=CARTESIAN_POINT('',(-0.0254986106293531,0.0349288891324553,0.0906729166666667));
#32044=CARTESIAN_POINT('',(-0.0267360000000001,0.0327856678737492,0.0908052083333334));
#32045=CARTESIAN_POINT('',(-0.026736,0.0303108891324553,0.0909375));
#32046=CARTESIAN_POINT('',(-0.008264,0.0303108891324553,0.08935));
#32047=CARTESIAN_POINT('',(-0.026736,0.0303108891324553,0.0877625));
#32048=CARTESIAN_POINT('',(-0.0267360000000001,0.0278361103911614,0.0878947916666667));
#32049=CARTESIAN_POINT('',(-0.0254986106293531,0.0256928891324554,0.0880270833333334));
#32050=CARTESIAN_POINT('',(-0.0242612212587062,0.0235496678737492,0.088159375));
#32051=CARTESIAN_POINT('',(-0.022118,0.0223122785031023,0.0882916666666667));
#32052=CARTESIAN_POINT('',(-0.0199747787412939,0.0210748891324553,0.0884239583333334));
#32053=CARTESIAN_POINT('',(-0.0175,0.0210748891324553,0.08855625));
#32054=CARTESIAN_POINT('',(-0.0150252212587062,0.0210748891324553,0.0886885416666667));
#32055=CARTESIAN_POINT('',(-0.012882,0.0223122785031023,0.0888208333333334));
#32056=CARTESIAN_POINT('',(-0.0107387787412939,0.0235496678737492,0.088953125));
#32057=CARTESIAN_POINT('',(-0.00950138937064697,0.0256928891324554,0.0890854166666667));
#32058=CARTESIAN_POINT('',(-0.00826400000000006,0.0278361103911614,0.0892177083333334));
#32059=CARTESIAN_POINT('',(-0.008264,0.0303108891324553,0.08935));
#32060=CARTESIAN_POINT('',(-0.026736,0.0303108891324553,0.0877625));
#32061=CARTESIAN_POINT('',(-0.008264,0.0303108891324553,0.086175));
#32062=CARTESIAN_POINT('',(-0.00826400000000003,0.0327856678737492,0.0863072916666667));
#32063=CARTESIAN_POINT('',(-0.00950138937064697,0.0349288891324553,0.0864395833333334));
#32064=CARTESIAN_POINT('',(-0.0107387787412939,0.0370721103911615,0.086571875));
#32065=CARTESIAN_POINT('',(-0.012882,0.0383094997618084,0.0867041666666667));
#32066=CARTESIAN_POINT('',(-0.0150252212587062,0.0395468891324554,0.0868364583333334));
#32067=CARTESIAN_POINT('',(-0.0175,0.0395468891324554,0.08696875));
#32068=CARTESIAN_POINT('',(-0.0199747787412939,0.0395468891324554,0.0871010416666667));
#32069=CARTESIAN_POINT('',(-0.022118,0.0383094997618084,0.0872333333333334));
#32070=CARTESIAN_POINT('',(-0.0242612212587062,0.0370721103911615,0.087365625));
#32071=CARTESIAN_POINT('',(-0.0254986106293531,0.0349288891324553,0.0874979166666667));
#32072=CARTESIAN_POINT('',(-0.0267360000000001,0.0327856678737492,0.0876302083333333));
#32073=CARTESIAN_POINT('',(-0.026736,0.0303108891324553,0.0877625));
#32074=CARTESIAN_POINT('',(-0.008264,0.0303108891324553,0.086175));
#32075=CARTESIAN_POINT('',(-0.026736,0.0303108891324553,0.0845875));
#32076=CARTESIAN_POINT('',(-0.0267360000000001,0.0278361103911614,0.0847197916666667));
#32077=CARTESIAN_POINT('',(-0.0254986106293531,0.0256928891324554,0.0848520833333334));
#32078=CARTESIAN_POINT('',(-0.0242612212587062,0.0235496678737492,0.0849843750000001));
#32079=CARTESIAN_POINT('',(-0.022118,0.0223122785031023,0.0851166666666667));
#32080=CARTESIAN_POINT('',(-0.0199747787412939,0.0210748891324553,0.0852489583333334));
#32081=CARTESIAN_POINT('',(-0.0175,0.0210748891324553,0.08538125));
#32082=CARTESIAN_POINT('',(-0.0150252212587062,0.0210748891324553,0.0855135416666667));
#32083=CARTESIAN_POINT('',(-0.012882,0.0223122785031023,0.0856458333333334));
#32084=CARTESIAN_POINT('',(-0.0107387787412939,0.0235496678737492,0.0857781250000001));
#32085=CARTESIAN_POINT('',(-0.00950138937064697,0.0256928891324554,0.0859104166666667));
#32086=CARTESIAN_POINT('',(-0.00826400000000006,0.0278361103911614,0.0860427083333333));
#32087=CARTESIAN_POINT('',(-0.008264,0.0303108891324553,0.086175));
#32088=CARTESIAN_POINT('',(-0.026736,0.0303108891324553,0.0845875));
#32089=CARTESIAN_POINT('',(-0.008264,0.0303108891324553,0.083));
#32090=CARTESIAN_POINT('',(-0.00826400000000004,0.0327856678737492,0.0831322916666668));
#32091=CARTESIAN_POINT('',(-0.00950138937064697,0.0349288891324553,0.0832645833333334));
#32092=CARTESIAN_POINT('',(-0.0107387787412939,0.0370721103911615,0.0833968750000001));
#32093=CARTESIAN_POINT('',(-0.012882,0.0383094997618084,0.0835291666666667));
#32094=CARTESIAN_POINT('',(-0.0150252212587062,0.0395468891324554,0.0836614583333334));
#32095=CARTESIAN_POINT('',(-0.0175,0.0395468891324554,0.08379375));
#32096=CARTESIAN_POINT('',(-0.0199747787412939,0.0395468891324554,0.0839260416666667));
#32097=CARTESIAN_POINT('',(-0.022118,0.0383094997618084,0.0840583333333334));
#32098=CARTESIAN_POINT('',(-0.0242612212587062,0.0370721103911615,0.084190625));
#32099=CARTESIAN_POINT('',(-0.0254986106293531,0.0349288891324553,0.0843229166666667));
#32100=CARTESIAN_POINT('',(-0.0267360000000001,0.0327856678737491,0.0844552083333334));
#32101=CARTESIAN_POINT('',(-0.026736,0.0303108891324553,0.0845875));
#32102=CARTESIAN_POINT('',(-0.0084871846327359,0.0303108891324553,0.0835388153672642));
#32103=CARTESIAN_POINT('',(-0.0084871846327359,0.0327258657316446,0.0836711070339308));
#32104=CARTESIAN_POINT('',(-0.00969467293233052,0.0348172968160874,0.0838033987005975));
#32105=CARTESIAN_POINT('',(-0.0109021612319251,0.0369087279005302,0.0839356903672642));
#32106=CARTESIAN_POINT('',(-0.012993592316368,0.0381162162001248,0.0840679820339308));
#32107=CARTESIAN_POINT('',(-0.0150850234008108,0.0393237044997195,0.0842002737005975));
#32108=CARTESIAN_POINT('',(-0.0175,0.0393237044997195,0.0843325653672642));
#32109=CARTESIAN_POINT('',(-0.0199149765991893,0.0393237044997195,0.0844648570339309));
#32110=CARTESIAN_POINT('',(-0.0220064076836321,0.0381162162001248,0.0845971487005975));
#32111=CARTESIAN_POINT('',(-0.024097838768075,0.0369087279005302,0.0847294403672642));
#32112=CARTESIAN_POINT('',(-0.0253053270676696,0.0348172968160874,0.0848617320339308));
#32113=CARTESIAN_POINT('',(-0.0265128153672642,0.0327258657316446,0.0849940237005975));
#32114=CARTESIAN_POINT('',(-0.0265128153672642,0.0303108891324553,0.0851263153672642));
#32115=CARTESIAN_POINT('',(-0.0265128153672642,0.0278959125332661,0.0852586070339309));
#32116=CARTESIAN_POINT('',(-0.0253053270676696,0.0258044814488233,0.0853908987005975));
#32117=CARTESIAN_POINT('',(-0.024097838768075,0.0237130503643804,0.0855231903672642));
#32118=CARTESIAN_POINT('',(-0.0220064076836321,0.0225055620647858,0.0856554820339308));
#32119=CARTESIAN_POINT('',(-0.0199149765991893,0.0212980737651912,0.0857877737005975));
#32120=CARTESIAN_POINT('',(-0.0175,0.0212980737651912,0.0859200653672642));
#32121=CARTESIAN_POINT('',(-0.0150850234008108,0.0212980737651912,0.0860523570339309));
#32122=CARTESIAN_POINT('',(-0.012993592316368,0.0225055620647858,0.0861846487005975));
#32123=CARTESIAN_POINT('',(-0.0109021612319251,0.0237130503643804,0.0863169403672642));
#32124=CARTESIAN_POINT('',(-0.00969467293233052,0.0258044814488233,0.0864492320339308));
#32125=CARTESIAN_POINT('',(-0.0084871846327359,0.0278959125332661,0.0865815237005975));
#32126=CARTESIAN_POINT('',(-0.0084871846327359,0.0303108891324553,0.0867138153672642));
#32127=CARTESIAN_POINT('',(-0.0084871846327359,0.0327258657316446,0.0868461070339309));
#32128=CARTESIAN_POINT('',(-0.00969467293233052,0.0348172968160874,0.0869783987005975));
#32129=CARTESIAN_POINT('',(-0.0109021612319251,0.0369087279005302,0.0871106903672642));
#32130=CARTESIAN_POINT('',(-0.012993592316368,0.0381162162001248,0.0872429820339308));
#32131=CARTESIAN_POINT('',(-0.0150850234008108,0.0393237044997195,0.0873752737005975));
#32132=CARTESIAN_POINT('',(-0.0175,0.0393237044997195,0.0875075653672642));
#32133=CARTESIAN_POINT('',(-0.0199149765991893,0.0393237044997195,0.0876398570339308));
#32134=CARTESIAN_POINT('',(-0.0220064076836321,0.0381162162001248,0.0877721487005975));
#32135=CARTESIAN_POINT('',(-0.024097838768075,0.0369087279005302,0.0879044403672642));
#32136=CARTESIAN_POINT('',(-0.0253053270676696,0.0348172968160874,0.0880367320339308));
#32137=CARTESIAN_POINT('',(-0.0265128153672642,0.0327258657316446,0.0881690237005976));
#32138=CARTESIAN_POINT('',(-0.0265128153672642,0.0303108891324553,0.0883013153672642));
#32139=CARTESIAN_POINT('',(-0.0265128153672642,0.0278959125332661,0.0884336070339309));
#32140=CARTESIAN_POINT('',(-0.0253053270676696,0.0258044814488233,0.0885658987005975));
#32141=CARTESIAN_POINT('',(-0.024097838768075,0.0237130503643804,0.0886981903672642));
#32142=CARTESIAN_POINT('',(-0.0220064076836321,0.0225055620647858,0.0888304820339308));
#32143=CARTESIAN_POINT('',(-0.0199149765991893,0.0212980737651912,0.0889627737005975));
#32144=CARTESIAN_POINT('',(-0.0175,0.0212980737651912,0.0890950653672642));
#32145=CARTESIAN_POINT('',(-0.0150850234008108,0.0212980737651912,0.0892273570339309));
#32146=CARTESIAN_POINT('',(-0.012993592316368,0.0225055620647858,0.0893596487005975));
#32147=CARTESIAN_POINT('',(-0.0109021612319251,0.0237130503643804,0.0894919403672642));
#32148=CARTESIAN_POINT('',(-0.00969467293233052,0.0258044814488233,0.0896242320339308));
#32149=CARTESIAN_POINT('',(-0.0084871846327359,0.0278959125332661,0.0897565237005975));
#32150=CARTESIAN_POINT('',(-0.0084871846327359,0.0303108891324553,0.0898888153672642));
#32151=CARTESIAN_POINT('',(-0.0084871846327359,0.0327258657316446,0.0900211070339309));
#32152=CARTESIAN_POINT('',(-0.00969467293233052,0.0348172968160874,0.0901533987005975));
#32153=CARTESIAN_POINT('',(-0.0109021612319251,0.0369087279005302,0.0902856903672642));
#32154=CARTESIAN_POINT('',(-0.012993592316368,0.0381162162001248,0.0904179820339308));
#32155=CARTESIAN_POINT('',(-0.0150850234008108,0.0393237044997195,0.0905502737005975));
#32156=CARTESIAN_POINT('',(-0.0175,0.0393237044997195,0.0906825653672642));
#32157=CARTESIAN_POINT('',(-0.0199149765991893,0.0393237044997195,0.0908148570339309));
#32158=CARTESIAN_POINT('',(-0.0220064076836321,0.0381162162001248,0.0909471487005975));
#32159=CARTESIAN_POINT('',(-0.024097838768075,0.0369087279005302,0.0910794403672642));
#32160=CARTESIAN_POINT('',(-0.0253053270676696,0.0348172968160874,0.0912117320339308));
#32161=CARTESIAN_POINT('',(-0.0265128153672642,0.0327258657316446,0.0913440237005975));
#32162=CARTESIAN_POINT('',(-0.0265128153672642,0.0303108891324553,0.0914763153672642));
#32163=CARTESIAN_POINT('',(-0.00910761536726419,0.0303108891324553,0.0841592461017925));
#32164=CARTESIAN_POINT('',(-0.00910761536726418,0.0325596218173683,0.0842915377684592));
#32165=CARTESIAN_POINT('',(-0.0102319817097207,0.0345070814488233,0.0844238294351258));
#32166=CARTESIAN_POINT('',(-0.0113563480521771,0.0364545410802783,0.0845561211017925));
#32167=CARTESIAN_POINT('',(-0.0133038076836321,0.0375789074227347,0.0846884127684591));
#32168=CARTESIAN_POINT('',(-0.0152512673150871,0.0387032737651912,0.0848207044351258));
#32169=CARTESIAN_POINT('',(-0.0175,0.0387032737651912,0.0849529961017925));
#32170=CARTESIAN_POINT('',(-0.019748732684913,0.0387032737651912,0.0850852877684591));
#32171=CARTESIAN_POINT('',(-0.0216961923163679,0.0375789074227348,0.0852175794351258));
#32172=CARTESIAN_POINT('',(-0.023643651947823,0.0364545410802783,0.0853498711017925));
#32173=CARTESIAN_POINT('',(-0.0247680182902794,0.0345070814488233,0.0854821627684591));
#32174=CARTESIAN_POINT('',(-0.0258923846327359,0.0325596218173683,0.0856144544351258));
#32175=CARTESIAN_POINT('',(-0.0258923846327359,0.0303108891324553,0.0857467461017925));
#32176=CARTESIAN_POINT('',(-0.0258923846327359,0.0280621564475424,0.0858790377684592));
#32177=CARTESIAN_POINT('',(-0.0247680182902794,0.0261146968160874,0.0860113294351258));
#32178=CARTESIAN_POINT('',(-0.023643651947823,0.0241672371846324,0.0861436211017925));
#32179=CARTESIAN_POINT('',(-0.021696192316368,0.023042870842176,0.0862759127684591));
#32180=CARTESIAN_POINT('',(-0.019748732684913,0.0219185044997195,0.0864082044351258));
#32181=CARTESIAN_POINT('',(-0.0175,0.0219185044997195,0.0865404961017925));
#32182=CARTESIAN_POINT('',(-0.0152512673150871,0.0219185044997195,0.0866727877684591));
#32183=CARTESIAN_POINT('',(-0.0133038076836321,0.023042870842176,0.0868050794351258));
#32184=CARTESIAN_POINT('',(-0.0113563480521771,0.0241672371846324,0.0869373711017925));
#32185=CARTESIAN_POINT('',(-0.0102319817097207,0.0261146968160874,0.0870696627684591));
#32186=CARTESIAN_POINT('',(-0.00910761536726419,0.0280621564475424,0.0872019544351259));
#32187=CARTESIAN_POINT('',(-0.00910761536726419,0.0303108891324553,0.0873342461017925));
#32188=CARTESIAN_POINT('',(-0.00910761536726418,0.0325596218173683,0.0874665377684592));
#32189=CARTESIAN_POINT('',(-0.0102319817097207,0.0345070814488233,0.0875988294351258));
#32190=CARTESIAN_POINT('',(-0.0113563480521771,0.0364545410802783,0.0877311211017925));
#32191=CARTESIAN_POINT('',(-0.0133038076836321,0.0375789074227347,0.0878634127684591));
#32192=CARTESIAN_POINT('',(-0.0152512673150871,0.0387032737651912,0.0879957044351258));
#32193=CARTESIAN_POINT('',(-0.0175,0.0387032737651912,0.0881279961017925));
#32194=CARTESIAN_POINT('',(-0.019748732684913,0.0387032737651912,0.0882602877684591));
#32195=CARTESIAN_POINT('',(-0.0216961923163679,0.0375789074227348,0.0883925794351258));
#32196=CARTESIAN_POINT('',(-0.023643651947823,0.0364545410802783,0.0885248711017924));
#32197=CARTESIAN_POINT('',(-0.0247680182902794,0.0345070814488233,0.0886571627684591));
#32198=CARTESIAN_POINT('',(-0.0258923846327359,0.0325596218173683,0.0887894544351258));
#32199=CARTESIAN_POINT('',(-0.0258923846327359,0.0303108891324553,0.0889217461017925));
#32200=CARTESIAN_POINT('',(-0.0258923846327359,0.0280621564475424,0.0890540377684592));
#32201=CARTESIAN_POINT('',(-0.0247680182902794,0.0261146968160874,0.0891863294351258));
#32202=CARTESIAN_POINT('',(-0.023643651947823,0.0241672371846324,0.0893186211017925));
#32203=CARTESIAN_POINT('',(-0.021696192316368,0.023042870842176,0.0894509127684591));
#32204=CARTESIAN_POINT('',(-0.019748732684913,0.0219185044997195,0.0895832044351258));
#32205=CARTESIAN_POINT('',(-0.0175,0.0219185044997195,0.0897154961017925));
#32206=CARTESIAN_POINT('',(-0.0152512673150871,0.0219185044997195,0.0898477877684591));
#32207=CARTESIAN_POINT('',(-0.0133038076836321,0.023042870842176,0.0899800794351258));
#32208=CARTESIAN_POINT('',(-0.0113563480521771,0.0241672371846324,0.0901123711017924));
#32209=CARTESIAN_POINT('',(-0.0102319817097207,0.0261146968160874,0.0902446627684591));
#32210=CARTESIAN_POINT('',(-0.00910761536726419,0.0280621564475424,0.0903769544351259));
#32211=CARTESIAN_POINT('',(-0.00910761536726419,0.0303108891324553,0.0905092461017925));
#32212=CARTESIAN_POINT('',(-0.00910761536726418,0.0325596218173683,0.0906415377684592));
#32213=CARTESIAN_POINT('',(-0.0102319817097207,0.0345070814488233,0.0907738294351258));
#32214=CARTESIAN_POINT('',(-0.0113563480521771,0.0364545410802783,0.0909061211017925));
#32215=CARTESIAN_POINT('',(-0.0133038076836321,0.0375789074227347,0.0910384127684591));
#32216=CARTESIAN_POINT('',(-0.0152512673150871,0.0387032737651912,0.0911707044351258));
#32217=CARTESIAN_POINT('',(-0.0175,0.0387032737651912,0.0913029961017925));
#32218=CARTESIAN_POINT('',(-0.019748732684913,0.0387032737651912,0.0914352877684591));
#32219=CARTESIAN_POINT('',(-0.0216961923163679,0.0375789074227348,0.0915675794351258));
#32220=CARTESIAN_POINT('',(-0.023643651947823,0.0364545410802783,0.0916998711017924));
#32221=CARTESIAN_POINT('',(-0.0247680182902794,0.0345070814488233,0.0918321627684591));
#32222=CARTESIAN_POINT('',(-0.0258923846327359,0.0325596218173683,0.0919644544351259));
#32223=CARTESIAN_POINT('',(-0.0258923846327359,0.0303108891324553,0.0920967461017925));
#32224=CARTESIAN_POINT('',(-0.00910761536726419,0.0303108891324553,0.0841592461017925));
#32225=CARTESIAN_POINT('',(-0.00910761536726419,0.0325596218173683,0.0842915377684592));
#32226=CARTESIAN_POINT('',(-0.0102319817097207,0.0345070814488233,0.0844238294351258));
#32227=CARTESIAN_POINT('',(-0.0113563480521771,0.0364545410802783,0.0845561211017925));
#32228=CARTESIAN_POINT('',(-0.0133038076836321,0.0375789074227347,0.0846884127684591));
#32229=CARTESIAN_POINT('',(-0.0152512673150871,0.0387032737651912,0.0848207044351258));
#32230=CARTESIAN_POINT('',(-0.0175,0.0387032737651912,0.0849529961017925));
#32231=CARTESIAN_POINT('',(-0.019748732684913,0.0387032737651912,0.0850852877684591));
#32232=CARTESIAN_POINT('',(-0.0216961923163679,0.0375789074227348,0.0852175794351258));
#32233=CARTESIAN_POINT('',(-0.023643651947823,0.0364545410802783,0.0853498711017925));
#32234=CARTESIAN_POINT('',(-0.0247680182902794,0.0345070814488233,0.0854821627684591));
#32235=CARTESIAN_POINT('',(-0.0258923846327359,0.0325596218173683,0.0856144544351258));
#32236=CARTESIAN_POINT('',(-0.0258923846327359,0.0303108891324553,0.0857467461017925));
#32237=CARTESIAN_POINT('',(-0.0258923846327359,0.0280621564475424,0.0858790377684592));
#32238=CARTESIAN_POINT('',(-0.0247680182902794,0.0261146968160874,0.0860113294351258));
#32239=CARTESIAN_POINT('',(-0.023643651947823,0.0241672371846324,0.0861436211017925));
#32240=CARTESIAN_POINT('',(-0.021696192316368,0.023042870842176,0.0862759127684591));
#32241=CARTESIAN_POINT('',(-0.019748732684913,0.0219185044997195,0.0864082044351258));
#32242=CARTESIAN_POINT('',(-0.0175,0.0219185044997195,0.0865404961017925));
#32243=CARTESIAN_POINT('',(-0.0152512673150871,0.0219185044997195,0.0866727877684591));
#32244=CARTESIAN_POINT('',(-0.0133038076836321,0.023042870842176,0.0868050794351258));
#32245=CARTESIAN_POINT('',(-0.0113563480521771,0.0241672371846324,0.0869373711017925));
#32246=CARTESIAN_POINT('',(-0.0102319817097207,0.0261146968160874,0.0870696627684591));
#32247=CARTESIAN_POINT('',(-0.00910761536726419,0.0280621564475424,0.0872019544351259));
#32248=CARTESIAN_POINT('',(-0.00910761536726419,0.0303108891324553,0.0873342461017925));
#32249=CARTESIAN_POINT('',(-0.00910761536726419,0.0325596218173683,0.0874665377684592));
#32250=CARTESIAN_POINT('',(-0.0102319817097207,0.0345070814488233,0.0875988294351258));
#32251=CARTESIAN_POINT('',(-0.0113563480521771,0.0364545410802783,0.0877311211017925));
#32252=CARTESIAN_POINT('',(-0.0133038076836321,0.0375789074227347,0.0878634127684591));
#32253=CARTESIAN_POINT('',(-0.0152512673150871,0.0387032737651912,0.0879957044351258));
#32254=CARTESIAN_POINT('',(-0.0175,0.0387032737651912,0.0881279961017925));
#32255=CARTESIAN_POINT('',(-0.019748732684913,0.0387032737651912,0.0882602877684591));
#32256=CARTESIAN_POINT('',(-0.0216961923163679,0.0375789074227348,0.0883925794351258));
#32257=CARTESIAN_POINT('',(-0.023643651947823,0.0364545410802783,0.0885248711017924));
#32258=CARTESIAN_POINT('',(-0.0247680182902794,0.0345070814488233,0.0886571627684591));
#32259=CARTESIAN_POINT('',(-0.0258923846327359,0.0325596218173683,0.0887894544351259));
#32260=CARTESIAN_POINT('',(-0.0258923846327359,0.0303108891324553,0.0889217461017925));
#32261=CARTESIAN_POINT('',(-0.0258923846327359,0.0280621564475424,0.0890540377684592));
#32262=CARTESIAN_POINT('',(-0.0247680182902794,0.0261146968160874,0.0891863294351258));
#32263=CARTESIAN_POINT('',(-0.023643651947823,0.0241672371846324,0.0893186211017925));
#32264=CARTESIAN_POINT('',(-0.021696192316368,0.023042870842176,0.0894509127684591));
#32265=CARTESIAN_POINT('',(-0.019748732684913,0.0219185044997195,0.0895832044351258));
#32266=CARTESIAN_POINT('',(-0.0175,0.0219185044997195,0.0897154961017925));
#32267=CARTESIAN_POINT('',(-0.0152512673150871,0.0219185044997195,0.0898477877684591));
#32268=CARTESIAN_POINT('',(-0.0133038076836321,0.023042870842176,0.0899800794351258));
#32269=CARTESIAN_POINT('',(-0.0113563480521771,0.0241672371846324,0.0901123711017924));
#32270=CARTESIAN_POINT('',(-0.0102319817097207,0.0261146968160874,0.0902446627684591));
#32271=CARTESIAN_POINT('',(-0.00910761536726419,0.0280621564475424,0.0903769544351259));
#32272=CARTESIAN_POINT('',(-0.00910761536726419,0.0303108891324553,0.0905092461017925));
#32273=CARTESIAN_POINT('',(-0.00910761536726419,0.0325596218173683,0.0906415377684592));
#32274=CARTESIAN_POINT('',(-0.0102319817097207,0.0345070814488233,0.0907738294351258));
#32275=CARTESIAN_POINT('',(-0.0113563480521771,0.0364545410802783,0.0909061211017925));
#32276=CARTESIAN_POINT('',(-0.0133038076836321,0.0375789074227347,0.0910384127684591));
#32277=CARTESIAN_POINT('',(-0.0152512673150871,0.0387032737651912,0.0911707044351258));
#32278=CARTESIAN_POINT('',(-0.0175,0.0387032737651912,0.0913029961017925));
#32279=CARTESIAN_POINT('',(-0.019748732684913,0.0387032737651912,0.0914352877684591));
#32280=CARTESIAN_POINT('',(-0.0216961923163679,0.0375789074227348,0.0915675794351258));
#32281=CARTESIAN_POINT('',(-0.0226539774004862,0.0370259299465933,0.0916326421368322));
#32282=CARTESIAN_POINT('',(-0.0234358084101918,0.0362437045131391,0.0917));
#32283=CARTESIAN_POINT('',(-0.00910761536726419,0.0303108891324553,0.0841592461017925));
#32284=CARTESIAN_POINT('',(-0.0234358084101918,0.0362437045131391,0.0917));
#32285=CARTESIAN_POINT('',(-0.0234358084101918,0.0362437045131391,0.0917));
#32286=CARTESIAN_POINT('',(-0.0251331818648351,0.0347404540104153,0.0917));
#32287=CARTESIAN_POINT('',(-0.0261619940731697,0.0325741608248562,0.0917));
#32288=CARTESIAN_POINT('',(-0.0262891307345282,0.0303108891324569,0.0917));
#32289=CARTESIAN_POINT('',(-0.0262891307345283,0.0303108891324572,0.0917));
#32290=CARTESIAN_POINT('',(-0.0264009730508963,0.0303108891324564,0.0915881576836321));
#32291=CARTESIAN_POINT('',(-0.0087974,0.0303108891324553,0.0838490307345283));
#32292=CARTESIAN_POINT('',(-0.00910761536726419,0.0303108891324553,0.0841592461017925));
#32293=CARTESIAN_POINT('',(-0.00910761536726419,0.0325596218173683,0.0842915377684592));
#32294=CARTESIAN_POINT('',(-0.0102319817097207,0.0345070814488233,0.0844238294351258));
#32295=CARTESIAN_POINT('',(-0.0113563480521771,0.0364545410802783,0.0845561211017925));
#32296=CARTESIAN_POINT('',(-0.0133038076836321,0.0375789074227347,0.0846884127684591));
#32297=CARTESIAN_POINT('',(-0.0152512673150871,0.0387032737651912,0.0848207044351258));
#32298=CARTESIAN_POINT('',(-0.0175,0.0387032737651912,0.0849529961017925));
#32299=CARTESIAN_POINT('',(-0.019748732684913,0.0387032737651912,0.0850852877684591));
#32300=CARTESIAN_POINT('',(-0.0216961923163679,0.0375789074227348,0.0852175794351258));
#32301=CARTESIAN_POINT('',(-0.023643651947823,0.0364545410802783,0.0853498711017925));
#32302=CARTESIAN_POINT('',(-0.0247680182902794,0.0345070814488233,0.0854821627684591));
#32303=CARTESIAN_POINT('',(-0.0258923846327359,0.0325596218173683,0.0856144544351258));
#32304=CARTESIAN_POINT('',(-0.0258923846327359,0.0303108891324553,0.0857467461017925));
#32305=CARTESIAN_POINT('',(-0.0258923846327359,0.0280621564475424,0.0858790377684592));
#32306=CARTESIAN_POINT('',(-0.0247680182902794,0.0261146968160874,0.0860113294351258));
#32307=CARTESIAN_POINT('',(-0.023643651947823,0.0241672371846324,0.0861436211017925));
#32308=CARTESIAN_POINT('',(-0.021696192316368,0.023042870842176,0.0862759127684591));
#32309=CARTESIAN_POINT('',(-0.019748732684913,0.0219185044997195,0.0864082044351258));
#32310=CARTESIAN_POINT('',(-0.0175,0.0219185044997195,0.0865404961017925));
#32311=CARTESIAN_POINT('',(-0.0152512673150871,0.0219185044997195,0.0866727877684591));
#32312=CARTESIAN_POINT('',(-0.0133038076836321,0.023042870842176,0.0868050794351258));
#32313=CARTESIAN_POINT('',(-0.0113563480521771,0.0241672371846324,0.0869373711017925));
#32314=CARTESIAN_POINT('',(-0.0102319817097207,0.0261146968160874,0.0870696627684591));
#32315=CARTESIAN_POINT('',(-0.00910761536726419,0.0280621564475424,0.0872019544351259));
#32316=CARTESIAN_POINT('',(-0.00910761536726419,0.0303108891324553,0.0873342461017925));
#32317=CARTESIAN_POINT('',(-0.00910761536726419,0.0325596218173683,0.0874665377684592));
#32318=CARTESIAN_POINT('',(-0.0102319817097207,0.0345070814488233,0.0875988294351258));
#32319=CARTESIAN_POINT('',(-0.0113563480521771,0.0364545410802783,0.0877311211017925));
#32320=CARTESIAN_POINT('',(-0.0133038076836321,0.0375789074227347,0.0878634127684591));
#32321=CARTESIAN_POINT('',(-0.0152512673150871,0.0387032737651912,0.0879957044351258));
#32322=CARTESIAN_POINT('',(-0.0175,0.0387032737651912,0.0881279961017925));
#32323=CARTESIAN_POINT('',(-0.019748732684913,0.0387032737651912,0.0882602877684591));
#32324=CARTESIAN_POINT('',(-0.0216961923163679,0.0375789074227348,0.0883925794351258));
#32325=CARTESIAN_POINT('',(-0.023643651947823,0.0364545410802783,0.0885248711017924));
#32326=CARTESIAN_POINT('',(-0.0247680182902794,0.0345070814488233,0.0886571627684591));
#32327=CARTESIAN_POINT('',(-0.0258923846327359,0.0325596218173683,0.0887894544351258));
#32328=CARTESIAN_POINT('',(-0.0258923846327359,0.0303108891324553,0.0889217461017925));
#32329=CARTESIAN_POINT('',(-0.0258923846327359,0.0280621564475424,0.0890540377684592));
#32330=CARTESIAN_POINT('',(-0.0247680182902794,0.0261146968160874,0.0891863294351258));
#32331=CARTESIAN_POINT('',(-0.023643651947823,0.0241672371846324,0.0893186211017925));
#32332=CARTESIAN_POINT('',(-0.021696192316368,0.023042870842176,0.0894509127684591));
#32333=CARTESIAN_POINT('',(-0.019748732684913,0.0219185044997195,0.0895832044351258));
#32334=CARTESIAN_POINT('',(-0.0175,0.0219185044997195,0.0897154961017925));
#32335=CARTESIAN_POINT('',(-0.0152512673150871,0.0219185044997195,0.0898477877684591));
#32336=CARTESIAN_POINT('',(-0.0133038076836321,0.023042870842176,0.0899800794351258));
#32337=CARTESIAN_POINT('',(-0.0113563480521771,0.0241672371846324,0.0901123711017924));
#32338=CARTESIAN_POINT('',(-0.0102319817097207,0.0261146968160874,0.0902446627684591));
#32339=CARTESIAN_POINT('',(-0.00910761536726419,0.0280621564475424,0.0903769544351259));
#32340=CARTESIAN_POINT('',(-0.00910761536726419,0.0303108891324553,0.0905092461017925));
#32341=CARTESIAN_POINT('',(-0.00910761536726419,0.0325596218173683,0.0906415377684592));
#32342=CARTESIAN_POINT('',(-0.0102319817097207,0.0345070814488233,0.0907738294351258));
#32343=CARTESIAN_POINT('',(-0.0113563480521771,0.0364545410802783,0.0909061211017925));
#32344=CARTESIAN_POINT('',(-0.0133038076836321,0.0375789074227347,0.0910384127684591));
#32345=CARTESIAN_POINT('',(-0.0152512673150871,0.0387032737651912,0.0911707044351258));
#32346=CARTESIAN_POINT('',(-0.0175,0.0387032737651912,0.0913029961017925));
#32347=CARTESIAN_POINT('',(-0.019748732684913,0.0387032737651912,0.0914352877684591));
#32348=CARTESIAN_POINT('',(-0.0216961923163679,0.0375789074227348,0.0915675794351258));
#32349=CARTESIAN_POINT('',(-0.0229888949513052,0.0368325652084716,0.0916553932122732));
#32350=CARTESIAN_POINT('',(-0.0239449665364756,0.0356862520195069,0.091745934795067));
#32351=CARTESIAN_POINT('',(-0.00925242797917949,0.0303108891324554,0.0843040587137078));
#32352=CARTESIAN_POINT('',(-0.00925242797917948,0.0325208193949517,0.0844363503803744));
#32353=CARTESIAN_POINT('',(-0.0103573931104277,0.0344346751428656,0.0845686420470411));
#32354=CARTESIAN_POINT('',(-0.0114623582416759,0.0363485308907795,0.0847009337137078));
#32355=CARTESIAN_POINT('',(-0.0133762139895898,0.0374534960220277,0.0848332253803744));
#32356=CARTESIAN_POINT('',(-0.0152900697375036,0.0385584611532759,0.0849655170470411));
#32357=CARTESIAN_POINT('',(-0.0175000000000001,0.0385584611532759,0.0850978087137078));
#32358=CARTESIAN_POINT('',(-0.0197099302624964,0.0385584611532759,0.0852301003803745));
#32359=CARTESIAN_POINT('',(-0.0216237860104103,0.0374534960220277,0.0853623920470411));
#32360=CARTESIAN_POINT('',(-0.0235376417583242,0.0363485308907795,0.0854946837137077));
#32361=CARTESIAN_POINT('',(-0.0246426068895724,0.0344346751428656,0.0856269753803744));
#32362=CARTESIAN_POINT('',(-0.0257475720208206,0.0325208193949517,0.0857592670470411));
#32363=CARTESIAN_POINT('',(-0.0257475720208206,0.0303108891324554,0.0858915587137078));
#32364=CARTESIAN_POINT('',(-0.0257475720208206,0.028100958869959,0.0860238503803745));
#32365=CARTESIAN_POINT('',(-0.0246426068895724,0.0261871031220451,0.0861561420470411));
#32366=CARTESIAN_POINT('',(-0.0235376417583242,0.0242732473741312,0.0862884337137078));
#32367=CARTESIAN_POINT('',(-0.0216237860104103,0.023168282242883,0.0864207253803744));
#32368=CARTESIAN_POINT('',(-0.0197099302624964,0.0220633171116348,0.0865530170470411));
#32369=CARTESIAN_POINT('',(-0.0175000000000001,0.0220633171116348,0.0866853087137078));
#32370=CARTESIAN_POINT('',(-0.0152900697375037,0.0220633171116348,0.0868176003803744));
#32371=CARTESIAN_POINT('',(-0.0133762139895898,0.023168282242883,0.0869498920470411));
#32372=CARTESIAN_POINT('',(-0.0114623582416759,0.0242732473741312,0.0870821837137078));
#32373=CARTESIAN_POINT('',(-0.0103573931104277,0.026187103122045,0.0872144753803745));
#32374=CARTESIAN_POINT('',(-0.0092524279791795,0.0281009588699589,0.0873467670470411));
#32375=CARTESIAN_POINT('',(-0.00925242797917949,0.0303108891324554,0.0874790587137078));
#32376=CARTESIAN_POINT('',(-0.00925242797917948,0.0325208193949517,0.0876113503803744));
#32377=CARTESIAN_POINT('',(-0.0103573931104277,0.0344346751428656,0.0877436420470411));
#32378=CARTESIAN_POINT('',(-0.0114623582416759,0.0363485308907795,0.0878759337137077));
#32379=CARTESIAN_POINT('',(-0.0133762139895898,0.0374534960220277,0.0880082253803745));
#32380=CARTESIAN_POINT('',(-0.0152900697375036,0.0385584611532759,0.088140517047041));
#32381=CARTESIAN_POINT('',(-0.0175000000000001,0.0385584611532759,0.0882728087137078));
#32382=CARTESIAN_POINT('',(-0.0197099302624964,0.0385584611532759,0.0884051003803744));
#32383=CARTESIAN_POINT('',(-0.0216237860104103,0.0374534960220277,0.0885373920470411));
#32384=CARTESIAN_POINT('',(-0.0235376417583242,0.0363485308907795,0.0886696837137077));
#32385=CARTESIAN_POINT('',(-0.0246426068895724,0.0344346751428656,0.0888019753803745));
#32386=CARTESIAN_POINT('',(-0.0257475720208206,0.0325208193949517,0.088934267047041));
#32387=CARTESIAN_POINT('',(-0.0257475720208206,0.0303108891324554,0.0890665587137078));
#32388=CARTESIAN_POINT('',(-0.0257475720208206,0.028100958869959,0.0891988503803744));
#32389=CARTESIAN_POINT('',(-0.0246426068895724,0.0261871031220451,0.0893311420470412));
#32390=CARTESIAN_POINT('',(-0.0235376417583242,0.0242732473741312,0.0894634337137077));
#32391=CARTESIAN_POINT('',(-0.0216237860104103,0.023168282242883,0.0895957253803744));
#32392=CARTESIAN_POINT('',(-0.0197099302624964,0.0220633171116348,0.0897280170470411));
#32393=CARTESIAN_POINT('',(-0.0175000000000001,0.0220633171116348,0.0898603087137078));
#32394=CARTESIAN_POINT('',(-0.0152900697375037,0.0220633171116348,0.0899926003803744));
#32395=CARTESIAN_POINT('',(-0.0133762139895898,0.023168282242883,0.0901248920470411));
#32396=CARTESIAN_POINT('',(-0.0114623582416759,0.0242732473741312,0.0902571837137077));
#32397=CARTESIAN_POINT('',(-0.0103573931104277,0.026187103122045,0.0903894753803744));
#32398=CARTESIAN_POINT('',(-0.0092524279791795,0.0281009588699589,0.0905217670470411));
#32399=CARTESIAN_POINT('',(-0.00925242797917949,0.0303108891324554,0.0906540587137077));
#32400=CARTESIAN_POINT('',(-0.00925242797917948,0.0325208193949517,0.0907863503803744));
#32401=CARTESIAN_POINT('',(-0.0103573931104277,0.0344346751428656,0.0909186420470411));
#32402=CARTESIAN_POINT('',(-0.0114623582416759,0.0363485308907795,0.0910509337137077));
#32403=CARTESIAN_POINT('',(-0.0133762139895898,0.0374534960220277,0.0911832253803744));
#32404=CARTESIAN_POINT('',(-0.0152900697375036,0.0385584611532759,0.0913155170470411));
#32405=CARTESIAN_POINT('',(-0.0175000000000001,0.0385584611532759,0.0914478087137078));
#32406=CARTESIAN_POINT('',(-0.0197099302624964,0.0385584611532759,0.0915801003803744));
#32407=CARTESIAN_POINT('',(-0.0216237860104103,0.0374534960220277,0.0917123920470411));
#32408=CARTESIAN_POINT('',(-0.0228941827509936,0.0367200321218743,0.0918002058241885));
#32409=CARTESIAN_POINT('',(-0.0238337570914016,0.035593498842224,0.0918907474069823));
#32410=CARTESIAN_POINT('',(-0.00933080000000004,0.0303108891324554,0.0844932655092833));
#32411=CARTESIAN_POINT('',(-0.00933080000000003,0.0324998196752636,0.08462555717595));
#32412=CARTESIAN_POINT('',(-0.0104252652714042,0.0343954891324553,0.0847578488426167));
#32413=CARTESIAN_POINT('',(-0.0115197305428084,0.036291158589647,0.0848901405092833));
#32414=CARTESIAN_POINT('',(-0.0134154,0.0373856238610512,0.08502243217595));
#32415=CARTESIAN_POINT('',(-0.0153110694571917,0.0384800891324553,0.0851547238426166));
#32416=CARTESIAN_POINT('',(-0.0175000000000001,0.0384800891324554,0.0852870155092833));
#32417=CARTESIAN_POINT('',(-0.0196889305428084,0.0384800891324553,0.08541930717595));
#32418=CARTESIAN_POINT('',(-0.0215846000000001,0.0373856238610512,0.0855515988426167));
#32419=CARTESIAN_POINT('',(-0.0234802694571917,0.036291158589647,0.0856838905092833));
#32420=CARTESIAN_POINT('',(-0.0245747347285959,0.0343954891324554,0.08581618217595));
#32421=CARTESIAN_POINT('',(-0.0256692,0.0324998196752637,0.0859484738426166));
#32422=CARTESIAN_POINT('',(-0.0256692000000001,0.0303108891324554,0.0860807655092833));
#32423=CARTESIAN_POINT('',(-0.0256692000000001,0.028121958589647,0.08621305717595));
#32424=CARTESIAN_POINT('',(-0.0245747347285959,0.0262262891324554,0.0863453488426167));
#32425=CARTESIAN_POINT('',(-0.0234802694571917,0.0243306196752637,0.0864776405092833));
#32426=CARTESIAN_POINT('',(-0.0215846000000001,0.0232361544038595,0.08660993217595));
#32427=CARTESIAN_POINT('',(-0.0196889305428084,0.0221416891324553,0.0867422238426167));
#32428=CARTESIAN_POINT('',(-0.0175000000000001,0.0221416891324553,0.0868745155092834));
#32429=CARTESIAN_POINT('',(-0.0153110694571917,0.0221416891324553,0.08700680717595));
#32430=CARTESIAN_POINT('',(-0.0134154000000001,0.0232361544038595,0.0871390988426167));
#32431=CARTESIAN_POINT('',(-0.0115197305428084,0.0243306196752637,0.0872713905092833));
#32432=CARTESIAN_POINT('',(-0.0104252652714042,0.0262262891324553,0.08740368217595));
#32433=CARTESIAN_POINT('',(-0.00933080000000004,0.028121958589647,0.0875359738426167));
#32434=CARTESIAN_POINT('',(-0.00933080000000004,0.0303108891324554,0.0876682655092834));
#32435=CARTESIAN_POINT('',(-0.00933080000000003,0.0324998196752636,0.08780055717595));
#32436=CARTESIAN_POINT('',(-0.0104252652714042,0.0343954891324553,0.0879328488426166));
#32437=CARTESIAN_POINT('',(-0.0115197305428084,0.036291158589647,0.0880651405092833));
#32438=CARTESIAN_POINT('',(-0.0134154,0.0373856238610512,0.0881974321759499));
#32439=CARTESIAN_POINT('',(-0.0153110694571917,0.0384800891324553,0.0883297238426167));
#32440=CARTESIAN_POINT('',(-0.0175000000000001,0.0384800891324554,0.0884620155092833));
#32441=CARTESIAN_POINT('',(-0.0196889305428084,0.0384800891324553,0.08859430717595));
#32442=CARTESIAN_POINT('',(-0.0215846000000001,0.0373856238610512,0.0887265988426167));
#32443=CARTESIAN_POINT('',(-0.0234802694571917,0.036291158589647,0.0888588905092832));
#32444=CARTESIAN_POINT('',(-0.0245747347285959,0.0343954891324554,0.08899118217595));
#32445=CARTESIAN_POINT('',(-0.0256692,0.0324998196752637,0.0891234738426166));
#32446=CARTESIAN_POINT('',(-0.0256692000000001,0.0303108891324554,0.0892557655092833));
#32447=CARTESIAN_POINT('',(-0.0256692000000001,0.028121958589647,0.0893880571759499));
#32448=CARTESIAN_POINT('',(-0.0245747347285959,0.0262262891324554,0.0895203488426166));
#32449=CARTESIAN_POINT('',(-0.0234802694571917,0.0243306196752637,0.0896526405092834));
#32450=CARTESIAN_POINT('',(-0.0215846000000001,0.0232361544038595,0.08978493217595));
#32451=CARTESIAN_POINT('',(-0.0196889305428084,0.0221416891324553,0.0899172238426166));
#32452=CARTESIAN_POINT('',(-0.0175000000000001,0.0221416891324553,0.0900495155092833));
#32453=CARTESIAN_POINT('',(-0.0153110694571917,0.0221416891324553,0.0901818071759499));
#32454=CARTESIAN_POINT('',(-0.0134154000000001,0.0232361544038595,0.0903140988426166));
#32455=CARTESIAN_POINT('',(-0.0115197305428084,0.0243306196752637,0.0904463905092833));
#32456=CARTESIAN_POINT('',(-0.0104252652714042,0.0262262891324553,0.09057868217595));
#32457=CARTESIAN_POINT('',(-0.00933080000000004,0.028121958589647,0.0907109738426166));
#32458=CARTESIAN_POINT('',(-0.00933080000000004,0.0303108891324554,0.0908432655092833));
#32459=CARTESIAN_POINT('',(-0.00933080000000003,0.0324998196752636,0.0909755571759499));
#32460=CARTESIAN_POINT('',(-0.0104252652714042,0.0343954891324553,0.0911078488426166));
#32461=CARTESIAN_POINT('',(-0.0115197305428084,0.036291158589647,0.0912401405092833));
#32462=CARTESIAN_POINT('',(-0.0134154,0.0373856238610512,0.09137243217595));
#32463=CARTESIAN_POINT('',(-0.0153110694571917,0.0384800891324553,0.0915047238426166));
#32464=CARTESIAN_POINT('',(-0.0175000000000001,0.0384800891324554,0.0916370155092833));
#32465=CARTESIAN_POINT('',(-0.0196889305428084,0.0384800891324553,0.0917693071759499));
#32466=CARTESIAN_POINT('',(-0.0215846000000001,0.0373856238610512,0.0919015988426167));
#32467=CARTESIAN_POINT('',(-0.0228429248775488,0.0366591296542704,0.0919894126197641));
#32468=CARTESIAN_POINT('',(-0.0237735709734282,0.0355433011844023,0.0920799542025578));
#32469=CARTESIAN_POINT('',(-0.0093308,0.0303108891324553,0.0846980614690566));
#32470=CARTESIAN_POINT('',(-0.00933080000000004,0.0324998196752637,0.0848303531357232));
#32471=CARTESIAN_POINT('',(-0.0104252652714042,0.0343954891324554,0.0849626448023899));
#32472=CARTESIAN_POINT('',(-0.0115197305428084,0.036291158589647,0.0850949364690567));
#32473=CARTESIAN_POINT('',(-0.0134154,0.0373856238610511,0.0852272281357233));
#32474=CARTESIAN_POINT('',(-0.0153110694571917,0.0384800891324553,0.08535951980239));
#32475=CARTESIAN_POINT('',(-0.0175,0.0384800891324554,0.0854918114690566));
#32476=CARTESIAN_POINT('',(-0.0196889305428084,0.0384800891324554,0.0856241031357233));
#32477=CARTESIAN_POINT('',(-0.0215846,0.0373856238610512,0.0857563948023899));
#32478=CARTESIAN_POINT('',(-0.0234802694571917,0.036291158589647,0.0858886864690566));
#32479=CARTESIAN_POINT('',(-0.0245747347285959,0.0343954891324554,0.0860209781357233));
#32480=CARTESIAN_POINT('',(-0.0256692000000001,0.0324998196752637,0.0861532698023899));
#32481=CARTESIAN_POINT('',(-0.0256692,0.0303108891324553,0.0862855614690566));
#32482=CARTESIAN_POINT('',(-0.0256692000000001,0.028121958589647,0.0864178531357234));
#32483=CARTESIAN_POINT('',(-0.0245747347285959,0.0262262891324554,0.0865501448023899));
#32484=CARTESIAN_POINT('',(-0.0234802694571917,0.0243306196752637,0.0866824364690567));
#32485=CARTESIAN_POINT('',(-0.0215846,0.0232361544038595,0.0868147281357233));
#32486=CARTESIAN_POINT('',(-0.0196889305428084,0.0221416891324553,0.08694701980239));
#32487=CARTESIAN_POINT('',(-0.0175,0.0221416891324554,0.0870793114690566));
#32488=CARTESIAN_POINT('',(-0.0153110694571917,0.0221416891324553,0.0872116031357233));
#32489=CARTESIAN_POINT('',(-0.0134154,0.0232361544038595,0.0873438948023899));
#32490=CARTESIAN_POINT('',(-0.0115197305428084,0.0243306196752637,0.0874761864690566));
#32491=CARTESIAN_POINT('',(-0.0104252652714042,0.0262262891324553,0.0876084781357233));
#32492=CARTESIAN_POINT('',(-0.00933080000000005,0.028121958589647,0.0877407698023899));
#32493=CARTESIAN_POINT('',(-0.0093308,0.0303108891324553,0.0878730614690566));
#32494=CARTESIAN_POINT('',(-0.00933080000000004,0.0324998196752637,0.0880053531357233));
#32495=CARTESIAN_POINT('',(-0.0104252652714042,0.0343954891324554,0.0881376448023899));
#32496=CARTESIAN_POINT('',(-0.0115197305428084,0.036291158589647,0.0882699364690567));
#32497=CARTESIAN_POINT('',(-0.0134154,0.0373856238610511,0.0884022281357233));
#32498=CARTESIAN_POINT('',(-0.0153110694571917,0.0384800891324553,0.08853451980239));
#32499=CARTESIAN_POINT('',(-0.0175,0.0384800891324554,0.0886668114690566));
#32500=CARTESIAN_POINT('',(-0.0196889305428084,0.0384800891324554,0.0887991031357233));
#32501=CARTESIAN_POINT('',(-0.0215846,0.0373856238610512,0.0889313948023899));
#32502=CARTESIAN_POINT('',(-0.0234802694571917,0.036291158589647,0.0890636864690566));
#32503=CARTESIAN_POINT('',(-0.0245747347285959,0.0343954891324554,0.0891959781357233));
#32504=CARTESIAN_POINT('',(-0.0256692000000001,0.0324998196752637,0.0893282698023899));
#32505=CARTESIAN_POINT('',(-0.0256692,0.0303108891324553,0.0894605614690566));
#32506=CARTESIAN_POINT('',(-0.0256692000000001,0.028121958589647,0.0895928531357233));
#32507=CARTESIAN_POINT('',(-0.0245747347285959,0.0262262891324554,0.0897251448023899));
#32508=CARTESIAN_POINT('',(-0.0234802694571917,0.0243306196752637,0.0898574364690567));
#32509=CARTESIAN_POINT('',(-0.0215846,0.0232361544038595,0.0899897281357233));
#32510=CARTESIAN_POINT('',(-0.0196889305428084,0.0221416891324553,0.09012201980239));
#32511=CARTESIAN_POINT('',(-0.0175,0.0221416891324554,0.0902543114690566));
#32512=CARTESIAN_POINT('',(-0.0153110694571917,0.0221416891324553,0.0903866031357233));
#32513=CARTESIAN_POINT('',(-0.0134154,0.0232361544038595,0.0905188948023899));
#32514=CARTESIAN_POINT('',(-0.0115197305428084,0.0243306196752637,0.0906511864690566));
#32515=CARTESIAN_POINT('',(-0.0104252652714042,0.0262262891324553,0.0907834781357233));
#32516=CARTESIAN_POINT('',(-0.00933080000000005,0.028121958589647,0.0909157698023899));
#32517=CARTESIAN_POINT('',(-0.0093308,0.0303108891324553,0.0910480614690566));
#32518=CARTESIAN_POINT('',(-0.00933080000000004,0.0324998196752637,0.0911803531357234));
#32519=CARTESIAN_POINT('',(-0.0104252652714042,0.0343954891324554,0.0913126448023899));
#32520=CARTESIAN_POINT('',(-0.0115197305428084,0.036291158589647,0.0914449364690567));
#32521=CARTESIAN_POINT('',(-0.0134154,0.0373856238610511,0.0915772281357233));
#32522=CARTESIAN_POINT('',(-0.0153110694571917,0.0384800891324553,0.09170951980239));
#32523=CARTESIAN_POINT('',(-0.0175,0.0384800891324554,0.0918418114690566));
#32524=CARTESIAN_POINT('',(-0.0196889305428084,0.0384800891324554,0.0919741031357233));
#32525=CARTESIAN_POINT('',(-0.0215846,0.0373856238610512,0.0921063948023899));
#32526=CARTESIAN_POINT('',(-0.0228429248775487,0.0366591296542704,0.0921942085795374));
#32527=CARTESIAN_POINT('',(-0.0237735709734282,0.0355433011844023,0.0922847501623312));
#32528=CARTESIAN_POINT('',(-0.0093308,0.0303108891324553,0.0846980614690566));
#32529=CARTESIAN_POINT('',(-0.00933080000000005,0.0324998196752637,0.0848303531357232));
#32530=CARTESIAN_POINT('',(-0.0104252652714042,0.0343954891324554,0.0849626448023899));
#32531=CARTESIAN_POINT('',(-0.0115197305428084,0.036291158589647,0.0850949364690567));
#32532=CARTESIAN_POINT('',(-0.0134154,0.0373856238610511,0.0852272281357233));
#32533=CARTESIAN_POINT('',(-0.0153110694571917,0.0384800891324553,0.08535951980239));
#32534=CARTESIAN_POINT('',(-0.0175,0.0384800891324554,0.0854918114690566));
#32535=CARTESIAN_POINT('',(-0.0196889305428084,0.0384800891324554,0.0856241031357233));
#32536=CARTESIAN_POINT('',(-0.0215846,0.0373856238610512,0.0857563948023899));
#32537=CARTESIAN_POINT('',(-0.0234802694571917,0.036291158589647,0.0858886864690566));
#32538=CARTESIAN_POINT('',(-0.0245747347285959,0.0343954891324554,0.0860209781357233));
#32539=CARTESIAN_POINT('',(-0.0256692000000001,0.0324998196752637,0.0861532698023899));
#32540=CARTESIAN_POINT('',(-0.0256692,0.0303108891324553,0.0862855614690566));
#32541=CARTESIAN_POINT('',(-0.0256692000000001,0.028121958589647,0.0864178531357234));
#32542=CARTESIAN_POINT('',(-0.0245747347285959,0.0262262891324554,0.0865501448023899));
#32543=CARTESIAN_POINT('',(-0.0234802694571917,0.0243306196752637,0.0866824364690567));
#32544=CARTESIAN_POINT('',(-0.0215846,0.0232361544038595,0.0868147281357233));
#32545=CARTESIAN_POINT('',(-0.0196889305428084,0.0221416891324553,0.08694701980239));
#32546=CARTESIAN_POINT('',(-0.0175,0.0221416891324554,0.0870793114690566));
#32547=CARTESIAN_POINT('',(-0.0153110694571917,0.0221416891324553,0.0872116031357233));
#32548=CARTESIAN_POINT('',(-0.0134154,0.0232361544038595,0.0873438948023899));
#32549=CARTESIAN_POINT('',(-0.0115197305428084,0.0243306196752637,0.0874761864690566));
#32550=CARTESIAN_POINT('',(-0.0104252652714042,0.0262262891324553,0.0876084781357233));
#32551=CARTESIAN_POINT('',(-0.00933080000000005,0.028121958589647,0.0877407698023899));
#32552=CARTESIAN_POINT('',(-0.0093308,0.0303108891324553,0.0878730614690566));
#32553=CARTESIAN_POINT('',(-0.00933080000000005,0.0324998196752637,0.0880053531357232));
#32554=CARTESIAN_POINT('',(-0.0104252652714042,0.0343954891324554,0.0881376448023899));
#32555=CARTESIAN_POINT('',(-0.0115197305428084,0.036291158589647,0.0882699364690567));
#32556=CARTESIAN_POINT('',(-0.0134154,0.0373856238610511,0.0884022281357233));
#32557=CARTESIAN_POINT('',(-0.0153110694571917,0.0384800891324553,0.08853451980239));
#32558=CARTESIAN_POINT('',(-0.0175,0.0384800891324554,0.0886668114690566));
#32559=CARTESIAN_POINT('',(-0.0196889305428084,0.0384800891324554,0.0887991031357233));
#32560=CARTESIAN_POINT('',(-0.0215846,0.0373856238610512,0.0889313948023899));
#32561=CARTESIAN_POINT('',(-0.0234802694571917,0.036291158589647,0.0890636864690566));
#32562=CARTESIAN_POINT('',(-0.0245747347285959,0.0343954891324554,0.0891959781357233));
#32563=CARTESIAN_POINT('',(-0.0256692000000001,0.0324998196752637,0.0893282698023899));
#32564=CARTESIAN_POINT('',(-0.0256692,0.0303108891324553,0.0894605614690566));
#32565=CARTESIAN_POINT('',(-0.0256692000000001,0.028121958589647,0.0895928531357233));
#32566=CARTESIAN_POINT('',(-0.0245747347285959,0.0262262891324554,0.0897251448023899));
#32567=CARTESIAN_POINT('',(-0.0234802694571917,0.0243306196752637,0.0898574364690567));
#32568=CARTESIAN_POINT('',(-0.0215846,0.0232361544038595,0.0899897281357233));
#32569=CARTESIAN_POINT('',(-0.0196889305428084,0.0221416891324553,0.09012201980239));
#32570=CARTESIAN_POINT('',(-0.0175,0.0221416891324554,0.0902543114690566));
#32571=CARTESIAN_POINT('',(-0.0153110694571917,0.0221416891324553,0.0903866031357233));
#32572=CARTESIAN_POINT('',(-0.0134154,0.0232361544038595,0.0905188948023899));
#32573=CARTESIAN_POINT('',(-0.0115197305428084,0.0243306196752637,0.0906511864690566));
#32574=CARTESIAN_POINT('',(-0.0104252652714042,0.0262262891324553,0.0907834781357233));
#32575=CARTESIAN_POINT('',(-0.00933080000000005,0.028121958589647,0.0909157698023899));
#32576=CARTESIAN_POINT('',(-0.0093308,0.0303108891324553,0.0910480614690566));
#32577=CARTESIAN_POINT('',(-0.00933080000000005,0.0324998196752637,0.0911803531357234));
#32578=CARTESIAN_POINT('',(-0.0104252652714042,0.0343954891324554,0.0913126448023899));
#32579=CARTESIAN_POINT('',(-0.0115197305428084,0.036291158589647,0.0914449364690567));
#32580=CARTESIAN_POINT('',(-0.0134154,0.0373856238610511,0.0915772281357233));
#32581=CARTESIAN_POINT('',(-0.0142798580955441,0.0378847189752167,0.0916375554263219));
#32582=CARTESIAN_POINT('',(-0.0152390568438961,0.0381609824239307,0.0917));
#32583=CARTESIAN_POINT('',(-0.0093308,0.0303108891324553,0.0846980614690566));
#32584=CARTESIAN_POINT('',(-0.0152390568438961,0.0381609824239307,0.0917));
#32585=CARTESIAN_POINT('',(-0.0152390568438961,0.0381609824239307,0.0917));
#32586=CARTESIAN_POINT('',(-0.0166557501341046,0.0385690110778415,0.0917));
#32587=CARTESIAN_POINT('',(-0.0196821427881546,0.038626058036794,0.0917000000000001));
#32588=CARTESIAN_POINT('',(-0.0223327085372635,0.0372206465255158,0.0917));
#32589=CARTESIAN_POINT('',(-0.0234358084101918,0.0362437045131391,0.0917));
#32590=CARTESIAN_POINT('',(-0.0085688,0.0303108891324553,0.0846980614690566));
#32591=CARTESIAN_POINT('',(-0.0175,0.0303108891324553,0.0863555479362832));
#32592=CARTESIAN_POINT('',(-0.0093308,0.0303108891324553,0.0850479938051895));
#32593=CARTESIAN_POINT('',(-0.00933080000000005,0.0324998196752637,0.0851802854718562));
#32594=CARTESIAN_POINT('',(-0.0104252652714042,0.0343954891324554,0.0853125771385228));
#32595=CARTESIAN_POINT('',(-0.0115197305428084,0.036291158589647,0.0854448688051895));
#32596=CARTESIAN_POINT('',(-0.0134154,0.0373856238610512,0.0855771604718562));
#32597=CARTESIAN_POINT('',(-0.0153110694571917,0.0384800891324553,0.0857094521385228));
#32598=CARTESIAN_POINT('',(-0.0175,0.0384800891324554,0.0858417438051895));
#32599=CARTESIAN_POINT('',(-0.0196889305428084,0.0384800891324554,0.0859740354718562));
#32600=CARTESIAN_POINT('',(-0.0215846,0.0373856238610512,0.0861063271385228));
#32601=CARTESIAN_POINT('',(-0.0234802694571917,0.036291158589647,0.0862386188051896));
#32602=CARTESIAN_POINT('',(-0.0245747347285959,0.0343954891324554,0.0863709104718562));
#32603=CARTESIAN_POINT('',(-0.0256692000000001,0.0324998196752637,0.0865032021385229));
#32604=CARTESIAN_POINT('',(-0.0256692,0.0303108891324553,0.0866354938051895));
#32605=CARTESIAN_POINT('',(-0.0256692000000001,0.028121958589647,0.0867677854718562));
#32606=CARTESIAN_POINT('',(-0.0245747347285959,0.0262262891324554,0.0869000771385228));
#32607=CARTESIAN_POINT('',(-0.0234802694571917,0.0243306196752637,0.0870323688051895));
#32608=CARTESIAN_POINT('',(-0.0215846,0.0232361544038595,0.0871646604718562));
#32609=CARTESIAN_POINT('',(-0.0196889305428084,0.0221416891324553,0.0872969521385228));
#32610=CARTESIAN_POINT('',(-0.0175,0.0221416891324554,0.0874292438051895));
#32611=CARTESIAN_POINT('',(-0.0153110694571917,0.0221416891324553,0.0875615354718562));
#32612=CARTESIAN_POINT('',(-0.0134154,0.0232361544038595,0.0876938271385228));
#32613=CARTESIAN_POINT('',(-0.0115197305428084,0.0243306196752637,0.0878261188051896));
#32614=CARTESIAN_POINT('',(-0.0104252652714042,0.0262262891324554,0.0879584104718562));
#32615=CARTESIAN_POINT('',(-0.00933080000000005,0.028121958589647,0.0880907021385229));
#32616=CARTESIAN_POINT('',(-0.0093308,0.0303108891324553,0.0882229938051895));
#32617=CARTESIAN_POINT('',(-0.00933080000000005,0.0324998196752637,0.0883552854718562));
#32618=CARTESIAN_POINT('',(-0.0104252652714042,0.0343954891324554,0.0884875771385228));
#32619=CARTESIAN_POINT('',(-0.0115197305428084,0.036291158589647,0.0886198688051895));
#32620=CARTESIAN_POINT('',(-0.0134154,0.0373856238610512,0.0887521604718562));
#32621=CARTESIAN_POINT('',(-0.0153110694571917,0.0384800891324553,0.0888844521385229));
#32622=CARTESIAN_POINT('',(-0.0175,0.0384800891324554,0.0890167438051895));
#32623=CARTESIAN_POINT('',(-0.0196889305428084,0.0384800891324554,0.0891490354718562));
#32624=CARTESIAN_POINT('',(-0.0215846,0.0373856238610512,0.0892813271385228));
#32625=CARTESIAN_POINT('',(-0.0234802694571917,0.036291158589647,0.0894136188051896));
#32626=CARTESIAN_POINT('',(-0.0245747347285959,0.0343954891324554,0.0895459104718562));
#32627=CARTESIAN_POINT('',(-0.0256692000000001,0.0324998196752637,0.0896782021385229));
#32628=CARTESIAN_POINT('',(-0.0256692,0.0303108891324553,0.0898104938051895));
#32629=CARTESIAN_POINT('',(-0.0256692000000001,0.028121958589647,0.0899427854718562));
#32630=CARTESIAN_POINT('',(-0.0245747347285959,0.0262262891324554,0.0900750771385228));
#32631=CARTESIAN_POINT('',(-0.0234802694571917,0.0243306196752637,0.0902073688051895));
#32632=CARTESIAN_POINT('',(-0.0215846,0.0232361544038595,0.0903396604718562));
#32633=CARTESIAN_POINT('',(-0.0196889305428084,0.0221416891324553,0.0904719521385229));
#32634=CARTESIAN_POINT('',(-0.0175,0.0221416891324554,0.0906042438051895));
#32635=CARTESIAN_POINT('',(-0.0153110694571917,0.0221416891324553,0.0907365354718562));
#32636=CARTESIAN_POINT('',(-0.0134154,0.0232361544038595,0.0908688271385228));
#32637=CARTESIAN_POINT('',(-0.0115197305428084,0.0243306196752637,0.0910011188051895));
#32638=CARTESIAN_POINT('',(-0.0104252652714042,0.0262262891324554,0.0911334104718562));
#32639=CARTESIAN_POINT('',(-0.00933080000000005,0.028121958589647,0.0912657021385229));
#32640=CARTESIAN_POINT('',(-0.0093308,0.0303108891324553,0.0913979938051895));
#32641=CARTESIAN_POINT('',(-0.00933080000000005,0.0324998196752637,0.0915302854718562));
#32642=CARTESIAN_POINT('',(-0.0104252652714042,0.0343954891324554,0.0916625771385228));
#32643=CARTESIAN_POINT('',(-0.0105787406133938,0.0346613162224903,0.0916811282148471));
#32644=CARTESIAN_POINT('',(-0.0107517314949501,0.0349148766241576,0.0917));
#32645=CARTESIAN_POINT('',(-0.0093308,0.0303108891324553,0.0850479938051895));
#32646=CARTESIAN_POINT('',(-0.0107517314949501,0.0349148766241576,0.0917));
#32647=CARTESIAN_POINT('',(-0.0175,0.0303108891324553,0.0917));
#32648=CARTESIAN_POINT('',(-0.0093308,0.0303108891324553,0.0848730276371231));
#32649=CARTESIAN_POINT('',(-0.00832342471144782,0.0303108891324553,0.085499093987987));
#32650=CARTESIAN_POINT('',(-0.008518,0.0303108891324553,0.0856623620408474));
#32651=CARTESIAN_POINT('',(-0.00847389336287265,0.0303108891324553,0.0854122208715823));
#32652=CARTESIAN_POINT('',(-0.008264,0.0303108891324553,0.0856623620408474));
#32653=CARTESIAN_POINT('',(-0.0087974,0.0303108891324553,0.0853551779230184));
#32654=CARTESIAN_POINT('',(-0.00912090663712743,0.0303108891324553,0.0852981349744546));
#32655=CARTESIAN_POINT('',(-0.0090768,0.0303108891324553,0.0850479938051895));
#32656=CARTESIAN_POINT('',(-0.008264,0.0303108891324553,0.0843311810204237));
#32657=CARTESIAN_POINT('',(-0.0175,0.0303108891324553,0.0867173896326779));
#32658=CARTESIAN_POINT('',(-0.026736,0.0303108891324553,0.09135));
#32659=CARTESIAN_POINT('',(-0.026736,0.0303108891324553,0.091));
#32660=CARTESIAN_POINT('',(-0.026736,0.0303108891324564,0.0917));
#32661=CARTESIAN_POINT('',(-0.0175,0.0303108891324553,0.0917));
#32662=CARTESIAN_POINT('',(-0.00997922046889643,0.0249497725281897,0.0917));
#32663=CARTESIAN_POINT('',(-0.0213627414806,0.0219214359766142,0.0910000000000001));
#32664=CARTESIAN_POINT('',(-0.0195241340747034,0.0210748891324554,0.0911104100162255));
#32665=CARTESIAN_POINT('',(-0.0175,0.0210748891324553,0.0912186120408473));
#32666=CARTESIAN_POINT('',(-0.0150252212587062,0.0210748891324553,0.0913509037075141));
#32667=CARTESIAN_POINT('',(-0.012882,0.0223122785031023,0.0914831953741807));
#32668=CARTESIAN_POINT('',(-0.0111440750554154,0.0233156699376896,0.0915904698735012));
#32669=CARTESIAN_POINT('',(-0.00997922046889642,0.0249497725281897,0.0916999999999999));
#32670=CARTESIAN_POINT('',(-0.0213627414806001,0.0219214359766143,0.091));
#32671=CARTESIAN_POINT('',(-0.0175,0.0303108891324553,0.091));
#32672=CARTESIAN_POINT('',(-0.0093308,0.0303108891324553,0.0850479938051895));
#32673=CARTESIAN_POINT('',(-0.00933080000000005,0.0324998196752637,0.0851802854718562));
#32674=CARTESIAN_POINT('',(-0.0104252652714042,0.0343954891324554,0.0853125771385228));
#32675=CARTESIAN_POINT('',(-0.0115197305428084,0.036291158589647,0.0854448688051895));
#32676=CARTESIAN_POINT('',(-0.0134154,0.0373856238610511,0.0855771604718562));
#32677=CARTESIAN_POINT('',(-0.0153110694571917,0.0384800891324553,0.0857094521385228));
#32678=CARTESIAN_POINT('',(-0.0175,0.0384800891324554,0.0858417438051895));
#32679=CARTESIAN_POINT('',(-0.0196889305428084,0.0384800891324553,0.0859740354718562));
#32680=CARTESIAN_POINT('',(-0.0215846,0.0373856238610512,0.0861063271385228));
#32681=CARTESIAN_POINT('',(-0.0234802694571917,0.036291158589647,0.0862386188051896));
#32682=CARTESIAN_POINT('',(-0.0245747347285959,0.0343954891324554,0.0863709104718562));
#32683=CARTESIAN_POINT('',(-0.0256692000000001,0.0324998196752637,0.0865032021385229));
#32684=CARTESIAN_POINT('',(-0.0256692,0.0303108891324553,0.0866354938051895));
#32685=CARTESIAN_POINT('',(-0.0256692000000001,0.028121958589647,0.0867677854718562));
#32686=CARTESIAN_POINT('',(-0.0245747347285959,0.0262262891324554,0.0869000771385228));
#32687=CARTESIAN_POINT('',(-0.0234802694571917,0.0243306196752637,0.0870323688051895));
#32688=CARTESIAN_POINT('',(-0.0215846,0.0232361544038595,0.0871646604718562));
#32689=CARTESIAN_POINT('',(-0.0196889305428084,0.0221416891324553,0.0872969521385228));
#32690=CARTESIAN_POINT('',(-0.0175,0.0221416891324554,0.0874292438051895));
#32691=CARTESIAN_POINT('',(-0.0153110694571917,0.0221416891324553,0.0875615354718562));
#32692=CARTESIAN_POINT('',(-0.0134154,0.0232361544038595,0.0876938271385228));
#32693=CARTESIAN_POINT('',(-0.0115197305428084,0.0243306196752637,0.0878261188051896));
#32694=CARTESIAN_POINT('',(-0.0104252652714042,0.0262262891324553,0.0879584104718562));
#32695=CARTESIAN_POINT('',(-0.00933080000000006,0.028121958589647,0.0880907021385229));
#32696=CARTESIAN_POINT('',(-0.0093308,0.0303108891324553,0.0882229938051895));
#32697=CARTESIAN_POINT('',(-0.00933080000000005,0.0324998196752637,0.0883552854718562));
#32698=CARTESIAN_POINT('',(-0.0104252652714042,0.0343954891324554,0.0884875771385228));
#32699=CARTESIAN_POINT('',(-0.0115197305428084,0.036291158589647,0.0886198688051895));
#32700=CARTESIAN_POINT('',(-0.0134154,0.0373856238610511,0.0887521604718562));
#32701=CARTESIAN_POINT('',(-0.0153110694571917,0.0384800891324553,0.0888844521385229));
#32702=CARTESIAN_POINT('',(-0.0175,0.0384800891324554,0.0890167438051895));
#32703=CARTESIAN_POINT('',(-0.0196889305428084,0.0384800891324553,0.0891490354718562));
#32704=CARTESIAN_POINT('',(-0.0215846,0.0373856238610512,0.0892813271385228));
#32705=CARTESIAN_POINT('',(-0.0234802694571917,0.036291158589647,0.0894136188051895));
#32706=CARTESIAN_POINT('',(-0.0245747347285959,0.0343954891324554,0.0895459104718562));
#32707=CARTESIAN_POINT('',(-0.0256692000000001,0.0324998196752637,0.0896782021385228));
#32708=CARTESIAN_POINT('',(-0.0256692,0.0303108891324553,0.0898104938051895));
#32709=CARTESIAN_POINT('',(-0.0256692000000001,0.028121958589647,0.0899427854718562));
#32710=CARTESIAN_POINT('',(-0.0245747347285959,0.0262262891324554,0.0900750771385228));
#32711=CARTESIAN_POINT('',(-0.0234802694571917,0.0243306196752637,0.0902073688051895));
#32712=CARTESIAN_POINT('',(-0.0215846,0.0232361544038595,0.0903396604718562));
#32713=CARTESIAN_POINT('',(-0.0196889305428084,0.0221416891324553,0.0904719521385229));
#32714=CARTESIAN_POINT('',(-0.0175,0.0221416891324554,0.0906042438051895));
#32715=CARTESIAN_POINT('',(-0.0153110694571917,0.0221416891324553,0.0907365354718562));
#32716=CARTESIAN_POINT('',(-0.0134154,0.0232361544038595,0.0908688271385228));
#32717=CARTESIAN_POINT('',(-0.0115197305428084,0.0243306196752637,0.0910011188051895));
#32718=CARTESIAN_POINT('',(-0.0104252652714042,0.0262262891324553,0.0911334104718562));
#32719=CARTESIAN_POINT('',(-0.00933080000000006,0.028121958589647,0.0912657021385229));
#32720=CARTESIAN_POINT('',(-0.0093308,0.0303108891324553,0.0913979938051895));
#32721=CARTESIAN_POINT('',(-0.00933080000000005,0.0324998196752637,0.0915302854718562));
#32722=CARTESIAN_POINT('',(-0.0104252652714042,0.0343954891324554,0.0916625771385228));
#32723=CARTESIAN_POINT('',(-0.0107406510492572,0.0349417533236814,0.0917006988690932));
#32724=CARTESIAN_POINT('',(-0.0111361563717333,0.0354331272092114,0.0917399368095904));
#32725=CARTESIAN_POINT('',(-0.00933080000000005,0.0303108891324553,0.085176952984899));
#32726=CARTESIAN_POINT('',(-0.00933080000000005,0.0324998196752637,0.0853092446515657));
#32727=CARTESIAN_POINT('',(-0.0104252652714042,0.0343954891324554,0.0854415363182324));
#32728=CARTESIAN_POINT('',(-0.0115197305428084,0.036291158589647,0.085573827984899));
#32729=CARTESIAN_POINT('',(-0.0134154,0.0373856238610512,0.0857061196515657));
#32730=CARTESIAN_POINT('',(-0.0153110694571917,0.0384800891324553,0.0858384113182323));
#32731=CARTESIAN_POINT('',(-0.0175,0.0384800891324553,0.085970702984899));
#32732=CARTESIAN_POINT('',(-0.0196889305428083,0.0384800891324553,0.0861029946515657));
#32733=CARTESIAN_POINT('',(-0.0215846,0.0373856238610512,0.0862352863182323));
#32734=CARTESIAN_POINT('',(-0.0234802694571917,0.036291158589647,0.0863675779848991));
#32735=CARTESIAN_POINT('',(-0.0245747347285959,0.0343954891324554,0.0864998696515657));
#32736=CARTESIAN_POINT('',(-0.0256692,0.0324998196752637,0.0866321613182323));
#32737=CARTESIAN_POINT('',(-0.0256692,0.0303108891324553,0.086764452984899));
#32738=CARTESIAN_POINT('',(-0.0256692000000001,0.028121958589647,0.0868967446515656));
#32739=CARTESIAN_POINT('',(-0.0245747347285959,0.0262262891324553,0.0870290363182323));
#32740=CARTESIAN_POINT('',(-0.0234802694571917,0.0243306196752637,0.087161327984899));
#32741=CARTESIAN_POINT('',(-0.0215846000000001,0.0232361544038595,0.0872936196515656));
#32742=CARTESIAN_POINT('',(-0.0196889305428084,0.0221416891324554,0.0874259113182324));
#32743=CARTESIAN_POINT('',(-0.0175,0.0221416891324554,0.087558202984899));
#32744=CARTESIAN_POINT('',(-0.0153110694571917,0.0221416891324554,0.0876904946515657));
#32745=CARTESIAN_POINT('',(-0.0134154000000001,0.0232361544038595,0.0878227863182323));
#32746=CARTESIAN_POINT('',(-0.0115197305428084,0.0243306196752637,0.0879550779848991));
#32747=CARTESIAN_POINT('',(-0.0104252652714042,0.0262262891324553,0.0880873696515656));
#32748=CARTESIAN_POINT('',(-0.00933080000000006,0.028121958589647,0.0882196613182324));
#32749=CARTESIAN_POINT('',(-0.00933080000000005,0.0303108891324553,0.088351952984899));
#32750=CARTESIAN_POINT('',(-0.00933080000000005,0.0324998196752637,0.0884842446515657));
#32751=CARTESIAN_POINT('',(-0.0104252652714042,0.0343954891324554,0.0886165363182324));
#32752=CARTESIAN_POINT('',(-0.0115197305428084,0.036291158589647,0.088748827984899));
#32753=CARTESIAN_POINT('',(-0.0134154,0.0373856238610512,0.0888811196515657));
#32754=CARTESIAN_POINT('',(-0.0153110694571917,0.0384800891324553,0.0890134113182324));
#32755=CARTESIAN_POINT('',(-0.0175,0.0384800891324553,0.089145702984899));
#32756=CARTESIAN_POINT('',(-0.0196889305428083,0.0384800891324553,0.0892779946515657));
#32757=CARTESIAN_POINT('',(-0.0215846,0.0373856238610512,0.0894102863182323));
#32758=CARTESIAN_POINT('',(-0.0234802694571917,0.036291158589647,0.089542577984899));
#32759=CARTESIAN_POINT('',(-0.0245747347285959,0.0343954891324554,0.0896748696515657));
#32760=CARTESIAN_POINT('',(-0.0256692,0.0324998196752637,0.0898071613182323));
#32761=CARTESIAN_POINT('',(-0.0256692,0.0303108891324553,0.089939452984899));
#32762=CARTESIAN_POINT('',(-0.0256692000000001,0.028121958589647,0.0900717446515657));
#32763=CARTESIAN_POINT('',(-0.0245747347285959,0.0262262891324553,0.0902040363182323));
#32764=CARTESIAN_POINT('',(-0.0234802694571917,0.0243306196752637,0.090336327984899));
#32765=CARTESIAN_POINT('',(-0.0215846000000001,0.0232361544038595,0.0904686196515656));
#32766=CARTESIAN_POINT('',(-0.0196889305428084,0.0221416891324554,0.0906009113182324));
#32767=CARTESIAN_POINT('',(-0.0175,0.0221416891324554,0.090733202984899));
#32768=CARTESIAN_POINT('',(-0.0153110694571917,0.0221416891324554,0.0908654946515656));
#32769=CARTESIAN_POINT('',(-0.0134154000000001,0.0232361544038595,0.0909977863182323));
#32770=CARTESIAN_POINT('',(-0.0115197305428084,0.0243306196752637,0.091130077984899));
#32771=CARTESIAN_POINT('',(-0.0104252652714042,0.0262262891324553,0.0912623696515656));
#32772=CARTESIAN_POINT('',(-0.00933080000000006,0.028121958589647,0.0913946613182323));
#32773=CARTESIAN_POINT('',(-0.00933080000000005,0.0303108891324553,0.0915269529848989));
#32774=CARTESIAN_POINT('',(-0.00933080000000005,0.0324998196752637,0.0916592446515657));
#32775=CARTESIAN_POINT('',(-0.0104252652714042,0.0343954891324554,0.0917915363182324));
#32776=CARTESIAN_POINT('',(-0.0107406510492572,0.0349417533236814,0.0918296580488028));
#32777=CARTESIAN_POINT('',(-0.0111361563717333,0.0354331272092114,0.0918688959893));
#32778=CARTESIAN_POINT('',(-0.00924790663712744,0.0303108891324553,0.0852757414479046));
#32779=CARTESIAN_POINT('',(-0.00924790663712744,0.0325220308849033,0.0854080331145713));
#32780=CARTESIAN_POINT('',(-0.0103534775133514,0.0344369358138916,0.085540324781238));
#32781=CARTESIAN_POINT('',(-0.0114590483895754,0.03635184074288,0.0856726164479047));
#32782=CARTESIAN_POINT('',(-0.0133739533185637,0.037457411619104,0.0858049081145713));
#32783=CARTESIAN_POINT('',(-0.0152888582475521,0.038562982495328,0.0859371997812381));
#32784=CARTESIAN_POINT('',(-0.0175,0.0385629824953279,0.0860694914479046));
#32785=CARTESIAN_POINT('',(-0.019711141752448,0.038562982495328,0.0862017831145713));
#32786=CARTESIAN_POINT('',(-0.0216260466814364,0.037457411619104,0.0863340747812379));
#32787=CARTESIAN_POINT('',(-0.0235409516104247,0.03635184074288,0.0864663664479047));
#32788=CARTESIAN_POINT('',(-0.0246465224866487,0.0344369358138917,0.0865986581145713));
#32789=CARTESIAN_POINT('',(-0.0257520933628727,0.0325220308849033,0.086730949781238));
#32790=CARTESIAN_POINT('',(-0.0257520933628726,0.0303108891324553,0.0868632414479047));
#32791=CARTESIAN_POINT('',(-0.0257520933628727,0.0280997473800074,0.0869955331145714));
#32792=CARTESIAN_POINT('',(-0.0246465224866487,0.0261848424510191,0.087127824781238));
#32793=CARTESIAN_POINT('',(-0.0235409516104247,0.0242699375220307,0.0872601164479047));
#32794=CARTESIAN_POINT('',(-0.0216260466814364,0.0231643666458067,0.0873924081145713));
#32795=CARTESIAN_POINT('',(-0.019711141752448,0.0220587957695827,0.0875246997812379));
#32796=CARTESIAN_POINT('',(-0.0175,0.0220587957695827,0.0876569914479047));
#32797=CARTESIAN_POINT('',(-0.0152888582475521,0.0220587957695827,0.0877892831145713));
#32798=CARTESIAN_POINT('',(-0.0133739533185638,0.0231643666458067,0.087921574781238));
#32799=CARTESIAN_POINT('',(-0.0114590483895754,0.0242699375220307,0.0880538664479047));
#32800=CARTESIAN_POINT('',(-0.0103534775133514,0.026184842451019,0.0881861581145713));
#32801=CARTESIAN_POINT('',(-0.00924790663712744,0.0280997473800074,0.088318449781238));
#32802=CARTESIAN_POINT('',(-0.00924790663712744,0.0303108891324553,0.0884507414479046));
#32803=CARTESIAN_POINT('',(-0.00924790663712744,0.0325220308849033,0.0885830331145714));
#32804=CARTESIAN_POINT('',(-0.0103534775133514,0.0344369358138916,0.088715324781238));
#32805=CARTESIAN_POINT('',(-0.0114590483895754,0.03635184074288,0.0888476164479046));
#32806=CARTESIAN_POINT('',(-0.0133739533185637,0.037457411619104,0.0889799081145713));
#32807=CARTESIAN_POINT('',(-0.0152888582475521,0.038562982495328,0.089112199781238));
#32808=CARTESIAN_POINT('',(-0.0175,0.0385629824953279,0.0892444914479046));
#32809=CARTESIAN_POINT('',(-0.019711141752448,0.038562982495328,0.0893767831145713));
#32810=CARTESIAN_POINT('',(-0.0216260466814364,0.037457411619104,0.0895090747812379));
#32811=CARTESIAN_POINT('',(-0.0235409516104247,0.03635184074288,0.0896413664479047));
#32812=CARTESIAN_POINT('',(-0.0246465224866487,0.0344369358138917,0.0897736581145713));
#32813=CARTESIAN_POINT('',(-0.0257520933628727,0.0325220308849033,0.0899059497812379));
#32814=CARTESIAN_POINT('',(-0.0257520933628726,0.0303108891324553,0.0900382414479046));
#32815=CARTESIAN_POINT('',(-0.0257520933628727,0.0280997473800074,0.0901705331145713));
#32816=CARTESIAN_POINT('',(-0.0246465224866487,0.0261848424510191,0.0903028247812379));
#32817=CARTESIAN_POINT('',(-0.0235409516104247,0.0242699375220307,0.0904351164479046));
#32818=CARTESIAN_POINT('',(-0.0216260466814364,0.0231643666458067,0.0905674081145714));
#32819=CARTESIAN_POINT('',(-0.019711141752448,0.0220587957695827,0.090699699781238));
#32820=CARTESIAN_POINT('',(-0.0175,0.0220587957695827,0.0908319914479047));
#32821=CARTESIAN_POINT('',(-0.0152888582475521,0.0220587957695827,0.0909642831145713));
#32822=CARTESIAN_POINT('',(-0.0133739533185638,0.0231643666458067,0.091096574781238));
#32823=CARTESIAN_POINT('',(-0.0114590483895754,0.0242699375220307,0.0912288664479047));
#32824=CARTESIAN_POINT('',(-0.0103534775133514,0.026184842451019,0.0913611581145713));
#32825=CARTESIAN_POINT('',(-0.00924790663712744,0.0280997473800074,0.091493449781238));
#32826=CARTESIAN_POINT('',(-0.00924790663712744,0.0303108891324553,0.0916257414479047));
#32827=CARTESIAN_POINT('',(-0.00924790663712744,0.0325220308849033,0.0917580331145713));
#32828=CARTESIAN_POINT('',(-0.0103534775133514,0.0344369358138916,0.091890324781238));
#32829=CARTESIAN_POINT('',(-0.0106720635296278,0.0349887429806633,0.0919284465118084));
#32830=CARTESIAN_POINT('',(-0.0110715820683569,0.0354851028665115,0.0919676844523055));
#32831=CARTESIAN_POINT('',(-0.00912090663712744,0.0303108891324553,0.0852981349744546));
#32832=CARTESIAN_POINT('',(-0.00912090663712744,0.032556060432342,0.0854304266411213));
#32833=CARTESIAN_POINT('',(-0.0102434922870708,0.0345004358138917,0.0855627183077879));
#32834=CARTESIAN_POINT('',(-0.0113660779370141,0.0364448111954412,0.0856950099744546));
#32835=CARTESIAN_POINT('',(-0.0133104533185637,0.0375673968453846,0.0858273016411213));
#32836=CARTESIAN_POINT('',(-0.0152548287001133,0.038689982495328,0.0859595933077879));
#32837=CARTESIAN_POINT('',(-0.0175,0.038689982495328,0.0860918849744546));
#32838=CARTESIAN_POINT('',(-0.0197451712998867,0.038689982495328,0.0862241766411214));
#32839=CARTESIAN_POINT('',(-0.0216895466814364,0.0375673968453846,0.0863564683077879));
#32840=CARTESIAN_POINT('',(-0.023633922062986,0.0364448111954412,0.0864887599744547));
#32841=CARTESIAN_POINT('',(-0.0247565077129293,0.0345004358138917,0.0866210516411213));
#32842=CARTESIAN_POINT('',(-0.0258790933628727,0.0325560604323421,0.086753343307788));
#32843=CARTESIAN_POINT('',(-0.0258790933628727,0.0303108891324553,0.0868856349744546));
#32844=CARTESIAN_POINT('',(-0.0258790933628727,0.0280657178325686,0.0870179266411213));
#32845=CARTESIAN_POINT('',(-0.0247565077129293,0.0261213424510191,0.087150218307788));
#32846=CARTESIAN_POINT('',(-0.023633922062986,0.0241769670694694,0.0872825099744546));
#32847=CARTESIAN_POINT('',(-0.0216895466814364,0.0230543814195261,0.0874148016411213));
#32848=CARTESIAN_POINT('',(-0.0197451712998867,0.0219317957695827,0.087547093307788));
#32849=CARTESIAN_POINT('',(-0.0175,0.0219317957695827,0.0876793849744546));
#32850=CARTESIAN_POINT('',(-0.0152548287001134,0.0219317957695827,0.0878116766411214));
#32851=CARTESIAN_POINT('',(-0.0133104533185637,0.0230543814195261,0.087943968307788));
#32852=CARTESIAN_POINT('',(-0.0113660779370141,0.0241769670694694,0.0880762599744547));
#32853=CARTESIAN_POINT('',(-0.0102434922870708,0.026121342451019,0.0882085516411213));
#32854=CARTESIAN_POINT('',(-0.00912090663712744,0.0280657178325686,0.088340843307788));
#32855=CARTESIAN_POINT('',(-0.00912090663712744,0.0303108891324553,0.0884731349744546));
#32856=CARTESIAN_POINT('',(-0.00912090663712744,0.032556060432342,0.0886054266411213));
#32857=CARTESIAN_POINT('',(-0.0102434922870708,0.0345004358138917,0.0887377183077879));
#32858=CARTESIAN_POINT('',(-0.0113660779370141,0.0364448111954412,0.0888700099744546));
#32859=CARTESIAN_POINT('',(-0.0133104533185637,0.0375673968453846,0.0890023016411213));
#32860=CARTESIAN_POINT('',(-0.0152548287001133,0.038689982495328,0.0891345933077879));
#32861=CARTESIAN_POINT('',(-0.0175,0.038689982495328,0.0892668849744546));
#32862=CARTESIAN_POINT('',(-0.0197451712998867,0.038689982495328,0.0893991766411213));
#32863=CARTESIAN_POINT('',(-0.0216895466814364,0.0375673968453846,0.089531468307788));
#32864=CARTESIAN_POINT('',(-0.023633922062986,0.0364448111954412,0.0896637599744546));
#32865=CARTESIAN_POINT('',(-0.0247565077129293,0.0345004358138917,0.0897960516411213));
#32866=CARTESIAN_POINT('',(-0.0258790933628727,0.0325560604323421,0.089928343307788));
#32867=CARTESIAN_POINT('',(-0.0258790933628727,0.0303108891324553,0.0900606349744546));
#32868=CARTESIAN_POINT('',(-0.0258790933628727,0.0280657178325686,0.0901929266411213));
#32869=CARTESIAN_POINT('',(-0.0247565077129293,0.0261213424510191,0.0903252183077879));
#32870=CARTESIAN_POINT('',(-0.023633922062986,0.0241769670694694,0.0904575099744546));
#32871=CARTESIAN_POINT('',(-0.0216895466814364,0.0230543814195261,0.0905898016411213));
#32872=CARTESIAN_POINT('',(-0.0197451712998867,0.0219317957695827,0.0907220933077879));
#32873=CARTESIAN_POINT('',(-0.0175,0.0219317957695827,0.0908543849744546));
#32874=CARTESIAN_POINT('',(-0.0152548287001134,0.0219317957695827,0.0909866766411213));
#32875=CARTESIAN_POINT('',(-0.0133104533185637,0.0230543814195261,0.0911189683077879));
#32876=CARTESIAN_POINT('',(-0.0113660779370141,0.0241769670694694,0.0912512599744547));
#32877=CARTESIAN_POINT('',(-0.0102434922870708,0.026121342451019,0.0913835516411213));
#32878=CARTESIAN_POINT('',(-0.00912090663712744,0.0280657178325686,0.091515843307788));
#32879=CARTESIAN_POINT('',(-0.00912090663712744,0.0303108891324553,0.0916481349744546));
#32880=CARTESIAN_POINT('',(-0.00912090663712744,0.032556060432342,0.0917804266411213));
#32881=CARTESIAN_POINT('',(-0.0102434922870708,0.0345004358138917,0.0919127183077879));
#32882=CARTESIAN_POINT('',(-0.010566981353069,0.0350607353118935,0.0919508400383583));
#32883=CARTESIAN_POINT('',(-0.0109726484958174,0.035564734193416,0.0919900779788555));
#32884=CARTESIAN_POINT('',(-0.00912090663712744,0.0303108891324553,0.0852981349744546));
#32885=CARTESIAN_POINT('',(-0.00912090663712744,0.032556060432342,0.0854304266411213));
#32886=CARTESIAN_POINT('',(-0.0102434922870708,0.0345004358138917,0.0855627183077879));
#32887=CARTESIAN_POINT('',(-0.0113660779370141,0.0364448111954412,0.0856950099744546));
#32888=CARTESIAN_POINT('',(-0.0133104533185637,0.0375673968453846,0.0858273016411213));
#32889=CARTESIAN_POINT('',(-0.0152548287001133,0.038689982495328,0.0859595933077879));
#32890=CARTESIAN_POINT('',(-0.0175,0.038689982495328,0.0860918849744546));
#32891=CARTESIAN_POINT('',(-0.0197451712998867,0.038689982495328,0.0862241766411212));
#32892=CARTESIAN_POINT('',(-0.0216895466814364,0.0375673968453846,0.0863564683077879));
#32893=CARTESIAN_POINT('',(-0.023633922062986,0.0364448111954412,0.0864887599744547));
#32894=CARTESIAN_POINT('',(-0.0247565077129293,0.0345004358138917,0.0866210516411213));
#32895=CARTESIAN_POINT('',(-0.0258790933628727,0.0325560604323421,0.086753343307788));
#32896=CARTESIAN_POINT('',(-0.0258790933628727,0.0303108891324553,0.0868856349744546));
#32897=CARTESIAN_POINT('',(-0.0258790933628727,0.0280657178325686,0.0870179266411213));
#32898=CARTESIAN_POINT('',(-0.0247565077129293,0.0261213424510191,0.087150218307788));
#32899=CARTESIAN_POINT('',(-0.023633922062986,0.0241769670694694,0.0872825099744546));
#32900=CARTESIAN_POINT('',(-0.0216895466814364,0.0230543814195261,0.0874148016411213));
#32901=CARTESIAN_POINT('',(-0.0197451712998867,0.0219317957695827,0.087547093307788));
#32902=CARTESIAN_POINT('',(-0.0175,0.0219317957695827,0.0876793849744546));
#32903=CARTESIAN_POINT('',(-0.0152548287001134,0.0219317957695827,0.0878116766411214));
#32904=CARTESIAN_POINT('',(-0.0133104533185637,0.0230543814195261,0.087943968307788));
#32905=CARTESIAN_POINT('',(-0.0113660779370141,0.0241769670694694,0.0880762599744547));
#32906=CARTESIAN_POINT('',(-0.0102434922870708,0.026121342451019,0.0882085516411213));
#32907=CARTESIAN_POINT('',(-0.00912090663712744,0.0280657178325686,0.088340843307788));
#32908=CARTESIAN_POINT('',(-0.00912090663712744,0.0303108891324553,0.0884731349744546));
#32909=CARTESIAN_POINT('',(-0.00912090663712744,0.032556060432342,0.0886054266411213));
#32910=CARTESIAN_POINT('',(-0.0102434922870708,0.0345004358138917,0.0887377183077879));
#32911=CARTESIAN_POINT('',(-0.0113660779370141,0.0364448111954412,0.0888700099744546));
#32912=CARTESIAN_POINT('',(-0.0133104533185637,0.0375673968453846,0.0890023016411213));
#32913=CARTESIAN_POINT('',(-0.0152548287001133,0.038689982495328,0.0891345933077879));
#32914=CARTESIAN_POINT('',(-0.0175,0.038689982495328,0.0892668849744546));
#32915=CARTESIAN_POINT('',(-0.0197451712998867,0.038689982495328,0.0893991766411213));
#32916=CARTESIAN_POINT('',(-0.0216895466814364,0.0375673968453846,0.089531468307788));
#32917=CARTESIAN_POINT('',(-0.023633922062986,0.0364448111954412,0.0896637599744546));
#32918=CARTESIAN_POINT('',(-0.0247565077129293,0.0345004358138917,0.0897960516411213));
#32919=CARTESIAN_POINT('',(-0.0258790933628727,0.0325560604323421,0.089928343307788));
#32920=CARTESIAN_POINT('',(-0.0258790933628727,0.0303108891324553,0.0900606349744546));
#32921=CARTESIAN_POINT('',(-0.0258790933628727,0.0280657178325686,0.0901929266411213));
#32922=CARTESIAN_POINT('',(-0.0247565077129293,0.0261213424510191,0.0903252183077879));
#32923=CARTESIAN_POINT('',(-0.023633922062986,0.0241769670694694,0.0904575099744546));
#32924=CARTESIAN_POINT('',(-0.0216895466814364,0.0230543814195261,0.0905898016411213));
#32925=CARTESIAN_POINT('',(-0.0197451712998867,0.0219317957695827,0.0907220933077879));
#32926=CARTESIAN_POINT('',(-0.0175,0.0219317957695827,0.0908543849744546));
#32927=CARTESIAN_POINT('',(-0.0152548287001134,0.0219317957695827,0.0909866766411213));
#32928=CARTESIAN_POINT('',(-0.0133104533185637,0.0230543814195261,0.0911189683077879));
#32929=CARTESIAN_POINT('',(-0.0113660779370141,0.0241769670694694,0.0912512599744547));
#32930=CARTESIAN_POINT('',(-0.0102434922870708,0.026121342451019,0.0913835516411213));
#32931=CARTESIAN_POINT('',(-0.00912090663712744,0.0280657178325686,0.091515843307788));
#32932=CARTESIAN_POINT('',(-0.00912090663712744,0.0303108891324553,0.0916481349744546));
#32933=CARTESIAN_POINT('',(-0.00912090663712743,0.0307461291971821,0.091673780515873));
#32934=CARTESIAN_POINT('',(-0.00916600081685451,0.0311790269090008,0.0917));
#32935=CARTESIAN_POINT('',(-0.00916600081685452,0.0311790269090009,0.0917));
#32936=CARTESIAN_POINT('',(-0.00916600081685452,0.0311790269090008,0.0917));
#32937=CARTESIAN_POINT('',(-0.00923799565048493,0.0313347702922195,0.0917));
#32938=CARTESIAN_POINT('',(-0.00931002513253627,0.0316684151962386,0.0916999999999999));
#32939=CARTESIAN_POINT('',(-0.0095023502836293,0.0323207574022983,0.0917000000000003));
#32940=CARTESIAN_POINT('',(-0.00977549559735775,0.0331234551269965,0.0916999999999976));
#32941=CARTESIAN_POINT('',(-0.0102085406903454,0.034051613931461,0.0917000000000007));
#32942=CARTESIAN_POINT('',(-0.0105596013841118,0.0346332630059237,0.0917));
#32943=CARTESIAN_POINT('',(-0.0107517314949501,0.0349148766241576,0.0917));
#32944=CARTESIAN_POINT('',(-0.00912090663712744,0.0303108891324553,0.0852981349744546));
#32945=CARTESIAN_POINT('',(-0.00912090663712744,0.032556060432342,0.0854304266411213));
#32946=CARTESIAN_POINT('',(-0.0102434922870708,0.0345004358138917,0.0855627183077879));
#32947=CARTESIAN_POINT('',(-0.0113660779370141,0.0364448111954412,0.0856950099744546));
#32948=CARTESIAN_POINT('',(-0.0133104533185637,0.0375673968453846,0.0858273016411213));
#32949=CARTESIAN_POINT('',(-0.0152548287001133,0.038689982495328,0.0859595933077879));
#32950=CARTESIAN_POINT('',(-0.0175,0.038689982495328,0.0860918849744546));
#32951=CARTESIAN_POINT('',(-0.0197451712998867,0.038689982495328,0.0862241766411214));
#32952=CARTESIAN_POINT('',(-0.0216895466814364,0.0375673968453846,0.0863564683077879));
#32953=CARTESIAN_POINT('',(-0.023633922062986,0.0364448111954412,0.0864887599744547));
#32954=CARTESIAN_POINT('',(-0.0247565077129293,0.0345004358138917,0.0866210516411213));
#32955=CARTESIAN_POINT('',(-0.0258790933628727,0.0325560604323421,0.086753343307788));
#32956=CARTESIAN_POINT('',(-0.0258790933628727,0.0303108891324553,0.0868856349744546));
#32957=CARTESIAN_POINT('',(-0.0258790933628727,0.0280657178325686,0.0870179266411213));
#32958=CARTESIAN_POINT('',(-0.0247565077129293,0.0261213424510191,0.087150218307788));
#32959=CARTESIAN_POINT('',(-0.023633922062986,0.0241769670694694,0.0872825099744546));
#32960=CARTESIAN_POINT('',(-0.0216895466814364,0.0230543814195261,0.0874148016411213));
#32961=CARTESIAN_POINT('',(-0.0197451712998867,0.0219317957695827,0.087547093307788));
#32962=CARTESIAN_POINT('',(-0.0175,0.0219317957695827,0.0876793849744546));
#32963=CARTESIAN_POINT('',(-0.0152548287001134,0.0219317957695827,0.0878116766411214));
#32964=CARTESIAN_POINT('',(-0.0133104533185637,0.0230543814195261,0.087943968307788));
#32965=CARTESIAN_POINT('',(-0.0113660779370141,0.0241769670694694,0.0880762599744547));
#32966=CARTESIAN_POINT('',(-0.0102434922870708,0.0261213424510191,0.0882085516411213));
#32967=CARTESIAN_POINT('',(-0.00912090663712744,0.0280657178325686,0.088340843307788));
#32968=CARTESIAN_POINT('',(-0.00912090663712744,0.0303108891324553,0.0884731349744546));
#32969=CARTESIAN_POINT('',(-0.00912090663712744,0.032556060432342,0.0886054266411213));
#32970=CARTESIAN_POINT('',(-0.0102434922870708,0.0345004358138917,0.0887377183077879));
#32971=CARTESIAN_POINT('',(-0.0113660779370141,0.0364448111954412,0.0888700099744546));
#32972=CARTESIAN_POINT('',(-0.0133104533185637,0.0375673968453846,0.0890023016411213));
#32973=CARTESIAN_POINT('',(-0.0152548287001133,0.038689982495328,0.0891345933077879));
#32974=CARTESIAN_POINT('',(-0.0175,0.038689982495328,0.0892668849744546));
#32975=CARTESIAN_POINT('',(-0.0197451712998867,0.038689982495328,0.0893991766411213));
#32976=CARTESIAN_POINT('',(-0.0216895466814364,0.0375673968453846,0.089531468307788));
#32977=CARTESIAN_POINT('',(-0.023633922062986,0.0364448111954412,0.0896637599744546));
#32978=CARTESIAN_POINT('',(-0.0247565077129293,0.0345004358138917,0.0897960516411213));
#32979=CARTESIAN_POINT('',(-0.0258790933628727,0.0325560604323421,0.089928343307788));
#32980=CARTESIAN_POINT('',(-0.0258790933628727,0.0303108891324553,0.0900606349744546));
#32981=CARTESIAN_POINT('',(-0.0258790933628727,0.0280657178325686,0.0901929266411213));
#32982=CARTESIAN_POINT('',(-0.0247565077129293,0.0261213424510191,0.0903252183077879));
#32983=CARTESIAN_POINT('',(-0.023633922062986,0.0241769670694694,0.0904575099744546));
#32984=CARTESIAN_POINT('',(-0.0216895466814364,0.0230543814195261,0.0905898016411213));
#32985=CARTESIAN_POINT('',(-0.0197451712998867,0.0219317957695827,0.0907220933077879));
#32986=CARTESIAN_POINT('',(-0.0175,0.0219317957695827,0.0908543849744546));
#32987=CARTESIAN_POINT('',(-0.0152548287001134,0.0219317957695827,0.0909866766411213));
#32988=CARTESIAN_POINT('',(-0.0133104533185637,0.0230543814195261,0.0911189683077879));
#32989=CARTESIAN_POINT('',(-0.0113660779370141,0.0241769670694694,0.0912512599744547));
#32990=CARTESIAN_POINT('',(-0.0102434922870708,0.0261213424510191,0.0913835516411213));
#32991=CARTESIAN_POINT('',(-0.00912090663712744,0.0280657178325686,0.091515843307788));
#32992=CARTESIAN_POINT('',(-0.00912090663712744,0.0303108891324553,0.0916481349744546));
#32993=CARTESIAN_POINT('',(-0.00912090663712744,0.0310669305934274,0.091692683016266));
#32994=CARTESIAN_POINT('',(-0.00925623934052464,0.0318107610513275,0.091738648225955));
#32995=CARTESIAN_POINT('',(-0.00847389336287264,0.0303108891324553,0.0854122208715823));
#32996=CARTESIAN_POINT('',(-0.00847389336287265,0.0327294271166708,0.085544512538249));
#32997=CARTESIAN_POINT('',(-0.00968316235498038,0.0348239424510191,0.0856768042049156));
#32998=CARTESIAN_POINT('',(-0.0108924313470881,0.0369184577853673,0.0858090958715823));
#32999=CARTESIAN_POINT('',(-0.0129869466814363,0.038127726777475,0.0859413875382489));
#33000=CARTESIAN_POINT('',(-0.0150814620157846,0.0393369957695828,0.0860736792049156));
#33001=CARTESIAN_POINT('',(-0.0175,0.0393369957695828,0.0862059708715822));
#33002=CARTESIAN_POINT('',(-0.0199185379842156,0.0393369957695828,0.086338262538249));
#33003=CARTESIAN_POINT('',(-0.0220130533185638,0.038127726777475,0.0864705542049156));
#33004=CARTESIAN_POINT('',(-0.024107568652912,0.0369184577853673,0.0866028458715823));
#33005=CARTESIAN_POINT('',(-0.0253168376450197,0.0348239424510191,0.0867351375382489));
#33006=CARTESIAN_POINT('',(-0.0265261066371274,0.0327294271166708,0.0868674292049156));
#33007=CARTESIAN_POINT('',(-0.0265261066371274,0.0303108891324553,0.0869997208715823));
#33008=CARTESIAN_POINT('',(-0.0265261066371274,0.0278923511482398,0.0871320125382489));
#33009=CARTESIAN_POINT('',(-0.0253168376450197,0.0257978358138917,0.0872643042049156));
#33010=CARTESIAN_POINT('',(-0.024107568652912,0.0237033204795434,0.0873965958715823));
#33011=CARTESIAN_POINT('',(-0.0220130533185638,0.0224940514874357,0.0875288875382489));
#33012=CARTESIAN_POINT('',(-0.0199185379842156,0.021284782495328,0.0876611792049156));
#33013=CARTESIAN_POINT('',(-0.0175,0.021284782495328,0.0877934708715823));
#33014=CARTESIAN_POINT('',(-0.0150814620157846,0.0212847824953279,0.087925762538249));
#33015=CARTESIAN_POINT('',(-0.0129869466814363,0.0224940514874356,0.0880580542049156));
#33016=CARTESIAN_POINT('',(-0.0108924313470881,0.0237033204795434,0.0881903458715823));
#33017=CARTESIAN_POINT('',(-0.00968316235498039,0.0257978358138917,0.0883226375382489));
#33018=CARTESIAN_POINT('',(-0.00847389336287265,0.0278923511482398,0.0884549292049156));
#33019=CARTESIAN_POINT('',(-0.00847389336287264,0.0303108891324553,0.0885872208715823));
#33020=CARTESIAN_POINT('',(-0.00847389336287265,0.0327294271166708,0.0887195125382489));
#33021=CARTESIAN_POINT('',(-0.00968316235498038,0.0348239424510191,0.0888518042049156));
#33022=CARTESIAN_POINT('',(-0.0108924313470881,0.0369184577853673,0.0889840958715822));
#33023=CARTESIAN_POINT('',(-0.0129869466814363,0.038127726777475,0.0891163875382489));
#33024=CARTESIAN_POINT('',(-0.0150814620157846,0.0393369957695828,0.0892486792049156));
#33025=CARTESIAN_POINT('',(-0.0175,0.0393369957695828,0.0893809708715822));
#33026=CARTESIAN_POINT('',(-0.0199185379842156,0.0393369957695828,0.089513262538249));
#33027=CARTESIAN_POINT('',(-0.0220130533185638,0.038127726777475,0.0896455542049156));
#33028=CARTESIAN_POINT('',(-0.024107568652912,0.0369184577853673,0.0897778458715823));
#33029=CARTESIAN_POINT('',(-0.0253168376450197,0.0348239424510191,0.0899101375382489));
#33030=CARTESIAN_POINT('',(-0.0265261066371274,0.0327294271166708,0.0900424292049156));
#33031=CARTESIAN_POINT('',(-0.0265261066371274,0.0303108891324553,0.0901747208715823));
#33032=CARTESIAN_POINT('',(-0.0265261066371274,0.0278923511482398,0.0903070125382489));
#33033=CARTESIAN_POINT('',(-0.0253168376450197,0.0257978358138917,0.0904393042049156));
#33034=CARTESIAN_POINT('',(-0.024107568652912,0.0237033204795434,0.0905715958715823));
#33035=CARTESIAN_POINT('',(-0.0220130533185638,0.0224940514874357,0.0907038875382489));
#33036=CARTESIAN_POINT('',(-0.0199185379842156,0.021284782495328,0.0908361792049157));
#33037=CARTESIAN_POINT('',(-0.0175,0.021284782495328,0.0909684708715822));
#33038=CARTESIAN_POINT('',(-0.0150814620157846,0.0212847824953279,0.091100762538249));
#33039=CARTESIAN_POINT('',(-0.0129869466814363,0.0224940514874356,0.0912330542049156));
#33040=CARTESIAN_POINT('',(-0.0108924313470881,0.0237033204795434,0.0913653458715823));
#33041=CARTESIAN_POINT('',(-0.00968316235498039,0.0257978358138917,0.0914976375382489));
#33042=CARTESIAN_POINT('',(-0.00847389336287265,0.0278923511482398,0.0916299292049156));
#33043=CARTESIAN_POINT('',(-0.00847389336287264,0.0303108891324553,0.0917622208715822));
#33044=CARTESIAN_POINT('',(-0.00847389336287264,0.0311253102820108,0.0918067689133936));
#33045=CARTESIAN_POINT('',(-0.00861967612951019,0.0319265775244429,0.0918527341230826));
#33046=CARTESIAN_POINT('',(-0.00847389336287264,0.0303108891324553,0.0854122208715823));
#33047=CARTESIAN_POINT('',(-0.00847389336287265,0.0327294271166708,0.085544512538249));
#33048=CARTESIAN_POINT('',(-0.00968316235498038,0.0348239424510191,0.0856768042049156));
#33049=CARTESIAN_POINT('',(-0.0108924313470881,0.0369184577853673,0.0858090958715823));
#33050=CARTESIAN_POINT('',(-0.0129869466814363,0.038127726777475,0.0859413875382489));
#33051=CARTESIAN_POINT('',(-0.0150814620157846,0.0393369957695828,0.0860736792049156));
#33052=CARTESIAN_POINT('',(-0.0175,0.0393369957695828,0.0862059708715822));
#33053=CARTESIAN_POINT('',(-0.0199185379842156,0.0393369957695828,0.086338262538249));
#33054=CARTESIAN_POINT('',(-0.0220130533185638,0.038127726777475,0.0864705542049156));
#33055=CARTESIAN_POINT('',(-0.024107568652912,0.0369184577853673,0.0866028458715823));
#33056=CARTESIAN_POINT('',(-0.0253168376450197,0.0348239424510191,0.0867351375382489));
#33057=CARTESIAN_POINT('',(-0.0265261066371274,0.0327294271166708,0.0868674292049156));
#33058=CARTESIAN_POINT('',(-0.0265261066371274,0.0303108891324553,0.0869997208715823));
#33059=CARTESIAN_POINT('',(-0.0265261066371274,0.0278923511482398,0.0871320125382489));
#33060=CARTESIAN_POINT('',(-0.0253168376450197,0.0257978358138917,0.0872643042049156));
#33061=CARTESIAN_POINT('',(-0.024107568652912,0.0237033204795434,0.0873965958715823));
#33062=CARTESIAN_POINT('',(-0.0220130533185638,0.0224940514874357,0.0875288875382489));
#33063=CARTESIAN_POINT('',(-0.0199185379842156,0.021284782495328,0.0876611792049155));
#33064=CARTESIAN_POINT('',(-0.0175,0.021284782495328,0.0877934708715823));
#33065=CARTESIAN_POINT('',(-0.0150814620157846,0.021284782495328,0.087925762538249));
#33066=CARTESIAN_POINT('',(-0.0129869466814363,0.0224940514874356,0.0880580542049156));
#33067=CARTESIAN_POINT('',(-0.0108924313470881,0.0237033204795434,0.0881903458715823));
#33068=CARTESIAN_POINT('',(-0.00968316235498039,0.0257978358138917,0.0883226375382489));
#33069=CARTESIAN_POINT('',(-0.00847389336287265,0.0278923511482398,0.0884549292049156));
#33070=CARTESIAN_POINT('',(-0.00847389336287264,0.0303108891324553,0.0885872208715823));
#33071=CARTESIAN_POINT('',(-0.00847389336287265,0.0327294271166708,0.088719512538249));
#33072=CARTESIAN_POINT('',(-0.00968316235498038,0.0348239424510191,0.0888518042049156));
#33073=CARTESIAN_POINT('',(-0.0108924313470881,0.0369184577853673,0.0889840958715823));
#33074=CARTESIAN_POINT('',(-0.0129869466814363,0.038127726777475,0.0891163875382489));
#33075=CARTESIAN_POINT('',(-0.0150814620157846,0.0393369957695828,0.0892486792049156));
#33076=CARTESIAN_POINT('',(-0.0175,0.0393369957695828,0.0893809708715822));
#33077=CARTESIAN_POINT('',(-0.0199185379842156,0.0393369957695828,0.089513262538249));
#33078=CARTESIAN_POINT('',(-0.0220130533185638,0.038127726777475,0.0896455542049156));
#33079=CARTESIAN_POINT('',(-0.024107568652912,0.0369184577853673,0.0897778458715823));
#33080=CARTESIAN_POINT('',(-0.0253168376450197,0.0348239424510191,0.0899101375382489));
#33081=CARTESIAN_POINT('',(-0.0265261066371274,0.0327294271166708,0.0900424292049156));
#33082=CARTESIAN_POINT('',(-0.0265261066371274,0.0303108891324553,0.0901747208715823));
#33083=CARTESIAN_POINT('',(-0.0265261066371274,0.0278923511482398,0.0903070125382489));
#33084=CARTESIAN_POINT('',(-0.0253168376450197,0.0257978358138917,0.0904393042049156));
#33085=CARTESIAN_POINT('',(-0.024107568652912,0.0237033204795434,0.0905715958715823));
#33086=CARTESIAN_POINT('',(-0.0220130533185638,0.0224940514874357,0.0907038875382489));
#33087=CARTESIAN_POINT('',(-0.0199185379842156,0.021284782495328,0.0908361792049157));
#33088=CARTESIAN_POINT('',(-0.0175,0.021284782495328,0.0909684708715822));
#33089=CARTESIAN_POINT('',(-0.0150814620157846,0.021284782495328,0.091100762538249));
#33090=CARTESIAN_POINT('',(-0.0129869466814363,0.0224940514874356,0.0912330542049156));
#33091=CARTESIAN_POINT('',(-0.0108924313470881,0.0237033204795434,0.0913653458715823));
#33092=CARTESIAN_POINT('',(-0.00968316235498039,0.0257978358138917,0.0914976375382489));
#33093=CARTESIAN_POINT('',(-0.00876991648182173,0.027379624066005,0.091597544853681));
#33094=CARTESIAN_POINT('',(-0.00854350778716387,0.0291920288779395,0.0917000000000564));
#33095=CARTESIAN_POINT('',(-0.0085435077872263,0.0291920288774397,0.0917000000000283));
#33096=CARTESIAN_POINT('',(-0.00854350778722381,0.0291920288774402,0.0917));
#33097=CARTESIAN_POINT('',(-0.00867070228446611,0.0298765386535114,0.0917));
#33098=CARTESIAN_POINT('',(-0.008873827876199,0.0305469815250745,0.0917));
#33099=CARTESIAN_POINT('',(-0.00916600081685446,0.0311790269090009,0.0917));
#33100=CARTESIAN_POINT('',(-0.00847389336287264,0.0303108891324553,0.0854122208715823));
#33101=CARTESIAN_POINT('',(-0.00847389336287265,0.0327294271166708,0.085544512538249));
#33102=CARTESIAN_POINT('',(-0.00968316235498038,0.0348239424510191,0.0856768042049156));
#33103=CARTESIAN_POINT('',(-0.0108924313470881,0.0369184577853673,0.0858090958715823));
#33104=CARTESIAN_POINT('',(-0.0129869466814363,0.038127726777475,0.0859413875382489));
#33105=CARTESIAN_POINT('',(-0.0150814620157846,0.0393369957695828,0.0860736792049156));
#33106=CARTESIAN_POINT('',(-0.0175,0.0393369957695828,0.0862059708715822));
#33107=CARTESIAN_POINT('',(-0.0199185379842156,0.0393369957695828,0.086338262538249));
#33108=CARTESIAN_POINT('',(-0.0220130533185638,0.038127726777475,0.0864705542049156));
#33109=CARTESIAN_POINT('',(-0.024107568652912,0.0369184577853673,0.0866028458715823));
#33110=CARTESIAN_POINT('',(-0.0253168376450197,0.0348239424510191,0.0867351375382489));
#33111=CARTESIAN_POINT('',(-0.0265261066371274,0.0327294271166708,0.0868674292049156));
#33112=CARTESIAN_POINT('',(-0.0265261066371274,0.0303108891324553,0.0869997208715823));
#33113=CARTESIAN_POINT('',(-0.0265261066371274,0.0278923511482399,0.0871320125382489));
#33114=CARTESIAN_POINT('',(-0.0253168376450197,0.0257978358138917,0.0872643042049156));
#33115=CARTESIAN_POINT('',(-0.024107568652912,0.0237033204795435,0.0873965958715823));
#33116=CARTESIAN_POINT('',(-0.0220130533185638,0.0224940514874357,0.0875288875382489));
#33117=CARTESIAN_POINT('',(-0.0199185379842156,0.021284782495328,0.0876611792049156));
#33118=CARTESIAN_POINT('',(-0.0175,0.021284782495328,0.0877934708715823));
#33119=CARTESIAN_POINT('',(-0.0150814620157846,0.0212847824953279,0.087925762538249));
#33120=CARTESIAN_POINT('',(-0.0129869466814364,0.0224940514874356,0.0880580542049156));
#33121=CARTESIAN_POINT('',(-0.0108924313470881,0.0237033204795434,0.0881903458715823));
#33122=CARTESIAN_POINT('',(-0.00968316235498039,0.0257978358138917,0.0883226375382489));
#33123=CARTESIAN_POINT('',(-0.00847389336287265,0.0278923511482398,0.0884549292049156));
#33124=CARTESIAN_POINT('',(-0.00847389336287264,0.0303108891324553,0.0885872208715823));
#33125=CARTESIAN_POINT('',(-0.00847389336287265,0.0327294271166708,0.0887195125382489));
#33126=CARTESIAN_POINT('',(-0.00968316235498038,0.0348239424510191,0.0888518042049156));
#33127=CARTESIAN_POINT('',(-0.0108924313470881,0.0369184577853673,0.0889840958715822));
#33128=CARTESIAN_POINT('',(-0.0129869466814363,0.038127726777475,0.0891163875382489));
#33129=CARTESIAN_POINT('',(-0.0150814620157846,0.0393369957695828,0.0892486792049156));
#33130=CARTESIAN_POINT('',(-0.0175,0.0393369957695828,0.0893809708715822));
#33131=CARTESIAN_POINT('',(-0.0199185379842156,0.0393369957695828,0.089513262538249));
#33132=CARTESIAN_POINT('',(-0.0220130533185638,0.038127726777475,0.0896455542049156));
#33133=CARTESIAN_POINT('',(-0.024107568652912,0.0369184577853673,0.0897778458715823));
#33134=CARTESIAN_POINT('',(-0.0253168376450197,0.0348239424510191,0.0899101375382489));
#33135=CARTESIAN_POINT('',(-0.0265261066371274,0.0327294271166708,0.0900424292049156));
#33136=CARTESIAN_POINT('',(-0.0265261066371274,0.0303108891324553,0.0901747208715823));
#33137=CARTESIAN_POINT('',(-0.0265261066371274,0.0278923511482399,0.0903070125382489));
#33138=CARTESIAN_POINT('',(-0.0253168376450197,0.0257978358138917,0.0904393042049156));
#33139=CARTESIAN_POINT('',(-0.024107568652912,0.0237033204795435,0.0905715958715823));
#33140=CARTESIAN_POINT('',(-0.0220130533185638,0.0224940514874357,0.0907038875382489));
#33141=CARTESIAN_POINT('',(-0.0199185379842156,0.021284782495328,0.0908361792049157));
#33142=CARTESIAN_POINT('',(-0.0175,0.021284782495328,0.0909684708715822));
#33143=CARTESIAN_POINT('',(-0.0150814620157846,0.0212847824953279,0.091100762538249));
#33144=CARTESIAN_POINT('',(-0.0129869466814364,0.0224940514874356,0.0912330542049156));
#33145=CARTESIAN_POINT('',(-0.0108924313470881,0.0237033204795434,0.0913653458715823));
#33146=CARTESIAN_POINT('',(-0.00968316235498039,0.0257978358138917,0.0914976375382489));
#33147=CARTESIAN_POINT('',(-0.00859351540386823,0.0276851596955304,0.09161684278719));
#33148=CARTESIAN_POINT('',(-0.00848507467546628,0.0298617539435922,0.091737489735644));
#33149=CARTESIAN_POINT('',(-0.00834689336287265,0.0303108891324553,0.0854346143981323));
#33150=CARTESIAN_POINT('',(-0.00834689336287264,0.0327634566641096,0.0855669060647989));
#33151=CARTESIAN_POINT('',(-0.00957317712869975,0.0348874424510191,0.0856991977314656));
#33152=CARTESIAN_POINT('',(-0.0107994608945269,0.0370114282379285,0.0858314893981323));
#33153=CARTESIAN_POINT('',(-0.0129234466814363,0.0382377120037556,0.0859637810647989));
#33154=CARTESIAN_POINT('',(-0.0150474324683458,0.0394639957695828,0.0860960727314655));
#33155=CARTESIAN_POINT('',(-0.0175,0.0394639957695827,0.0862283643981323));
#33156=CARTESIAN_POINT('',(-0.0199525675316543,0.0394639957695828,0.0863606560647989));
#33157=CARTESIAN_POINT('',(-0.0220765533185638,0.0382377120037556,0.0864929477314656));
#33158=CARTESIAN_POINT('',(-0.0242005391054732,0.0370114282379285,0.0866252393981323));
#33159=CARTESIAN_POINT('',(-0.0254268228713003,0.0348874424510191,0.0867575310647989));
#33160=CARTESIAN_POINT('',(-0.0266531066371274,0.0327634566641096,0.0868898227314656));
#33161=CARTESIAN_POINT('',(-0.0266531066371274,0.0303108891324553,0.0870221143981322));
#33162=CARTESIAN_POINT('',(-0.0266531066371274,0.0278583216008011,0.087154406064799));
#33163=CARTESIAN_POINT('',(-0.0254268228713003,0.0257343358138916,0.0872866977314655));
#33164=CARTESIAN_POINT('',(-0.0242005391054732,0.0236103500269822,0.0874189893981322));
#33165=CARTESIAN_POINT('',(-0.0220765533185638,0.022384066261155,0.0875512810647989));
#33166=CARTESIAN_POINT('',(-0.0199525675316543,0.021157782495328,0.0876835727314656));
#33167=CARTESIAN_POINT('',(-0.0175,0.0211577824953279,0.0878158643981322));
#33168=CARTESIAN_POINT('',(-0.0150474324683458,0.021157782495328,0.0879481560647989));
#33169=CARTESIAN_POINT('',(-0.0129234466814363,0.022384066261155,0.0880804477314655));
#33170=CARTESIAN_POINT('',(-0.0107994608945269,0.0236103500269822,0.0882127393981323));
#33171=CARTESIAN_POINT('',(-0.00957317712869976,0.0257343358138916,0.0883450310647989));
#33172=CARTESIAN_POINT('',(-0.00834689336287266,0.0278583216008011,0.0884773227314656));
#33173=CARTESIAN_POINT('',(-0.00834689336287265,0.0303108891324553,0.0886096143981323));
#33174=CARTESIAN_POINT('',(-0.00834689336287264,0.0327634566641096,0.088741906064799));
#33175=CARTESIAN_POINT('',(-0.00957317712869975,0.0348874424510191,0.0888741977314656));
#33176=CARTESIAN_POINT('',(-0.0107994608945269,0.0370114282379285,0.0890064893981322));
#33177=CARTESIAN_POINT('',(-0.0129234466814363,0.0382377120037556,0.0891387810647989));
#33178=CARTESIAN_POINT('',(-0.0150474324683458,0.0394639957695828,0.0892710727314656));
#33179=CARTESIAN_POINT('',(-0.0175,0.0394639957695827,0.0894033643981323));
#33180=CARTESIAN_POINT('',(-0.0199525675316543,0.0394639957695828,0.0895356560647989));
#33181=CARTESIAN_POINT('',(-0.0220765533185638,0.0382377120037556,0.0896679477314656));
#33182=CARTESIAN_POINT('',(-0.0242005391054732,0.0370114282379285,0.0898002393981323));
#33183=CARTESIAN_POINT('',(-0.0254268228713003,0.0348874424510191,0.0899325310647989));
#33184=CARTESIAN_POINT('',(-0.0266531066371274,0.0327634566641096,0.0900648227314657));
#33185=CARTESIAN_POINT('',(-0.0266531066371274,0.0303108891324553,0.0901971143981322));
#33186=CARTESIAN_POINT('',(-0.0266531066371274,0.0278583216008011,0.0903294060647989));
#33187=CARTESIAN_POINT('',(-0.0254268228713003,0.0257343358138916,0.0904616977314656));
#33188=CARTESIAN_POINT('',(-0.0242005391054732,0.0236103500269822,0.0905939893981322));
#33189=CARTESIAN_POINT('',(-0.0220765533185638,0.022384066261155,0.0907262810647989));
#33190=CARTESIAN_POINT('',(-0.0199525675316543,0.021157782495328,0.0908585727314656));
#33191=CARTESIAN_POINT('',(-0.0175,0.0211577824953279,0.0909908643981322));
#33192=CARTESIAN_POINT('',(-0.0150474324683458,0.021157782495328,0.091123156064799));
#33193=CARTESIAN_POINT('',(-0.0129234466814363,0.022384066261155,0.0912554477314655));
#33194=CARTESIAN_POINT('',(-0.0107994608945269,0.0236103500269822,0.0913877393981323));
#33195=CARTESIAN_POINT('',(-0.00957317712869976,0.0257343358138916,0.0915200310647988));
#33196=CARTESIAN_POINT('',(-0.00846819852149771,0.0276482149028423,0.09163923631374));
#33197=CARTESIAN_POINT('',(-0.00835823199985392,0.0298554344781484,0.091759883262194));
#33198=CARTESIAN_POINT('',(-0.00826400000000004,0.0303108891324553,0.0855334028611379));
#33199=CARTESIAN_POINT('',(-0.00826400000000004,0.0327856678737492,0.0856656945278046));
#33200=CARTESIAN_POINT('',(-0.00950138937064697,0.0349288891324553,0.0857979861944712));
#33201=CARTESIAN_POINT('',(-0.0107387787412939,0.0370721103911615,0.0859302778611379));
#33202=CARTESIAN_POINT('',(-0.012882,0.0383094997618084,0.0860625695278045));
#33203=CARTESIAN_POINT('',(-0.0150252212587062,0.0395468891324554,0.0861948611944711));
#33204=CARTESIAN_POINT('',(-0.0175,0.0395468891324554,0.0863271528611379));
#33205=CARTESIAN_POINT('',(-0.0199747787412939,0.0395468891324554,0.0864594445278045));
#33206=CARTESIAN_POINT('',(-0.022118,0.0383094997618084,0.0865917361944712));
#33207=CARTESIAN_POINT('',(-0.0242612212587062,0.0370721103911615,0.0867240278611378));
#33208=CARTESIAN_POINT('',(-0.0254986106293532,0.0349288891324553,0.0868563195278045));
#33209=CARTESIAN_POINT('',(-0.0267360000000001,0.0327856678737492,0.0869886111944712));
#33210=CARTESIAN_POINT('',(-0.0267360000000001,0.0303108891324553,0.0871209028611378));
#33211=CARTESIAN_POINT('',(-0.0267360000000001,0.0278361103911615,0.0872531945278046));
#33212=CARTESIAN_POINT('',(-0.0254986106293532,0.0256928891324553,0.0873854861944711));
#33213=CARTESIAN_POINT('',(-0.0242612212587062,0.0235496678737492,0.0875177778611379));
#33214=CARTESIAN_POINT('',(-0.022118,0.0223122785031023,0.0876500695278045));
#33215=CARTESIAN_POINT('',(-0.0199747787412939,0.0210748891324553,0.0877823611944713));
#33216=CARTESIAN_POINT('',(-0.0175,0.0210748891324553,0.0879146528611379));
#33217=CARTESIAN_POINT('',(-0.0150252212587062,0.0210748891324553,0.0880469445278045));
#33218=CARTESIAN_POINT('',(-0.012882,0.0223122785031023,0.0881792361944712));
#33219=CARTESIAN_POINT('',(-0.0107387787412939,0.0235496678737492,0.0883115278611379));
#33220=CARTESIAN_POINT('',(-0.00950138937064697,0.0256928891324553,0.0884438195278046));
#33221=CARTESIAN_POINT('',(-0.00826400000000005,0.0278361103911615,0.0885761111944712));
#33222=CARTESIAN_POINT('',(-0.00826400000000004,0.0303108891324553,0.0887084028611379));
#33223=CARTESIAN_POINT('',(-0.00826400000000004,0.0327856678737492,0.0888406945278046));
#33224=CARTESIAN_POINT('',(-0.00950138937064697,0.0349288891324553,0.0889729861944712));
#33225=CARTESIAN_POINT('',(-0.0107387787412939,0.0370721103911615,0.0891052778611379));
#33226=CARTESIAN_POINT('',(-0.012882,0.0383094997618084,0.0892375695278045));
#33227=CARTESIAN_POINT('',(-0.0150252212587062,0.0395468891324554,0.0893698611944712));
#33228=CARTESIAN_POINT('',(-0.0175,0.0395468891324554,0.0895021528611379));
#33229=CARTESIAN_POINT('',(-0.0199747787412939,0.0395468891324554,0.0896344445278045));
#33230=CARTESIAN_POINT('',(-0.022118,0.0383094997618084,0.0897667361944712));
#33231=CARTESIAN_POINT('',(-0.0242612212587062,0.0370721103911615,0.0898990278611379));
#33232=CARTESIAN_POINT('',(-0.0254986106293532,0.0349288891324553,0.0900313195278045));
#33233=CARTESIAN_POINT('',(-0.0267360000000001,0.0327856678737492,0.0901636111944712));
#33234=CARTESIAN_POINT('',(-0.0267360000000001,0.0303108891324553,0.0902959028611378));
#33235=CARTESIAN_POINT('',(-0.0267360000000001,0.0278361103911615,0.0904281945278046));
#33236=CARTESIAN_POINT('',(-0.0254986106293532,0.0256928891324553,0.0905604861944712));
#33237=CARTESIAN_POINT('',(-0.0242612212587062,0.0235496678737492,0.0906927778611378));
#33238=CARTESIAN_POINT('',(-0.022118,0.0223122785031023,0.0908250695278045));
#33239=CARTESIAN_POINT('',(-0.0199747787412939,0.0210748891324553,0.0909573611944712));
#33240=CARTESIAN_POINT('',(-0.0175,0.0210748891324553,0.0910896528611378));
#33241=CARTESIAN_POINT('',(-0.0150252212587062,0.0210748891324553,0.0912219445278045));
#33242=CARTESIAN_POINT('',(-0.012882,0.0223122785031023,0.0913542361944712));
#33243=CARTESIAN_POINT('',(-0.0107387787412939,0.0235496678737492,0.0914865278611379));
#33244=CARTESIAN_POINT('',(-0.00950138937064697,0.0256928891324553,0.0916188195278046));
#33245=CARTESIAN_POINT('',(-0.00838640373563626,0.0276241009020033,0.0917380247767456));
#33246=CARTESIAN_POINT('',(-0.00827544132318252,0.0298513097400209,0.0918586717251997));
#33247=CARTESIAN_POINT('',(-0.008264,0.0303108891324553,0.0856623620408474));
#33248=CARTESIAN_POINT('',(-0.00826400000000004,0.0327856678737492,0.0857946537075141));
#33249=CARTESIAN_POINT('',(-0.00950138937064697,0.0349288891324553,0.0859269453741807));
#33250=CARTESIAN_POINT('',(-0.0107387787412939,0.0370721103911615,0.0860592370408474));
#33251=CARTESIAN_POINT('',(-0.012882,0.0383094997618084,0.086191528707514));
#33252=CARTESIAN_POINT('',(-0.0150252212587062,0.0395468891324554,0.0863238203741807));
#33253=CARTESIAN_POINT('',(-0.0175,0.0395468891324554,0.0864561120408473));
#33254=CARTESIAN_POINT('',(-0.0199747787412939,0.0395468891324554,0.086588403707514));
#33255=CARTESIAN_POINT('',(-0.022118,0.0383094997618084,0.0867206953741807));
#33256=CARTESIAN_POINT('',(-0.0242612212587062,0.0370721103911615,0.0868529870408474));
#33257=CARTESIAN_POINT('',(-0.0254986106293531,0.0349288891324553,0.086985278707514));
#33258=CARTESIAN_POINT('',(-0.0267360000000001,0.0327856678737492,0.0871175703741807));
#33259=CARTESIAN_POINT('',(-0.026736,0.0303108891324553,0.0872498620408474));
#33260=CARTESIAN_POINT('',(-0.0267360000000001,0.0278361103911615,0.087382153707514));
#33261=CARTESIAN_POINT('',(-0.0254986106293531,0.0256928891324554,0.0875144453741807));
#33262=CARTESIAN_POINT('',(-0.0242612212587062,0.0235496678737492,0.0876467370408473));
#33263=CARTESIAN_POINT('',(-0.022118,0.0223122785031023,0.087779028707514));
#33264=CARTESIAN_POINT('',(-0.0199747787412939,0.0210748891324554,0.0879113203741807));
#33265=CARTESIAN_POINT('',(-0.0175,0.0210748891324553,0.0880436120408474));
#33266=CARTESIAN_POINT('',(-0.0150252212587062,0.0210748891324553,0.088175903707514));
#33267=CARTESIAN_POINT('',(-0.012882,0.0223122785031023,0.0883081953741807));
#33268=CARTESIAN_POINT('',(-0.0107387787412939,0.0235496678737492,0.0884404870408474));
#33269=CARTESIAN_POINT('',(-0.00950138937064697,0.0256928891324554,0.088572778707514));
#33270=CARTESIAN_POINT('',(-0.00826400000000005,0.0278361103911615,0.0887050703741807));
#33271=CARTESIAN_POINT('',(-0.008264,0.0303108891324553,0.0888373620408473));
#33272=CARTESIAN_POINT('',(-0.00826400000000004,0.0327856678737492,0.088969653707514));
#33273=CARTESIAN_POINT('',(-0.00950138937064697,0.0349288891324553,0.0891019453741807));
#33274=CARTESIAN_POINT('',(-0.0107387787412939,0.0370721103911615,0.0892342370408473));
#33275=CARTESIAN_POINT('',(-0.012882,0.0383094997618084,0.089366528707514));
#33276=CARTESIAN_POINT('',(-0.0150252212587062,0.0395468891324554,0.0894988203741807));
#33277=CARTESIAN_POINT('',(-0.0175,0.0395468891324554,0.0896311120408473));
#33278=CARTESIAN_POINT('',(-0.0199747787412939,0.0395468891324554,0.0897634037075141));
#33279=CARTESIAN_POINT('',(-0.022118,0.0383094997618084,0.0898956953741807));
#33280=CARTESIAN_POINT('',(-0.0242612212587062,0.0370721103911615,0.0900279870408474));
#33281=CARTESIAN_POINT('',(-0.0254986106293531,0.0349288891324553,0.090160278707514));
#33282=CARTESIAN_POINT('',(-0.0267360000000001,0.0327856678737492,0.0902925703741807));
#33283=CARTESIAN_POINT('',(-0.026736,0.0303108891324553,0.0904248620408473));
#33284=CARTESIAN_POINT('',(-0.0267360000000001,0.0278361103911615,0.090557153707514));
#33285=CARTESIAN_POINT('',(-0.0254986106293531,0.0256928891324554,0.0906894453741807));
#33286=CARTESIAN_POINT('',(-0.0242612212587062,0.0235496678737492,0.0908217370408474));
#33287=CARTESIAN_POINT('',(-0.022118,0.0223122785031023,0.090954028707514));
#33288=CARTESIAN_POINT('',(-0.0199747787412939,0.0210748891324554,0.0910863203741807));
#33289=CARTESIAN_POINT('',(-0.0175,0.0210748891324553,0.0912186120408473));
#33290=CARTESIAN_POINT('',(-0.0150252212587062,0.0210748891324553,0.0913509037075141));
#33291=CARTESIAN_POINT('',(-0.012882,0.0223122785031023,0.0914831953741807));
#33292=CARTESIAN_POINT('',(-0.0107387787412939,0.0235496678737492,0.0916154870408474));
#33293=CARTESIAN_POINT('',(-0.00950138937064697,0.0256928891324554,0.091747778707514));
#33294=CARTESIAN_POINT('',(-0.00838640373563626,0.0276241009020033,0.0918669839564551));
#33295=CARTESIAN_POINT('',(-0.00827544132318248,0.0298513097400209,0.0919876309049091));
#33296=CARTESIAN_POINT('',(-0.00997922046889643,0.0249497725281897,0.0917));
#33297=CARTESIAN_POINT('',(-0.00975815321976537,0.0252598941250487,0.0917));
#33298=CARTESIAN_POINT('',(-0.00935880114911267,0.02590976181805,0.0917000000000014));
#33299=CARTESIAN_POINT('',(-0.008904491714687,0.0269479762400238,0.091699999999995));
#33300=CARTESIAN_POINT('',(-0.00864371501392561,0.0278685853564734,0.0917000000000148));
#33301=CARTESIAN_POINT('',(-0.00854235352036947,0.0286227935316649,0.0916999999999744));
#33302=CARTESIAN_POINT('',(-0.00850783637718163,0.0290000596521613,0.0917000000000565));
#33303=CARTESIAN_POINT('',(-0.00854350778706608,0.0291920288774134,0.0917000000000565));
#33304=CARTESIAN_POINT('',(-0.008264,0.0303108891324553,0.0856623620408474));
#33305=CARTESIAN_POINT('',(-0.00826400000000004,0.0327856678737492,0.0857946537075141));
#33306=CARTESIAN_POINT('',(-0.00950138937064697,0.0349288891324553,0.0859269453741807));
#33307=CARTESIAN_POINT('',(-0.0107387787412939,0.0370721103911615,0.0860592370408474));
#33308=CARTESIAN_POINT('',(-0.012882,0.0383094997618084,0.086191528707514));
#33309=CARTESIAN_POINT('',(-0.0150252212587062,0.0395468891324554,0.0863238203741807));
#33310=CARTESIAN_POINT('',(-0.0175,0.0395468891324554,0.0864561120408473));
#33311=CARTESIAN_POINT('',(-0.0199747787412939,0.0395468891324554,0.086588403707514));
#33312=CARTESIAN_POINT('',(-0.022118,0.0383094997618084,0.0867206953741807));
#33313=CARTESIAN_POINT('',(-0.0242612212587062,0.0370721103911615,0.0868529870408474));
#33314=CARTESIAN_POINT('',(-0.0254986106293531,0.0349288891324553,0.086985278707514));
#33315=CARTESIAN_POINT('',(-0.0267360000000001,0.0327856678737491,0.0871175703741807));
#33316=CARTESIAN_POINT('',(-0.026736,0.0303108891324553,0.0872498620408474));
#33317=CARTESIAN_POINT('',(-0.026736,0.0303108891324553,0.0872498620408474));
#33318=CARTESIAN_POINT('',(-0.026736,0.0303108891324553,0.0872498620408473));
#33319=CARTESIAN_POINT('',(-0.0267360000000001,0.0278361103911614,0.087382153707514));
#33320=CARTESIAN_POINT('',(-0.0254986106293531,0.0256928891324554,0.0875144453741807));
#33321=CARTESIAN_POINT('',(-0.0242612212587062,0.0235496678737492,0.0876467370408474));
#33322=CARTESIAN_POINT('',(-0.022118,0.0223122785031023,0.087779028707514));
#33323=CARTESIAN_POINT('',(-0.0199747787412939,0.0210748891324553,0.0879113203741807));
#33324=CARTESIAN_POINT('',(-0.0175,0.0210748891324553,0.0880436120408474));
#33325=CARTESIAN_POINT('',(-0.0150252212587062,0.0210748891324553,0.088175903707514));
#33326=CARTESIAN_POINT('',(-0.012882,0.0223122785031023,0.0883081953741807));
#33327=CARTESIAN_POINT('',(-0.0107387787412939,0.0235496678737492,0.0884404870408474));
#33328=CARTESIAN_POINT('',(-0.00950138937064697,0.0256928891324554,0.088572778707514));
#33329=CARTESIAN_POINT('',(-0.00826400000000006,0.0278361103911614,0.0887050703741806));
#33330=CARTESIAN_POINT('',(-0.008264,0.0303108891324553,0.0888373620408473));
#33331=CARTESIAN_POINT('',(-0.008264,0.0303108891324553,0.0888373620408473));
#33332=CARTESIAN_POINT('',(-0.008264,0.0303108891324553,0.0888373620408474));
#33333=CARTESIAN_POINT('',(-0.00826400000000003,0.0327856678737492,0.088969653707514));
#33334=CARTESIAN_POINT('',(-0.00950138937064697,0.0349288891324553,0.0891019453741807));
#33335=CARTESIAN_POINT('',(-0.0107387787412939,0.0370721103911615,0.0892342370408473));
#33336=CARTESIAN_POINT('',(-0.012882,0.0383094997618084,0.089366528707514));
#33337=CARTESIAN_POINT('',(-0.0150252212587062,0.0395468891324554,0.0894988203741807));
#33338=CARTESIAN_POINT('',(-0.0175,0.0395468891324554,0.0896311120408473));
#33339=CARTESIAN_POINT('',(-0.0199747787412939,0.0395468891324554,0.0897634037075141));
#33340=CARTESIAN_POINT('',(-0.022118,0.0383094997618084,0.0898956953741807));
#33341=CARTESIAN_POINT('',(-0.0242612212587062,0.0370721103911615,0.0900279870408474));
#33342=CARTESIAN_POINT('',(-0.0254986106293531,0.0349288891324553,0.090160278707514));
#33343=CARTESIAN_POINT('',(-0.0267360000000001,0.0327856678737492,0.0902925703741807));
#33344=CARTESIAN_POINT('',(-0.026736,0.0303108891324553,0.0904248620408474));
#33345=CARTESIAN_POINT('',(-0.026736,0.0303108891324553,0.0904248620408473));
#33346=CARTESIAN_POINT('',(-0.026736,0.0303108891324553,0.0904248620408473));
#33347=CARTESIAN_POINT('',(-0.0267360000000001,0.0278361103911614,0.090557153707514));
#33348=CARTESIAN_POINT('',(-0.0254986106293531,0.0256928891324554,0.0906894453741807));
#33349=CARTESIAN_POINT('',(-0.0242612212587062,0.0235496678737492,0.0908217370408473));
#33350=CARTESIAN_POINT('',(-0.022118,0.0223122785031023,0.090954028707514));
#33351=CARTESIAN_POINT('',(-0.0217493769033143,0.0220994538590013,0.0909767821976795));
#33352=CARTESIAN_POINT('',(-0.0213627414806,0.0219214359766142,0.0909999999999999));
#33353=CARTESIAN_POINT('',(-0.00832342471144782,0.0303108891324553,0.085499093987987));
#33354=CARTESIAN_POINT('',(-0.0175,0.0303108891324553,0.0917));
#33355=CARTESIAN_POINT('',(-0.026736,0.0303108891324553,0.119284271247462));
#33356=CARTESIAN_POINT('',(-0.00832342471144782,0.0303108891324553,0.085499093987987));
#33357=CARTESIAN_POINT('',(-0.026736,0.0303108891324553,0.0935156110802982));
#33358=CARTESIAN_POINT('',(-0.026736,0.0303108891324559,0.093));
#33359=CARTESIAN_POINT('',(-0.026736,0.0303108891324553,0.0935998620408474));
#33360=CARTESIAN_POINT('',(-0.0175,0.0303108891324553,0.093));
#33361=CARTESIAN_POINT('',(-0.0256696111607028,0.0303108891274052,0.092999999842707));
#33362=CARTESIAN_POINT('',(-0.0258790933628727,0.0303108891324553,0.0932356349744546));
#33363=CARTESIAN_POINT('',(-0.0257663813457609,0.0303108891324553,0.0932157608047877));
#33364=CARTESIAN_POINT('',(-0.025676150498743,0.0303108891324553,0.093114263076951));
#33365=CARTESIAN_POINT('',(-0.0256696145170245,0.0303108891324553,0.0929999990740266));
#33366=CARTESIAN_POINT('',(-0.0258790933628727,0.0303108891324553,0.0932356349744546));
#33367=CARTESIAN_POINT('',(-0.0262026,0.0303108891324553,0.0932926779230184));
#33368=CARTESIAN_POINT('',(-0.0265261066371274,0.0303108891324553,0.0933497208715823));
#33369=CARTESIAN_POINT('',(-0.026482,0.0303108891324553,0.0935998620408473));
#33370=CARTESIAN_POINT('',(-0.0208098178710173,0.0387082522117494,0.0927462298951597));
#33371=CARTESIAN_POINT('',(-0.0214329756260445,0.0384626347894019,0.092783915922311));
#33372=CARTESIAN_POINT('',(-0.0220130533185638,0.038127726777475,0.0928205542049156));
#33373=CARTESIAN_POINT('',(-0.024107568652912,0.0369184577853673,0.0929528458715823));
#33374=CARTESIAN_POINT('',(-0.0253168376450197,0.0348239424510191,0.0930851375382489));
#33375=CARTESIAN_POINT('',(-0.0265261066371274,0.0327294271166708,0.0932174292049156));
#33376=CARTESIAN_POINT('',(-0.0265261066371274,0.0303108891324553,0.0933497208715822));
#33377=CARTESIAN_POINT('',(-0.0208563879910611,0.0388264056032331,0.0927686234217097));
#33378=CARTESIAN_POINT('',(-0.0214883137607009,0.0385773322708358,0.092806309448861));
#33379=CARTESIAN_POINT('',(-0.0220765533185638,0.0382377120037556,0.0928429477314656));
#33380=CARTESIAN_POINT('',(-0.0242005391054732,0.0370114282379285,0.0929752393981322));
#33381=CARTESIAN_POINT('',(-0.0254268228713003,0.0348874424510191,0.0931075310647989));
#33382=CARTESIAN_POINT('',(-0.0266531066371274,0.0327634566641096,0.0932398227314656));
#33383=CARTESIAN_POINT('',(-0.0266531066371274,0.0303108891324553,0.0933721143981322));
#33384=CARTESIAN_POINT('',(-0.0208867844781463,0.0389035247524842,0.0928674118847153));
#33385=CARTESIAN_POINT('',(-0.0215244331628801,0.0386521957350017,0.0929050979118666));
#33386=CARTESIAN_POINT('',(-0.022118,0.0383094997618084,0.0929417361944712));
#33387=CARTESIAN_POINT('',(-0.0242612212587062,0.0370721103911615,0.0930740278611379));
#33388=CARTESIAN_POINT('',(-0.0254986106293532,0.0349288891324553,0.0932063195278045));
#33389=CARTESIAN_POINT('',(-0.0267360000000001,0.0327856678737492,0.0933386111944712));
#33390=CARTESIAN_POINT('',(-0.0267360000000001,0.0303108891324553,0.0934709028611378));
#33391=CARTESIAN_POINT('',(-0.0208867844781462,0.0389035247524842,0.0929963710644248));
#33392=CARTESIAN_POINT('',(-0.0215244331628801,0.0386521957350017,0.0930340570915761));
#33393=CARTESIAN_POINT('',(-0.022118,0.0383094997618084,0.0930706953741807));
#33394=CARTESIAN_POINT('',(-0.0242612212587062,0.0370721103911615,0.0932029870408474));
#33395=CARTESIAN_POINT('',(-0.0254986106293531,0.0349288891324553,0.093335278707514));
#33396=CARTESIAN_POINT('',(-0.0267360000000001,0.0327856678737492,0.0934675703741807));
#33397=CARTESIAN_POINT('',(-0.026736,0.0303108891324553,0.0935998620408473));
#33398=CARTESIAN_POINT('',(-0.02444400516351,0.0360772912441661,0.093));
#33399=CARTESIAN_POINT('',(-0.0249336325663123,0.0354876731170587,0.0930432156508374));
#33400=CARTESIAN_POINT('',(-0.0253168376450197,0.0348239424510191,0.0930851375382489));
#33401=CARTESIAN_POINT('',(-0.0265261066371274,0.0327294271166708,0.0932174292049156));
#33402=CARTESIAN_POINT('',(-0.0265261066371274,0.0303108891324553,0.0933497208715822));
#33403=CARTESIAN_POINT('',(-0.0244440051635101,0.0360772912441661,0.093));
#33404=CARTESIAN_POINT('',(-0.0244440051635101,0.0360772912441661,0.093));
#33405=CARTESIAN_POINT('',(-0.0243715488570553,0.0362568694047589,0.093));
#33406=CARTESIAN_POINT('',(-0.0241354058133839,0.0365621839766753,0.0930000000000197));
#33407=CARTESIAN_POINT('',(-0.023645216577888,0.0371396946954097,0.0929999999999886));
#33408=CARTESIAN_POINT('',(-0.0229302657159657,0.037774800623597,0.0930000000000038));
#33409=CARTESIAN_POINT('',(-0.0219837917740965,0.0384065294749524,0.0929999999999989));
#33410=CARTESIAN_POINT('',(-0.0213022700815101,0.0387365742102223,0.093));
#33411=CARTESIAN_POINT('',(-0.0209481246951914,0.0388790938502718,0.093));
#33412=CARTESIAN_POINT('',(-0.0209481246951914,0.0388790938502718,0.093));
#33413=CARTESIAN_POINT('',(-0.0209481246951913,0.0388790938502718,0.093));
#33414=CARTESIAN_POINT('',(-0.0215531734565775,0.0386356025186988,0.0930358311040996));
#33415=CARTESIAN_POINT('',(-0.022118,0.0383094997618084,0.0930706953741807));
#33416=CARTESIAN_POINT('',(-0.0242612212587062,0.0370721103911615,0.0932029870408474));
#33417=CARTESIAN_POINT('',(-0.0254986106293531,0.0349288891324553,0.093335278707514));
#33418=CARTESIAN_POINT('',(-0.0267360000000001,0.0327856678737492,0.0934675703741807));
#33419=CARTESIAN_POINT('',(-0.026736,0.0303108891324553,0.0935998620408473));
#33420=CARTESIAN_POINT('',(-0.0239208501740996,0.0356883202624204,0.0928831027918458));
#33421=CARTESIAN_POINT('',(-0.0245484726165509,0.0349389160261808,0.0929425276418814));
#33422=CARTESIAN_POINT('',(-0.0250350358572561,0.0340954493917498,0.0929985783868971));
#33423=CARTESIAN_POINT('',(-0.0257040731328745,0.0322584121122458,0.093117439776351));
#33424=CARTESIAN_POINT('',(-0.0258752064163071,0.0312736120738746,0.0931781969911814));
#33425=CARTESIAN_POINT('',(-0.0258752064163071,0.0303108891324553,0.0932349496009025));
#33426=CARTESIAN_POINT('',(-0.024087187678253,0.0358276271218958,0.0929213598820724));
#33427=CARTESIAN_POINT('',(-0.0247310692059964,0.0350588089409482,0.092980784732108));
#33428=CARTESIAN_POINT('',(-0.0252302372751709,0.0341934915965639,0.0930368354771236));
#33429=CARTESIAN_POINT('',(-0.0259166065220384,0.0323088643269769,0.0931556968665776));
#33430=CARTESIAN_POINT('',(-0.0260921731565806,0.031298552218392,0.093216454081408));
#33431=CARTESIAN_POINT('',(-0.0260921731565806,0.0303108891324553,0.0932732066911291));
#33432=CARTESIAN_POINT('',(-0.0242535251824065,0.0359669339813711,0.0929596169722989));
#33433=CARTESIAN_POINT('',(-0.0249136657954419,0.0351787018557156,0.0930190418223346));
#33434=CARTESIAN_POINT('',(-0.0254254386930857,0.0342915338013779,0.0930750925673502));
#33435=CARTESIAN_POINT('',(-0.0261291399112023,0.032359316541708,0.0931939539568041));
#33436=CARTESIAN_POINT('',(-0.026309139896854,0.0313234923629095,0.0932547111716345));
#33437=CARTESIAN_POINT('',(-0.026309139896854,0.0303108891324553,0.0933114637813556));
#33438=CARTESIAN_POINT('',(-0.0244198626865599,0.0361062408408464,0.0929978740625255));
#33439=CARTESIAN_POINT('',(-0.0250962623848874,0.0352985947704829,0.0930572989125611));
#33440=CARTESIAN_POINT('',(-0.0256206401110005,0.034389576006192,0.0931133496575767));
#33441=CARTESIAN_POINT('',(-0.0263416733003661,0.032409768756439,0.0932322110470307));
#33442=CARTESIAN_POINT('',(-0.0265261066371274,0.0313484325074269,0.0932929682618611));
#33443=CARTESIAN_POINT('',(-0.0265261066371274,0.0303108891324553,0.0933497208715822));
#33444=CARTESIAN_POINT('',(-0.0174703820743504,0.0303029630442298,0.0931033427178736));
#33445=CARTESIAN_POINT('',(-0.0249879614552658,0.0340711602434389,0.0929999999999981));
#33446=CARTESIAN_POINT('',(-0.0249879614552682,0.0340711602434402,0.093));
#33447=CARTESIAN_POINT('',(-0.0248918662163977,0.0347594676980157,0.093));
#33448=CARTESIAN_POINT('',(-0.0247040214997711,0.0354328579618956,0.093));
#33449=CARTESIAN_POINT('',(-0.0244440051635101,0.0360772912441661,0.093));
#33450=CARTESIAN_POINT('',(-0.0247904637453546,0.0339973612414627,0.0927610698531875));
#33451=CARTESIAN_POINT('',(-0.0256695127292157,0.032258930959684,0.0928803654994113));
#33452=CARTESIAN_POINT('',(-0.0256695127292157,0.0303108891324553,0.0929980941481212));
#33453=CARTESIAN_POINT('',(-0.0247959527978272,0.0340001368178254,0.0928849080708547));
#33454=CARTESIAN_POINT('',(-0.0256756636251824,0.0322603976570276,0.0930042037170785));
#33455=CARTESIAN_POINT('',(-0.0256756636251824,0.0303108891324553,0.0931219323657884));
#33456=CARTESIAN_POINT('',(-0.0248692608122447,0.0340372055091949,0.0929772252855233));
#33457=CARTESIAN_POINT('',(-0.0257578107666889,0.0322799858592798,0.0930965209317472));
#33458=CARTESIAN_POINT('',(-0.0257578107666889,0.0303108891324553,0.093214249580457));
#33459=CARTESIAN_POINT('',(-0.0249774932613182,0.0340919339762356,0.0929986106795209));
#33460=CARTESIAN_POINT('',(-0.0258790933628727,0.0323089060137751,0.0931179063257447));
#33461=CARTESIAN_POINT('',(-0.0258790933628727,0.0303108891324553,0.0932356349744546));
#33462=CARTESIAN_POINT('',(-0.0256696128552748,0.0303108891215471,0.0929999998244189));
#33463=CARTESIAN_POINT('',(-0.0256707191428082,0.0306309045519008,0.0929999998244189));
#33464=CARTESIAN_POINT('',(-0.02563945609545,0.0312704222456812,0.0930000000816386));
#33465=CARTESIAN_POINT('',(-0.0254980011493608,0.0322205044648445,0.0929999999776367));
#33466=CARTESIAN_POINT('',(-0.0253010899158569,0.0329961385140969,0.0930000000027779));
#33467=CARTESIAN_POINT('',(-0.0251208175046229,0.0336100287475924,0.0929999999994444));
#33468=CARTESIAN_POINT('',(-0.025010301394035,0.0339111445489435,0.093));
#33469=CARTESIAN_POINT('',(-0.0249879614552709,0.0340711602434405,0.093));
#33470=CARTESIAN_POINT('',(-0.0175,0.0303108891324553,0.0867173896326779));
#33471=CARTESIAN_POINT('',(-0.0175,0.0303108891324553,0.093));
#33472=CARTESIAN_POINT('',(-0.0175,0.0303108891324553,0.083));
#33473=CARTESIAN_POINT('',(-0.0175,0.0303108891324553,0.083));
#33474=CARTESIAN_POINT('',(-0.0175,0.0303108891324553,0.083));
#33475=CARTESIAN_POINT('',(-0.0055,0.0303108891324553,0.083));
#33476=CARTESIAN_POINT('',(-0.0175,0.0303108891324553,0.093));
#33477=CARTESIAN_POINT('',(-0.0175,0.0303108891324553,0.093));
#33478=CARTESIAN_POINT('',(-0.0055,0.0303108891324553,0.093));
#33479=CARTESIAN_POINT('',(-0.0175,0.0303108891324553,0.091));
#33480=CARTESIAN_POINT('',(-0.0175,0.0303108891324553,0.091));
#33481=CARTESIAN_POINT('',(-0.0175,0.0303108891324553,0.091));
#33482=CARTESIAN_POINT('',(-0.0075,0.0303108891324553,0.091));
#33483=CARTESIAN_POINT('',(-0.0175,0.0303108891324553,0.091));
#33484=CARTESIAN_POINT('',(-0.0175,0.0303108891324553,0.091));
#33485=CARTESIAN_POINT('',(-0.0255,0.0303108891324553,0.091));
#33486=CARTESIAN_POINT('',(-0.0175,0.0303108891324553,0.0917));
#33487=CARTESIAN_POINT('',(-0.0175,0.0303108891324553,0.0917));
#33488=CARTESIAN_POINT('',(-0.0275,0.0303108891324553,0.0917));
#33489=CARTESIAN_POINT('',(-0.0175,0.0303108891324553,0.0917));
#33490=CARTESIAN_POINT('',(-0.0255,0.0303108891324553,0.0917));
#33491=CARTESIAN_POINT('',(-0.0175,0.0303108891324553,0.083));
#33492=CARTESIAN_POINT('',(-0.0175,0.0303108891324553,0.0917));
#33493=CARTESIAN_POINT('',(-0.0175,0.0303108891324553,0.119284271247462));
#33494=CARTESIAN_POINT('',(-0.0175,0.0303108891324553,0.093));
#33495=CARTESIAN_POINT('',(-8.67361737988404E-19,0.,0.001));
#33496=CARTESIAN_POINT('',(-0.00125,0.,-0.0300923697749146));
#33497=CARTESIAN_POINT('',(0.,0.,-0.0300923697749146));
#33498=CARTESIAN_POINT('',(-0.00125,0.,-0.0300923697749146));
#33499=CARTESIAN_POINT('',(0.,0.,-0.0300923697749146));
#33500=CARTESIAN_POINT('',(-0.00325,0.,-0.0300923697749146));
#33501=CARTESIAN_POINT('',(-0.0189,0.,0.0230923697749146));
#33502=CARTESIAN_POINT('',(0.,0.,0.0230923697749146));
#33503=CARTESIAN_POINT('',(-0.012,0.,0.0230923697749146));
#33504=CARTESIAN_POINT('',(0.,0.,0.0230923697749146));
#33505=CARTESIAN_POINT('',(-0.0189,0.,0.0230923697749146));
#33506=CARTESIAN_POINT('',(-0.012,0.,0.0250923697749146));
#33507=CARTESIAN_POINT('',(0.,0.,0.0250923697749146));
#33508=CARTESIAN_POINT('',(0.013,0.,0.0250923697749146));
#33509=CARTESIAN_POINT('',(0.,0.,0.0250923697749146));
#33510=CARTESIAN_POINT('',(0.0187,0.,0.0250923697749146));
#33511=CARTESIAN_POINT('',(-0.012,0.,0.0300923697749146));
#33512=CARTESIAN_POINT('',(0.,0.,0.0300923697749146));
#33513=CARTESIAN_POINT('',(0.0102,0.,0.0300923697749146));
#33514=CARTESIAN_POINT('',(0.,0.,0.0300923697749146));
#33515=CARTESIAN_POINT('',(0.0118,0.,0.0300923697749146));
#33516=CARTESIAN_POINT('',(0.,0.,-0.0300923697749146));
#33517=CARTESIAN_POINT('',(0.,0.,0.0260923697749146));
#33518=CARTESIAN_POINT('',(0.012,0.,0.0260923697749146));
#33519=CARTESIAN_POINT('',(0.,0.,0.0298923697749146));
#33520=CARTESIAN_POINT('',(0.012,0.,0.0298923697749146));
#33521=CARTESIAN_POINT('',(0.,0.,-0.0300923697749146));
#33522=CARTESIAN_POINT('',(0.,0.,0.0248923697749146));
#33523=CARTESIAN_POINT('',(0.0189,0.,0.0248923697749146));
#33524=CARTESIAN_POINT('',(0.,0.,-0.0300923697749146));
#33525=CARTESIAN_POINT('',(0.,0.,-0.0162074226868757));
#33526=CARTESIAN_POINT('',(-0.012,0.,-0.0162074226868757));
#33527=CARTESIAN_POINT('',(0.,0.,-0.0162074226868757));
#33528=CARTESIAN_POINT('',(0.,0.,-0.0190265005492334));
#33529=CARTESIAN_POINT('',(-0.010026060429977,0.,-0.0190265005492334));
#33530=CARTESIAN_POINT('',(0.,0.,-0.0208087445646827));
#33531=CARTESIAN_POINT('',(0.,0.,-0.0208087445646827));
#33532=CARTESIAN_POINT('',(-0.00512938524157182,0.,-0.0208087445646827));
#33533=CARTESIAN_POINT('',(0.,0.,-0.0234927848513341));
#33534=CARTESIAN_POINT('',(0.,0.,-0.0234927848513341));
#33535=CARTESIAN_POINT('',(-0.00325,0.,-0.0234927848513341));
#33536=CARTESIAN_POINT('',(0.,0.,-0.0300923697749146));
#33537=CARTESIAN_POINT('',(0.,0.,-0.0300923697749146));
#33538=CARTESIAN_POINT('',(0.,0.,-0.0224076685637936));
#33539=CARTESIAN_POINT('',(0.00125,0.,-0.0224076685637936));
#33540=CARTESIAN_POINT('',(0.,0.,-0.0194083294882633));
#33541=CARTESIAN_POINT('',(0.,0.,-0.0196666071357353));
#33542=CARTESIAN_POINT('',(-0.00294853728586081,0.,-0.0196666071357353));
#33543=CARTESIAN_POINT('',(0.,0.,-0.0218340921274426));
#33544=CARTESIAN_POINT('',(-0.00143084795571101,0.,-0.0218340921274426));
#33545=CARTESIAN_POINT('',(0.,0.,-0.0176355706936178));
#33546=CARTESIAN_POINT('',(0.,0.,-0.0176355706936178));
#33547=CARTESIAN_POINT('',(-0.008,0.,-0.0176355706936178));
#33548=CARTESIAN_POINT('',(0.,0.,-0.0193004909513005));
#33549=CARTESIAN_POINT('',(-0.00342566918682414,0.,-0.0193004909513005));
#33550=CARTESIAN_POINT('',(0.,0.,-0.0147792746801336));
#33551=CARTESIAN_POINT('',(0.,0.,-0.0147792746801336));
#33552=CARTESIAN_POINT('',(-0.01,0.,-0.0147792746801336));
#33553=CARTESIAN_POINT('',(0.,0.,-0.0300923697749146));
#33554=CARTESIAN_POINT('',(0.,0.,0.0298923697749146));
#33555=CARTESIAN_POINT('',(0.01,0.,0.0298923697749146));
#33556=CARTESIAN_POINT('',(0.,0.,0.0260923697749146));
#33557=CARTESIAN_POINT('',(0.,0.,0.0248923697749146));
#33558=CARTESIAN_POINT('',(0.,0.,0.0298923697749146));
#33559=CARTESIAN_POINT('',(0.,0.,0.0298923697749146));
#33560=CARTESIAN_POINT('',(0.,0.,-0.0202401835720864));
#33561=CARTESIAN_POINT('',(0.,0.,-0.0224076685637936));
#33562=CARTESIAN_POINT('',(0.,0.,0.0238076302250854));
#33563=CARTESIAN_POINT('',(0.,0.00159300366304774,0.));
#33564=CARTESIAN_POINT('',(0.,0.00159300366304774,0.));
#33565=CARTESIAN_POINT('',(0.,0.00159300366304774,-0.001));
#33566=CARTESIAN_POINT('',(0.,0.000812378913247946,0.));
#33567=CARTESIAN_POINT('',(0.,0.000812378913247946,-0.000625));
#33568=CARTESIAN_POINT('',(-0.0033118988125,0.0113437500020484,0.));
#33569=CARTESIAN_POINT('',(-0.0033118988125,0.0112500000020484,-0.00137183340534485));
#33570=CARTESIAN_POINT('',(-0.00234186610892243,0.0111562500020484,-0.00234186610892243));
#33571=CARTESIAN_POINT('',(-0.00137183340534485,0.0110625000020484,-0.0033118988125));
#33572=CARTESIAN_POINT('',(-2.02795313991402E-19,0.0109687500020484,-0.0033118988125));
#33573=CARTESIAN_POINT('',(0.00137183340534485,0.0108750000020484,-0.0033118988125));
#33574=CARTESIAN_POINT('',(0.00234186610892243,0.0107812500020484,-0.00234186610892243));
#33575=CARTESIAN_POINT('',(0.0033118988125,0.0106875000020484,-0.00137183340534485));
#33576=CARTESIAN_POINT('',(0.0033118988125,0.0105937500020484,-4.05590627982804E-19));
#33577=CARTESIAN_POINT('',(0.0033118988125,0.0105000000020484,0.00137183340534485));
#33578=CARTESIAN_POINT('',(0.00234186610892243,0.0104062500020484,0.00234186610892243));
#33579=CARTESIAN_POINT('',(0.00137183340534485,0.0103125000020484,0.0033118988125));
#33580=CARTESIAN_POINT('',(6.08385941974207E-19,0.0102187500020484,0.0033118988125));
#33581=CARTESIAN_POINT('',(-0.00137183340534485,0.0101250000020484,0.0033118988125));
#33582=CARTESIAN_POINT('',(-0.00234186610892243,0.0100312500020484,0.00234186610892243));
#33583=CARTESIAN_POINT('',(-0.0033118988125,0.00993750000204839,0.00137183340534485));
#33584=CARTESIAN_POINT('',(-0.0033118988125,0.00984375000204839,0.));
#33585=CARTESIAN_POINT('',(-0.0033118988125,0.00975000000204839,-0.00137183340534485));
#33586=CARTESIAN_POINT('',(-0.00234186610892243,0.00965625000204839,-0.00234186610892243));
#33587=CARTESIAN_POINT('',(-0.00137183340534485,0.00956250000204839,-0.0033118988125));
#33588=CARTESIAN_POINT('',(-2.02795313991402E-19,0.00946875000204839,-0.0033118988125));
#33589=CARTESIAN_POINT('',(0.00137183340534485,0.00937500000204839,-0.0033118988125));
#33590=CARTESIAN_POINT('',(0.00234186610892243,0.00928125000204839,-0.00234186610892243));
#33591=CARTESIAN_POINT('',(0.0033118988125,0.00918750000204839,-0.00137183340534485));
#33592=CARTESIAN_POINT('',(0.0033118988125,0.00909375000204839,-4.05590627982804E-19));
#33593=CARTESIAN_POINT('',(0.0033118988125,0.00900000000204839,0.00137183340534485));
#33594=CARTESIAN_POINT('',(0.00234186610892243,0.00890625000204839,0.00234186610892243));
#33595=CARTESIAN_POINT('',(0.00137183340534485,0.00881250000204839,0.0033118988125));
#33596=CARTESIAN_POINT('',(6.08385941974207E-19,0.00871875000204839,0.0033118988125));
#33597=CARTESIAN_POINT('',(-0.00137183340534485,0.00862500000204838,0.0033118988125));
#33598=CARTESIAN_POINT('',(-0.00234186610892243,0.00853125000204839,0.00234186610892243));
#33599=CARTESIAN_POINT('',(-0.0033118988125,0.00843750000204839,0.00137183340534485));
#33600=CARTESIAN_POINT('',(-0.0033118988125,0.00834375000204839,0.));
#33601=CARTESIAN_POINT('',(-0.0033118988125,0.00825000000204839,-0.00137183340534485));
#33602=CARTESIAN_POINT('',(-0.00234186610892243,0.00815625000204839,-0.00234186610892243));
#33603=CARTESIAN_POINT('',(-0.00137183340534485,0.00806250000204838,-0.0033118988125));
#33604=CARTESIAN_POINT('',(-2.02795313991402E-19,0.00796875000204839,-0.0033118988125));
#33605=CARTESIAN_POINT('',(0.00137183340534485,0.00787500000204839,-0.0033118988125));
#33606=CARTESIAN_POINT('',(0.00234186610892243,0.00778125000204839,-0.00234186610892243));
#33607=CARTESIAN_POINT('',(0.0033118988125,0.00768750000204838,-0.00137183340534485));
#33608=CARTESIAN_POINT('',(0.0033118988125,0.00759375000204839,-4.05590627982804E-19));
#33609=CARTESIAN_POINT('',(0.0033118988125,0.00750000000204839,0.00137183340534485));
#33610=CARTESIAN_POINT('',(0.00234186610892243,0.00740625000204839,0.00234186610892243));
#33611=CARTESIAN_POINT('',(0.00137183340534485,0.00731250000204839,0.0033118988125));
#33612=CARTESIAN_POINT('',(6.08385941974207E-19,0.00721875000204839,0.0033118988125));
#33613=CARTESIAN_POINT('',(-0.00137183340534485,0.00712500000204838,0.0033118988125));
#33614=CARTESIAN_POINT('',(-0.00234186610892243,0.00703125000204839,0.00234186610892243));
#33615=CARTESIAN_POINT('',(-0.0033118988125,0.00693750000204839,0.00137183340534485));
#33616=CARTESIAN_POINT('',(-0.0033118988125,0.00684375000204839,0.));
#33617=CARTESIAN_POINT('',(-0.0033118988125,0.00675000000204839,-0.00137183340534485));
#33618=CARTESIAN_POINT('',(-0.00234186610892243,0.00665625000204839,-0.00234186610892243));
#33619=CARTESIAN_POINT('',(-0.00137183340534485,0.00656250000204838,-0.0033118988125));
#33620=CARTESIAN_POINT('',(-2.02795313991402E-19,0.00646875000204839,-0.0033118988125));
#33621=CARTESIAN_POINT('',(0.00137183340534485,0.00637500000204839,-0.0033118988125));
#33622=CARTESIAN_POINT('',(0.00234186610892243,0.00628125000204839,-0.00234186610892243));
#33623=CARTESIAN_POINT('',(0.0033118988125,0.00618750000204839,-0.00137183340534485));
#33624=CARTESIAN_POINT('',(0.0033118988125,0.00609375000204839,-4.05590627982804E-19));
#33625=CARTESIAN_POINT('',(-0.0025,0.0108750000040968,0.));
#33626=CARTESIAN_POINT('',(-0.0025,0.0107812500040968,-0.00103553390593274));
#33627=CARTESIAN_POINT('',(-0.00176776695296637,0.0106875000040968,-0.00176776695296637));
#33628=CARTESIAN_POINT('',(-0.00103553390593274,0.0105937500040968,-0.0025));
#33629=CARTESIAN_POINT('',(-1.53080849893419E-19,0.0105000000040968,-0.0025));
#33630=CARTESIAN_POINT('',(0.00103553390593274,0.0104062500040968,-0.0025));
#33631=CARTESIAN_POINT('',(0.00176776695296637,0.0103125000040968,-0.00176776695296637));
#33632=CARTESIAN_POINT('',(0.0025,0.0102187500040968,-0.00103553390593274));
#33633=CARTESIAN_POINT('',(0.0025,0.0101250000040968,-3.06161699786838E-19));
#33634=CARTESIAN_POINT('',(0.0025,0.0100312500040968,0.00103553390593274));
#33635=CARTESIAN_POINT('',(0.00176776695296637,0.00993750000409678,0.00176776695296637));
#33636=CARTESIAN_POINT('',(0.00103553390593274,0.00984375000409678,0.0025));
#33637=CARTESIAN_POINT('',(4.59242549680257E-19,0.00975000000409678,0.0025));
#33638=CARTESIAN_POINT('',(-0.00103553390593274,0.00965625000409677,0.0025));
#33639=CARTESIAN_POINT('',(-0.00176776695296637,0.00956250000409678,0.00176776695296637));
#33640=CARTESIAN_POINT('',(-0.0025,0.00946875000409678,0.00103553390593274));
#33641=CARTESIAN_POINT('',(-0.0025,0.00937500000409678,0.));
#33642=CARTESIAN_POINT('',(-0.0025,0.00928125000409678,-0.00103553390593274));
#33643=CARTESIAN_POINT('',(-0.00176776695296637,0.00918750000409678,-0.00176776695296637));
#33644=CARTESIAN_POINT('',(-0.00103553390593274,0.00909375000409678,-0.0025));
#33645=CARTESIAN_POINT('',(-1.53080849893419E-19,0.00900000000409678,-0.0025));
#33646=CARTESIAN_POINT('',(0.00103553390593274,0.00890625000409678,-0.0025));
#33647=CARTESIAN_POINT('',(0.00176776695296637,0.00881250000409678,-0.00176776695296637));
#33648=CARTESIAN_POINT('',(0.0025,0.00871875000409679,-0.00103553390593274));
#33649=CARTESIAN_POINT('',(0.0025,0.00862500000409678,-3.06161699786838E-19));
#33650=CARTESIAN_POINT('',(0.0025,0.00853125000409678,0.00103553390593274));
#33651=CARTESIAN_POINT('',(0.00176776695296637,0.00843750000409678,0.00176776695296637));
#33652=CARTESIAN_POINT('',(0.00103553390593274,0.00834375000409678,0.0025));
#33653=CARTESIAN_POINT('',(4.59242549680257E-19,0.00825000000409678,0.0025));
#33654=CARTESIAN_POINT('',(-0.00103553390593274,0.00815625000409678,0.0025));
#33655=CARTESIAN_POINT('',(-0.00176776695296637,0.00806250000409678,0.00176776695296637));
#33656=CARTESIAN_POINT('',(-0.0025,0.00796875000409678,0.00103553390593274));
#33657=CARTESIAN_POINT('',(-0.0025,0.00787500000409678,0.));
#33658=CARTESIAN_POINT('',(-0.0025,0.00778125000409678,-0.00103553390593274));
#33659=CARTESIAN_POINT('',(-0.00176776695296637,0.00768750000409678,-0.00176776695296637));
#33660=CARTESIAN_POINT('',(-0.00103553390593274,0.00759375000409678,-0.0025));
#33661=CARTESIAN_POINT('',(-1.53080849893419E-19,0.00750000000409678,-0.0025));
#33662=CARTESIAN_POINT('',(0.00103553390593274,0.00740625000409678,-0.0025));
#33663=CARTESIAN_POINT('',(0.00176776695296637,0.00731250000409678,-0.00176776695296637));
#33664=CARTESIAN_POINT('',(0.0025,0.00721875000409678,-0.00103553390593274));
#33665=CARTESIAN_POINT('',(0.0025,0.00712500000409678,-3.06161699786838E-19));
#33666=CARTESIAN_POINT('',(0.0025,0.00703125000409678,0.00103553390593274));
#33667=CARTESIAN_POINT('',(0.00176776695296637,0.00693750000409678,0.00176776695296637));
#33668=CARTESIAN_POINT('',(0.00103553390593274,0.00684375000409678,0.0025));
#33669=CARTESIAN_POINT('',(4.59242549680257E-19,0.00675000000409678,0.0025));
#33670=CARTESIAN_POINT('',(-0.00103553390593274,0.00665625000409677,0.0025));
#33671=CARTESIAN_POINT('',(-0.00176776695296637,0.00656250000409678,0.00176776695296637));
#33672=CARTESIAN_POINT('',(-0.0025,0.00646875000409678,0.00103553390593274));
#33673=CARTESIAN_POINT('',(-0.0025,0.00637500000409678,0.));
#33674=CARTESIAN_POINT('',(-0.0025,0.00628125000409678,-0.00103553390593274));
#33675=CARTESIAN_POINT('',(-0.00176776695296637,0.00618750000409678,-0.00176776695296637));
#33676=CARTESIAN_POINT('',(-0.00103553390593274,0.00609375000409678,-0.0025));
#33677=CARTESIAN_POINT('',(-1.53080849893419E-19,0.00600000000409678,-0.0025));
#33678=CARTESIAN_POINT('',(0.00103553390593274,0.00590625000409678,-0.0025));
#33679=CARTESIAN_POINT('',(0.00176776695296637,0.00581250000409678,-0.00176776695296637));
#33680=CARTESIAN_POINT('',(0.0025,0.00571875000409678,-0.00103553390593274));
#33681=CARTESIAN_POINT('',(0.0025,0.00562500000409678,-3.06161699786838E-19));
#33682=CARTESIAN_POINT('',(4.52517978168079E-11,0.006,-0.0025));
#33683=CARTESIAN_POINT('',(0.000745353373849253,0.006,-0.00261687718084826));
#33684=CARTESIAN_POINT('',(0.0022915751006763,0.00599999999999974,-0.00215635246836324));
#33685=CARTESIAN_POINT('',(0.00305646177817112,0.006,-0.000747630389407334));
#33686=CARTESIAN_POINT('',(0.00314951904574251,0.006,-3.85704841822218E-19));
#33687=CARTESIAN_POINT('',(4.52517979936896E-11,0.006,-0.0025));
#33688=CARTESIAN_POINT('',(0.00314951904574251,0.006,-3.85704841822218E-19));
#33689=CARTESIAN_POINT('',(4.59242549680257E-19,0.00675000000409678,0.0025));
#33690=CARTESIAN_POINT('',(-0.00103553390593274,0.00665625000409677,0.0025));
#33691=CARTESIAN_POINT('',(-0.00176776695296637,0.00656250000409678,0.00176776695296637));
#33692=CARTESIAN_POINT('',(-0.0025,0.00646875000409678,0.00103553390593274));
#33693=CARTESIAN_POINT('',(-0.0025,0.00637500000409678,0.));
#33694=CARTESIAN_POINT('',(-0.0025,0.00628125000409678,-0.00103553390593274));
#33695=CARTESIAN_POINT('',(-0.00176776695296637,0.00618750000409678,-0.00176776695296637));
#33696=CARTESIAN_POINT('',(-0.00103553390593274,0.00609375000409678,-0.0025));
#33697=CARTESIAN_POINT('',(4.52517978168079E-11,0.006,-0.0025));
#33698=CARTESIAN_POINT('',(4.59242549680257E-19,0.00675000000409678,0.0025));
#33699=CARTESIAN_POINT('',(-1.53080849893419E-19,0.00750000000409678,-0.0025));
#33700=CARTESIAN_POINT('',(0.00103553390593274,0.00740625000409678,-0.0025));
#33701=CARTESIAN_POINT('',(0.00176776695296637,0.00731250000409678,-0.00176776695296637));
#33702=CARTESIAN_POINT('',(0.0025,0.00721875000409678,-0.00103553390593274));
#33703=CARTESIAN_POINT('',(0.0025,0.00712500000409678,-3.06161699786838E-19));
#33704=CARTESIAN_POINT('',(0.0025,0.00703125000409678,0.00103553390593274));
#33705=CARTESIAN_POINT('',(0.00176776695296637,0.00693750000409678,0.00176776695296637));
#33706=CARTESIAN_POINT('',(0.00103553390593274,0.00684375000409678,0.0025));
#33707=CARTESIAN_POINT('',(4.59242549680257E-19,0.00675000000409678,0.0025));
#33708=CARTESIAN_POINT('',(-1.53080849893419E-19,0.00750000000409678,-0.0025));
#33709=CARTESIAN_POINT('',(4.59242549680257E-19,0.00825000000409678,0.0025));
#33710=CARTESIAN_POINT('',(-0.00103553390593274,0.00815625000409678,0.0025));
#33711=CARTESIAN_POINT('',(-0.00176776695296637,0.00806250000409678,0.00176776695296637));
#33712=CARTESIAN_POINT('',(-0.0025,0.00796875000409678,0.00103553390593274));
#33713=CARTESIAN_POINT('',(-0.0025,0.00787500000409678,0.));
#33714=CARTESIAN_POINT('',(-0.0025,0.00778125000409678,-0.00103553390593274));
#33715=CARTESIAN_POINT('',(-0.00176776695296637,0.00768750000409678,-0.00176776695296637));
#33716=CARTESIAN_POINT('',(-0.00103553390593274,0.00759375000409678,-0.0025));
#33717=CARTESIAN_POINT('',(-1.53080849893419E-19,0.00750000000409678,-0.0025));
#33718=CARTESIAN_POINT('',(4.59242549680257E-19,0.00825000000409678,0.0025));
#33719=CARTESIAN_POINT('',(-1.53080849893419E-19,0.00900000000409678,-0.0025));
#33720=CARTESIAN_POINT('',(0.00103553390593274,0.00890625000409678,-0.0025));
#33721=CARTESIAN_POINT('',(0.00176776695296637,0.00881250000409678,-0.00176776695296637));
#33722=CARTESIAN_POINT('',(0.0025,0.00871875000409679,-0.00103553390593274));
#33723=CARTESIAN_POINT('',(0.0025,0.00862500000409678,-3.06161699786838E-19));
#33724=CARTESIAN_POINT('',(0.0025,0.00853125000409678,0.00103553390593274));
#33725=CARTESIAN_POINT('',(0.00176776695296637,0.00843750000409678,0.00176776695296637));
#33726=CARTESIAN_POINT('',(0.00103553390593274,0.00834375000409678,0.0025));
#33727=CARTESIAN_POINT('',(4.59242549680257E-19,0.00825000000409678,0.0025));
#33728=CARTESIAN_POINT('',(-1.53080849893419E-19,0.00900000000409678,-0.0025));
#33729=CARTESIAN_POINT('',(4.59242549680257E-19,0.00975000000409678,0.0025));
#33730=CARTESIAN_POINT('',(-0.00103553390593274,0.00965625000409677,0.0025));
#33731=CARTESIAN_POINT('',(-0.00176776695296637,0.00956250000409678,0.00176776695296637));
#33732=CARTESIAN_POINT('',(-0.0025,0.00946875000409678,0.00103553390593274));
#33733=CARTESIAN_POINT('',(-0.0025,0.00937500000409678,0.));
#33734=CARTESIAN_POINT('',(-0.0025,0.00928125000409678,-0.00103553390593274));
#33735=CARTESIAN_POINT('',(-0.00176776695296637,0.00918750000409678,-0.00176776695296637));
#33736=CARTESIAN_POINT('',(-0.00103553390593274,0.00909375000409678,-0.0025));
#33737=CARTESIAN_POINT('',(-1.53080849893419E-19,0.00900000000409678,-0.0025));
#33738=CARTESIAN_POINT('',(4.59242549680257E-19,0.00975000000409678,0.0025));
#33739=CARTESIAN_POINT('',(-1.53080849893419E-19,0.0105000000040968,-0.0025));
#33740=CARTESIAN_POINT('',(0.00103553390593274,0.0104062500040968,-0.0025));
#33741=CARTESIAN_POINT('',(0.00176776695296637,0.0103125000040968,-0.00176776695296637));
#33742=CARTESIAN_POINT('',(0.0025,0.0102187500040968,-0.00103553390593274));
#33743=CARTESIAN_POINT('',(0.0025,0.0101250000040968,-3.06161699786838E-19));
#33744=CARTESIAN_POINT('',(0.0025,0.0100312500040968,0.00103553390593274));
#33745=CARTESIAN_POINT('',(0.00176776695296637,0.00993750000409678,0.00176776695296637));
#33746=CARTESIAN_POINT('',(0.00103553390593274,0.00984375000409678,0.0025));
#33747=CARTESIAN_POINT('',(4.59242549680257E-19,0.00975000000409678,0.0025));
#33748=CARTESIAN_POINT('',(-1.53080849893419E-19,0.0105000000040968,-0.0025));
#33749=CARTESIAN_POINT('',(-0.0025,0.0108750000040968,0.));
#33750=CARTESIAN_POINT('',(-0.0025,0.0107812500040968,-0.00103553390593274));
#33751=CARTESIAN_POINT('',(-0.00176776695296637,0.0106875000040968,-0.00176776695296637));
#33752=CARTESIAN_POINT('',(-0.00103553390593274,0.0105937500040968,-0.0025));
#33753=CARTESIAN_POINT('',(-1.53080849893419E-19,0.0105000000040968,-0.0025));
#33754=CARTESIAN_POINT('',(-0.0025,0.0108750000040968,0.));
#33755=CARTESIAN_POINT('',(-0.00290594940625,0.0111093750030726,0.));
#33756=CARTESIAN_POINT('',(-0.0033118988125,0.0113437500020484,0.));
#33757=CARTESIAN_POINT('',(-0.0033118988125,0.0113437500020484,0.));
#33758=CARTESIAN_POINT('',(-0.0033118988125,0.0112500000020484,-0.00137183340534485));
#33759=CARTESIAN_POINT('',(-0.00234186610892243,0.0111562500020484,-0.00234186610892243));
#33760=CARTESIAN_POINT('',(-0.00137183340534485,0.0110625000020484,-0.0033118988125));
#33761=CARTESIAN_POINT('',(-2.02795313991402E-19,0.0109687500020484,-0.0033118988125));
#33762=CARTESIAN_POINT('',(0.00137183340534485,0.0108750000020484,-0.0033118988125));
#33763=CARTESIAN_POINT('',(0.00234186610892243,0.0107812500020484,-0.00234186610892243));
#33764=CARTESIAN_POINT('',(0.0033118988125,0.0106875000020484,-0.00137183340534485));
#33765=CARTESIAN_POINT('',(0.0033118988125,0.0105937500020484,-4.05590627982804E-19));
#33766=CARTESIAN_POINT('',(0.0033118988125,0.0105000000020484,0.00137183340534485));
#33767=CARTESIAN_POINT('',(0.00234186610892243,0.0104062500020484,0.00234186610892243));
#33768=CARTESIAN_POINT('',(0.00137183340534485,0.0103125000020484,0.0033118988125));
#33769=CARTESIAN_POINT('',(6.08385941974207E-19,0.0102187500020484,0.0033118988125));
#33770=CARTESIAN_POINT('',(-0.00137183340534485,0.0101250000020484,0.0033118988125));
#33771=CARTESIAN_POINT('',(-0.00234186610892243,0.0100312500020484,0.00234186610892243));
#33772=CARTESIAN_POINT('',(-0.0033118988125,0.00993750000204839,0.00137183340534485));
#33773=CARTESIAN_POINT('',(-0.0033118988125,0.00984375000204839,0.));
#33774=CARTESIAN_POINT('',(-0.0033118988125,0.00975000000204839,-0.00137183340534485));
#33775=CARTESIAN_POINT('',(-0.00234186610892243,0.00965625000204839,-0.00234186610892243));
#33776=CARTESIAN_POINT('',(-0.00137183340534485,0.00956250000204839,-0.0033118988125));
#33777=CARTESIAN_POINT('',(-2.02795313991402E-19,0.00946875000204839,-0.0033118988125));
#33778=CARTESIAN_POINT('',(0.00137183340534485,0.00937500000204839,-0.0033118988125));
#33779=CARTESIAN_POINT('',(0.00234186610892243,0.00928125000204839,-0.00234186610892243));
#33780=CARTESIAN_POINT('',(0.0033118988125,0.00918750000204839,-0.00137183340534485));
#33781=CARTESIAN_POINT('',(0.0033118988125,0.00909375000204839,-4.05590627982804E-19));
#33782=CARTESIAN_POINT('',(0.0033118988125,0.00900000000204839,0.00137183340534485));
#33783=CARTESIAN_POINT('',(0.00234186610892243,0.00890625000204839,0.00234186610892243));
#33784=CARTESIAN_POINT('',(0.00137183340534485,0.00881250000204839,0.0033118988125));
#33785=CARTESIAN_POINT('',(6.08385941974207E-19,0.00871875000204839,0.0033118988125));
#33786=CARTESIAN_POINT('',(-0.00137183340534485,0.00862500000204838,0.0033118988125));
#33787=CARTESIAN_POINT('',(-0.00234186610892243,0.00853125000204839,0.00234186610892243));
#33788=CARTESIAN_POINT('',(-0.0033118988125,0.00843750000204839,0.00137183340534485));
#33789=CARTESIAN_POINT('',(-0.0033118988125,0.00834375000204839,0.));
#33790=CARTESIAN_POINT('',(-0.0033118988125,0.00825000000204839,-0.00137183340534485));
#33791=CARTESIAN_POINT('',(-0.00234186610892243,0.00815625000204839,-0.00234186610892243));
#33792=CARTESIAN_POINT('',(-0.00137183340534485,0.00806250000204839,-0.0033118988125));
#33793=CARTESIAN_POINT('',(-2.02795313991402E-19,0.00796875000204839,-0.0033118988125));
#33794=CARTESIAN_POINT('',(0.00137183340534485,0.00787500000204839,-0.0033118988125));
#33795=CARTESIAN_POINT('',(0.00234186610892243,0.00778125000204839,-0.00234186610892243));
#33796=CARTESIAN_POINT('',(0.0033118988125,0.00768750000204838,-0.00137183340534485));
#33797=CARTESIAN_POINT('',(0.0033118988125,0.00759375000204839,-4.05590627982804E-19));
#33798=CARTESIAN_POINT('',(0.0033118988125,0.00750000000204839,0.00137183340534485));
#33799=CARTESIAN_POINT('',(0.00234186610892243,0.00740625000204839,0.00234186610892243));
#33800=CARTESIAN_POINT('',(0.00137183340534485,0.00731250000204839,0.0033118988125));
#33801=CARTESIAN_POINT('',(6.08385941974207E-19,0.00721875000204839,0.0033118988125));
#33802=CARTESIAN_POINT('',(-0.00137183340534485,0.00712500000204839,0.0033118988125));
#33803=CARTESIAN_POINT('',(-0.00234186610892243,0.00703125000204839,0.00234186610892243));
#33804=CARTESIAN_POINT('',(-0.0033118988125,0.00693750000204839,0.00137183340534485));
#33805=CARTESIAN_POINT('',(-0.0033118988125,0.00684375000204839,0.));
#33806=CARTESIAN_POINT('',(-0.0033118988125,0.00675000000204839,-0.00137183340534485));
#33807=CARTESIAN_POINT('',(-0.00234186610892243,0.00665625000204839,-0.00234186610892243));
#33808=CARTESIAN_POINT('',(-0.00137183340534485,0.00656250000204838,-0.0033118988125));
#33809=CARTESIAN_POINT('',(-2.02795313991402E-19,0.00646875000204839,-0.0033118988125));
#33810=CARTESIAN_POINT('',(0.00137183340534485,0.00637500000204839,-0.0033118988125));
#33811=CARTESIAN_POINT('',(0.00234186610892243,0.00628125000204839,-0.00234186610892243));
#33812=CARTESIAN_POINT('',(0.0033118988125,0.00618750000204839,-0.00137183340534485));
#33813=CARTESIAN_POINT('',(0.0033118988125,0.00609375000204839,-4.05590627982804E-19));
#33814=CARTESIAN_POINT('',(0.00331189864583333,0.00609375009827343,-4.05590607572024E-19));
#33815=CARTESIAN_POINT('',(0.00323070892912125,0.0060468750010242,-3.95647734902512E-19));
#33816=CARTESIAN_POINT('',(-0.0025,0.012,0.));
#33817=CARTESIAN_POINT('',(-0.0025,0.01190625,-0.00103553390593274));
#33818=CARTESIAN_POINT('',(-0.00176776695296637,0.0118125,-0.00176776695296637));
#33819=CARTESIAN_POINT('',(-0.00103553390593274,0.01171875,-0.0025));
#33820=CARTESIAN_POINT('',(-1.53080849893419E-19,0.011625,-0.0025));
#33821=CARTESIAN_POINT('',(0.00103553390593274,0.01153125,-0.0025));
#33822=CARTESIAN_POINT('',(0.00176776695296637,0.0114375,-0.00176776695296637));
#33823=CARTESIAN_POINT('',(0.0025,0.01134375,-0.00103553390593274));
#33824=CARTESIAN_POINT('',(0.0025,0.01125,-3.06161699786838E-19));
#33825=CARTESIAN_POINT('',(0.0025,0.01115625,0.00103553390593274));
#33826=CARTESIAN_POINT('',(0.00176776695296637,0.0110625,0.00176776695296637));
#33827=CARTESIAN_POINT('',(0.00103553390593274,0.01096875,0.0025));
#33828=CARTESIAN_POINT('',(4.59242549680257E-19,0.010875,0.0025));
#33829=CARTESIAN_POINT('',(-0.00103553390593274,0.01078125,0.0025));
#33830=CARTESIAN_POINT('',(-0.00176776695296637,0.0106875,0.00176776695296637));
#33831=CARTESIAN_POINT('',(-0.0025,0.01059375,0.00103553390593274));
#33832=CARTESIAN_POINT('',(-0.0025,0.0105,0.));
#33833=CARTESIAN_POINT('',(-0.0025,0.01040625,-0.00103553390593274));
#33834=CARTESIAN_POINT('',(-0.00176776695296637,0.0103125,-0.00176776695296637));
#33835=CARTESIAN_POINT('',(-0.00103553390593274,0.01021875,-0.0025));
#33836=CARTESIAN_POINT('',(-1.53080849893419E-19,0.010125,-0.0025));
#33837=CARTESIAN_POINT('',(0.00103553390593274,0.01003125,-0.0025));
#33838=CARTESIAN_POINT('',(0.00176776695296637,0.0099375,-0.00176776695296637));
#33839=CARTESIAN_POINT('',(0.0025,0.00984375,-0.00103553390593274));
#33840=CARTESIAN_POINT('',(0.0025,0.00975,-3.06161699786838E-19));
#33841=CARTESIAN_POINT('',(0.0025,0.00965624999999999,0.00103553390593274));
#33842=CARTESIAN_POINT('',(0.00176776695296637,0.0095625,0.00176776695296637));
#33843=CARTESIAN_POINT('',(0.00103553390593274,0.00946875,0.0025));
#33844=CARTESIAN_POINT('',(4.59242549680257E-19,0.009375,0.0025));
#33845=CARTESIAN_POINT('',(-0.00103553390593274,0.00928125,0.0025));
#33846=CARTESIAN_POINT('',(-0.00176776695296637,0.0091875,0.00176776695296637));
#33847=CARTESIAN_POINT('',(-0.0025,0.00909374999999999,0.00103553390593274));
#33848=CARTESIAN_POINT('',(-0.0025,0.009,0.));
#33849=CARTESIAN_POINT('',(-0.0025,0.00890625,-0.00103553390593274));
#33850=CARTESIAN_POINT('',(-0.00176776695296637,0.0088125,-0.00176776695296637));
#33851=CARTESIAN_POINT('',(-0.00103553390593274,0.00871875,-0.0025));
#33852=CARTESIAN_POINT('',(-1.53080849893419E-19,0.008625,-0.0025));
#33853=CARTESIAN_POINT('',(0.00103553390593274,0.00853125,-0.0025));
#33854=CARTESIAN_POINT('',(0.00176776695296637,0.0084375,-0.00176776695296637));
#33855=CARTESIAN_POINT('',(0.0025,0.00834375,-0.00103553390593274));
#33856=CARTESIAN_POINT('',(0.0025,0.00825,-3.06161699786838E-19));
#33857=CARTESIAN_POINT('',(0.0025,0.00815625,0.00103553390593274));
#33858=CARTESIAN_POINT('',(0.00176776695296637,0.0080625,0.00176776695296637));
#33859=CARTESIAN_POINT('',(0.00103553390593274,0.00796875,0.0025));
#33860=CARTESIAN_POINT('',(4.59242549680257E-19,0.007875,0.0025));
#33861=CARTESIAN_POINT('',(-0.00103553390593274,0.00778125,0.0025));
#33862=CARTESIAN_POINT('',(-0.00176776695296637,0.0076875,0.00176776695296637));
#33863=CARTESIAN_POINT('',(-0.0025,0.00759374999999999,0.00103553390593274));
#33864=CARTESIAN_POINT('',(-0.0025,0.0075,0.));
#33865=CARTESIAN_POINT('',(-0.0025,0.00740625,-0.00103553390593274));
#33866=CARTESIAN_POINT('',(-0.00176776695296637,0.0073125,-0.00176776695296637));
#33867=CARTESIAN_POINT('',(-0.00103553390593274,0.00721875,-0.0025));
#33868=CARTESIAN_POINT('',(-1.53080849893419E-19,0.007125,-0.0025));
#33869=CARTESIAN_POINT('',(0.00103553390593274,0.00703124999999999,-0.0025));
#33870=CARTESIAN_POINT('',(0.00176776695296637,0.0069375,-0.00176776695296637));
#33871=CARTESIAN_POINT('',(0.0025,0.00684375,-0.00103553390593274));
#33872=CARTESIAN_POINT('',(0.0025,0.00675,-3.06161699786838E-19));
#33873=CARTESIAN_POINT('',(-0.0033118988125,0.0115312500020484,0.));
#33874=CARTESIAN_POINT('',(-0.0033118988125,0.0114375000020484,-0.00137183340534485));
#33875=CARTESIAN_POINT('',(-0.00234186610892243,0.0113437500020484,-0.00234186610892243));
#33876=CARTESIAN_POINT('',(-0.00137183340534485,0.0112500000020484,-0.0033118988125));
#33877=CARTESIAN_POINT('',(-2.02795313991402E-19,0.0111562500020484,-0.0033118988125));
#33878=CARTESIAN_POINT('',(0.00137183340534485,0.0110625000020484,-0.0033118988125));
#33879=CARTESIAN_POINT('',(0.00234186610892243,0.0109687500020484,-0.00234186610892243));
#33880=CARTESIAN_POINT('',(0.0033118988125,0.0108750000020484,-0.00137183340534485));
#33881=CARTESIAN_POINT('',(0.0033118988125,0.0107812500020484,-4.05590627982804E-19));
#33882=CARTESIAN_POINT('',(0.0033118988125,0.0106875000020484,0.00137183340534485));
#33883=CARTESIAN_POINT('',(0.00234186610892243,0.0105937500020484,0.00234186610892243));
#33884=CARTESIAN_POINT('',(0.00137183340534485,0.0105000000020484,0.0033118988125));
#33885=CARTESIAN_POINT('',(6.08385941974207E-19,0.0104062500020484,0.0033118988125));
#33886=CARTESIAN_POINT('',(-0.00137183340534485,0.0103125000020484,0.0033118988125));
#33887=CARTESIAN_POINT('',(-0.00234186610892243,0.0102187500020484,0.00234186610892243));
#33888=CARTESIAN_POINT('',(-0.0033118988125,0.0101250000020484,0.00137183340534485));
#33889=CARTESIAN_POINT('',(-0.0033118988125,0.0100312500020484,0.));
#33890=CARTESIAN_POINT('',(-0.0033118988125,0.00993750000204839,-0.00137183340534485));
#33891=CARTESIAN_POINT('',(-0.00234186610892243,0.00984375000204839,-0.00234186610892243));
#33892=CARTESIAN_POINT('',(-0.00137183340534485,0.00975000000204839,-0.0033118988125));
#33893=CARTESIAN_POINT('',(-2.02795313991402E-19,0.00965625000204839,-0.0033118988125));
#33894=CARTESIAN_POINT('',(0.00137183340534485,0.00956250000204839,-0.0033118988125));
#33895=CARTESIAN_POINT('',(0.00234186610892243,0.00946875000204839,-0.00234186610892243));
#33896=CARTESIAN_POINT('',(0.0033118988125,0.00937500000204839,-0.00137183340534485));
#33897=CARTESIAN_POINT('',(0.0033118988125,0.00928125000204839,-4.05590627982804E-19));
#33898=CARTESIAN_POINT('',(0.0033118988125,0.00918750000204839,0.00137183340534485));
#33899=CARTESIAN_POINT('',(0.00234186610892243,0.00909375000204839,0.00234186610892243));
#33900=CARTESIAN_POINT('',(0.00137183340534485,0.00900000000204839,0.0033118988125));
#33901=CARTESIAN_POINT('',(6.08385941974207E-19,0.00890625000204839,0.0033118988125));
#33902=CARTESIAN_POINT('',(-0.00137183340534485,0.00881250000204839,0.0033118988125));
#33903=CARTESIAN_POINT('',(-0.00234186610892243,0.00871875000204839,0.00234186610892243));
#33904=CARTESIAN_POINT('',(-0.0033118988125,0.00862500000204838,0.00137183340534485));
#33905=CARTESIAN_POINT('',(-0.0033118988125,0.00853125000204839,0.));
#33906=CARTESIAN_POINT('',(-0.0033118988125,0.00843750000204839,-0.00137183340534485));
#33907=CARTESIAN_POINT('',(-0.00234186610892243,0.00834375000204839,-0.00234186610892243));
#33908=CARTESIAN_POINT('',(-0.00137183340534485,0.00825000000204839,-0.0033118988125));
#33909=CARTESIAN_POINT('',(-2.02795313991402E-19,0.00815625000204839,-0.0033118988125));
#33910=CARTESIAN_POINT('',(0.00137183340534485,0.00806250000204838,-0.0033118988125));
#33911=CARTESIAN_POINT('',(0.00234186610892243,0.00796875000204839,-0.00234186610892243));
#33912=CARTESIAN_POINT('',(0.0033118988125,0.00787500000204839,-0.00137183340534485));
#33913=CARTESIAN_POINT('',(0.0033118988125,0.00778125000204839,-4.05590627982804E-19));
#33914=CARTESIAN_POINT('',(0.0033118988125,0.00768750000204838,0.00137183340534485));
#33915=CARTESIAN_POINT('',(0.00234186610892243,0.00759375000204839,0.00234186610892243));
#33916=CARTESIAN_POINT('',(0.00137183340534485,0.00750000000204839,0.0033118988125));
#33917=CARTESIAN_POINT('',(6.08385941974207E-19,0.00740625000204839,0.0033118988125));
#33918=CARTESIAN_POINT('',(-0.00137183340534485,0.00731250000204839,0.0033118988125));
#33919=CARTESIAN_POINT('',(-0.00234186610892243,0.00721875000204839,0.00234186610892243));
#33920=CARTESIAN_POINT('',(-0.0033118988125,0.00712500000204838,0.00137183340534485));
#33921=CARTESIAN_POINT('',(-0.0033118988125,0.00703125000204839,0.));
#33922=CARTESIAN_POINT('',(-0.0033118988125,0.00693750000204839,-0.00137183340534485));
#33923=CARTESIAN_POINT('',(-0.00234186610892243,0.00684375000204839,-0.00234186610892243));
#33924=CARTESIAN_POINT('',(-0.00137183340534485,0.00675000000204839,-0.0033118988125));
#33925=CARTESIAN_POINT('',(-2.02795313991402E-19,0.00665625000204839,-0.0033118988125));
#33926=CARTESIAN_POINT('',(0.00137183340534485,0.00656250000204838,-0.0033118988125));
#33927=CARTESIAN_POINT('',(0.00234186610892243,0.00646875000204839,-0.00234186610892243));
#33928=CARTESIAN_POINT('',(0.0033118988125,0.00637500000204839,-0.00137183340534485));
#33929=CARTESIAN_POINT('',(0.0033118988125,0.00628125000204839,-4.05590627982804E-19));
#33930=CARTESIAN_POINT('',(-0.00290594940625,0.0117656250010242,0.));
#33931=CARTESIAN_POINT('',(-0.0025,0.012,0.));
#33932=CARTESIAN_POINT('',(-0.0033118988125,0.0115312500020484,0.));
#33933=CARTESIAN_POINT('',(-0.0025,0.012,0.));
#33934=CARTESIAN_POINT('',(-0.0025,0.01190625,-0.00103553390593274));
#33935=CARTESIAN_POINT('',(-0.00176776695296637,0.0118125,-0.00176776695296637));
#33936=CARTESIAN_POINT('',(-0.00103553390593274,0.01171875,-0.0025));
#33937=CARTESIAN_POINT('',(-1.53080849893419E-19,0.011625,-0.0025));
#33938=CARTESIAN_POINT('',(-1.53080849893419E-19,0.011625,-0.0025));
#33939=CARTESIAN_POINT('',(-1.53080849893419E-19,0.011625,-0.0025));
#33940=CARTESIAN_POINT('',(0.00103553390593274,0.01153125,-0.0025));
#33941=CARTESIAN_POINT('',(0.00176776695296637,0.0114375,-0.00176776695296637));
#33942=CARTESIAN_POINT('',(0.0025,0.01134375,-0.00103553390593274));
#33943=CARTESIAN_POINT('',(0.0025,0.01125,-3.06161699786838E-19));
#33944=CARTESIAN_POINT('',(0.0025,0.01115625,0.00103553390593274));
#33945=CARTESIAN_POINT('',(0.00176776695296637,0.0110625,0.00176776695296637));
#33946=CARTESIAN_POINT('',(0.00103553390593274,0.01096875,0.0025));
#33947=CARTESIAN_POINT('',(4.59242549680257E-19,0.010875,0.0025));
#33948=CARTESIAN_POINT('',(4.59242549680257E-19,0.010875,0.0025));
#33949=CARTESIAN_POINT('',(4.59242549680257E-19,0.010875,0.0025));
#33950=CARTESIAN_POINT('',(-0.00103553390593274,0.01078125,0.0025));
#33951=CARTESIAN_POINT('',(-0.00176776695296637,0.0106875,0.00176776695296637));
#33952=CARTESIAN_POINT('',(-0.0025,0.01059375,0.00103553390593274));
#33953=CARTESIAN_POINT('',(-0.0025,0.0105,0.));
#33954=CARTESIAN_POINT('',(-0.0025,0.01040625,-0.00103553390593274));
#33955=CARTESIAN_POINT('',(-0.00176776695296637,0.0103125,-0.00176776695296637));
#33956=CARTESIAN_POINT('',(-0.00103553390593274,0.01021875,-0.0025));
#33957=CARTESIAN_POINT('',(-1.53080849893419E-19,0.010125,-0.0025));
#33958=CARTESIAN_POINT('',(-1.53080849893419E-19,0.010125,-0.0025));
#33959=CARTESIAN_POINT('',(-1.53080849893419E-19,0.010125,-0.0025));
#33960=CARTESIAN_POINT('',(0.00103553390593274,0.01003125,-0.0025));
#33961=CARTESIAN_POINT('',(0.00176776695296637,0.0099375,-0.00176776695296637));
#33962=CARTESIAN_POINT('',(0.0025,0.00984375,-0.00103553390593274));
#33963=CARTESIAN_POINT('',(0.0025,0.00975,-3.06161699786838E-19));
#33964=CARTESIAN_POINT('',(0.0025,0.00965624999999999,0.00103553390593274));
#33965=CARTESIAN_POINT('',(0.00176776695296637,0.0095625,0.00176776695296637));
#33966=CARTESIAN_POINT('',(0.00103553390593274,0.00946875,0.0025));
#33967=CARTESIAN_POINT('',(4.59242549680257E-19,0.009375,0.0025));
#33968=CARTESIAN_POINT('',(4.59242549680257E-19,0.009375,0.0025));
#33969=CARTESIAN_POINT('',(4.59242549680257E-19,0.009375,0.0025));
#33970=CARTESIAN_POINT('',(-0.00103553390593274,0.00928125,0.0025));
#33971=CARTESIAN_POINT('',(-0.00176776695296637,0.0091875,0.00176776695296637));
#33972=CARTESIAN_POINT('',(-0.0025,0.00909374999999999,0.00103553390593274));
#33973=CARTESIAN_POINT('',(-0.0025,0.009,0.));
#33974=CARTESIAN_POINT('',(-0.0025,0.00890625,-0.00103553390593274));
#33975=CARTESIAN_POINT('',(-0.00176776695296637,0.0088125,-0.00176776695296637));
#33976=CARTESIAN_POINT('',(-0.00103553390593274,0.00871875,-0.0025));
#33977=CARTESIAN_POINT('',(-1.53080849893419E-19,0.008625,-0.0025));
#33978=CARTESIAN_POINT('',(-1.53080849893419E-19,0.008625,-0.0025));
#33979=CARTESIAN_POINT('',(-1.53080849893419E-19,0.008625,-0.0025));
#33980=CARTESIAN_POINT('',(0.00103553390593274,0.00853125,-0.0025));
#33981=CARTESIAN_POINT('',(0.00176776695296637,0.0084375,-0.00176776695296637));
#33982=CARTESIAN_POINT('',(0.0025,0.00834375,-0.00103553390593274));
#33983=CARTESIAN_POINT('',(0.0025,0.00825,-3.06161699786838E-19));
#33984=CARTESIAN_POINT('',(0.0025,0.00815625,0.00103553390593274));
#33985=CARTESIAN_POINT('',(0.00176776695296637,0.0080625,0.00176776695296637));
#33986=CARTESIAN_POINT('',(0.00103553390593274,0.00796875,0.0025));
#33987=CARTESIAN_POINT('',(4.59242549680257E-19,0.007875,0.0025));
#33988=CARTESIAN_POINT('',(4.59242549680257E-19,0.007875,0.0025));
#33989=CARTESIAN_POINT('',(4.59242549680257E-19,0.007875,0.0025));
#33990=CARTESIAN_POINT('',(-0.00103553390593274,0.00778125,0.0025));
#33991=CARTESIAN_POINT('',(-0.00176776695296637,0.0076875,0.00176776695296637));
#33992=CARTESIAN_POINT('',(-0.0025,0.00759374999999999,0.00103553390593274));
#33993=CARTESIAN_POINT('',(-0.0025,0.0075,0.));
#33994=CARTESIAN_POINT('',(-0.0025,0.00740625,-0.00103553390593274));
#33995=CARTESIAN_POINT('',(-0.00176776695296637,0.0073125,-0.00176776695296637));
#33996=CARTESIAN_POINT('',(-0.00103553390593274,0.00721875,-0.0025));
#33997=CARTESIAN_POINT('',(-1.53080849893419E-19,0.007125,-0.0025));
#33998=CARTESIAN_POINT('',(-1.53080849893419E-19,0.007125,-0.0025));
#33999=CARTESIAN_POINT('',(-1.53080849893419E-19,0.007125,-0.0025));
#34000=CARTESIAN_POINT('',(0.00103553390593274,0.00703125,-0.0025));
#34001=CARTESIAN_POINT('',(0.00176776695296637,0.0069375,-0.00176776695296637));
#34002=CARTESIAN_POINT('',(0.0025,0.00684375,-0.00103553390593274));
#34003=CARTESIAN_POINT('',(0.0025,0.00675,-3.06161699786838E-19));
#34004=CARTESIAN_POINT('',(0.0025,0.00675,-3.06161699786838E-19));
#34005=CARTESIAN_POINT('',(0.00290594940625,0.00651562500102419,-3.55876163884822E-19));
#34006=CARTESIAN_POINT('',(0.00331189864583333,0.00628124990582335,-4.05590607572024E-19));
#34007=CARTESIAN_POINT('',(-0.0033118988125,0.0115312500020484,0.));
#34008=CARTESIAN_POINT('',(-0.0033118988125,0.0114375000020484,-0.00137183340534485));
#34009=CARTESIAN_POINT('',(-0.00234186610892243,0.0113437500020484,-0.00234186610892243));
#34010=CARTESIAN_POINT('',(-0.00137183340534485,0.0112500000020484,-0.0033118988125));
#34011=CARTESIAN_POINT('',(-2.02795313991402E-19,0.0111562500020484,-0.0033118988125));
#34012=CARTESIAN_POINT('',(0.00137183340534485,0.0110625000020484,-0.0033118988125));
#34013=CARTESIAN_POINT('',(0.00234186610892243,0.0109687500020484,-0.00234186610892243));
#34014=CARTESIAN_POINT('',(0.0033118988125,0.0108750000020484,-0.00137183340534485));
#34015=CARTESIAN_POINT('',(0.0033118988125,0.0107812500020484,-4.05590627982804E-19));
#34016=CARTESIAN_POINT('',(0.0033118988125,0.0106875000020484,0.00137183340534485));
#34017=CARTESIAN_POINT('',(0.00234186610892243,0.0105937500020484,0.00234186610892243));
#34018=CARTESIAN_POINT('',(0.00137183340534485,0.0105000000020484,0.0033118988125));
#34019=CARTESIAN_POINT('',(6.08385941974207E-19,0.0104062500020484,0.0033118988125));
#34020=CARTESIAN_POINT('',(-0.00137183340534485,0.0103125000020484,0.0033118988125));
#34021=CARTESIAN_POINT('',(-0.00234186610892243,0.0102187500020484,0.00234186610892243));
#34022=CARTESIAN_POINT('',(-0.0033118988125,0.0101250000020484,0.00137183340534485));
#34023=CARTESIAN_POINT('',(-0.0033118988125,0.0100312500020484,0.));
#34024=CARTESIAN_POINT('',(-0.0033118988125,0.00993750000204839,-0.00137183340534485));
#34025=CARTESIAN_POINT('',(-0.00234186610892243,0.00984375000204839,-0.00234186610892243));
#34026=CARTESIAN_POINT('',(-0.00137183340534485,0.00975000000204839,-0.0033118988125));
#34027=CARTESIAN_POINT('',(-2.02795313991402E-19,0.00965625000204839,-0.0033118988125));
#34028=CARTESIAN_POINT('',(0.00137183340534485,0.00956250000204839,-0.0033118988125));
#34029=CARTESIAN_POINT('',(0.00234186610892243,0.00946875000204839,-0.00234186610892243));
#34030=CARTESIAN_POINT('',(0.0033118988125,0.00937500000204839,-0.00137183340534485));
#34031=CARTESIAN_POINT('',(0.0033118988125,0.00928125000204839,-4.05590627982804E-19));
#34032=CARTESIAN_POINT('',(0.0033118988125,0.00918750000204839,0.00137183340534485));
#34033=CARTESIAN_POINT('',(0.00234186610892243,0.00909375000204839,0.00234186610892243));
#34034=CARTESIAN_POINT('',(0.00137183340534485,0.00900000000204839,0.0033118988125));
#34035=CARTESIAN_POINT('',(6.08385941974207E-19,0.00890625000204839,0.0033118988125));
#34036=CARTESIAN_POINT('',(-0.00137183340534485,0.00881250000204839,0.0033118988125));
#34037=CARTESIAN_POINT('',(-0.00234186610892243,0.00871875000204839,0.00234186610892243));
#34038=CARTESIAN_POINT('',(-0.0033118988125,0.00862500000204838,0.00137183340534485));
#34039=CARTESIAN_POINT('',(-0.0033118988125,0.00853125000204839,0.));
#34040=CARTESIAN_POINT('',(-0.0033118988125,0.00843750000204839,-0.00137183340534485));
#34041=CARTESIAN_POINT('',(-0.00234186610892243,0.00834375000204839,-0.00234186610892243));
#34042=CARTESIAN_POINT('',(-0.00137183340534485,0.00825000000204839,-0.0033118988125));
#34043=CARTESIAN_POINT('',(-2.02795313991402E-19,0.00815625000204839,-0.0033118988125));
#34044=CARTESIAN_POINT('',(0.00137183340534485,0.00806250000204839,-0.0033118988125));
#34045=CARTESIAN_POINT('',(0.00234186610892243,0.00796875000204839,-0.00234186610892243));
#34046=CARTESIAN_POINT('',(0.0033118988125,0.00787500000204839,-0.00137183340534485));
#34047=CARTESIAN_POINT('',(0.0033118988125,0.00778125000204839,-4.05590627982804E-19));
#34048=CARTESIAN_POINT('',(0.0033118988125,0.00768750000204838,0.00137183340534485));
#34049=CARTESIAN_POINT('',(0.00234186610892243,0.00759375000204839,0.00234186610892243));
#34050=CARTESIAN_POINT('',(0.00137183340534485,0.00750000000204839,0.0033118988125));
#34051=CARTESIAN_POINT('',(6.08385941974207E-19,0.00740625000204839,0.0033118988125));
#34052=CARTESIAN_POINT('',(-0.00137183340534485,0.00731250000204839,0.0033118988125));
#34053=CARTESIAN_POINT('',(-0.00234186610892243,0.00721875000204839,0.00234186610892243));
#34054=CARTESIAN_POINT('',(-0.0033118988125,0.00712500000204839,0.00137183340534485));
#34055=CARTESIAN_POINT('',(-0.0033118988125,0.00703125000204839,0.));
#34056=CARTESIAN_POINT('',(-0.0033118988125,0.00693750000204839,-0.00137183340534485));
#34057=CARTESIAN_POINT('',(-0.00234186610892243,0.00684375000204839,-0.00234186610892243));
#34058=CARTESIAN_POINT('',(-0.00137183340534485,0.00675000000204839,-0.0033118988125));
#34059=CARTESIAN_POINT('',(-2.02795313991402E-19,0.00665625000204839,-0.0033118988125));
#34060=CARTESIAN_POINT('',(0.00137183340534485,0.00656250000204838,-0.0033118988125));
#34061=CARTESIAN_POINT('',(0.00234186610892243,0.00646875000204839,-0.00234186610892243));
#34062=CARTESIAN_POINT('',(0.0033118988125,0.00637500000204839,-0.00137183340534485));
#34063=CARTESIAN_POINT('',(0.0033118988125,0.00628125000204839,-4.05590627982804E-19));
#34064=CARTESIAN_POINT('',(3.25260651745651E-18,0.0104430389370738,6.50521303491303E-18));
#34065=CARTESIAN_POINT('',(-0.0033118988125,0.0114375000020484,0.));
#34066=CARTESIAN_POINT('',(0.0033118988125,0.00618750000204839,-4.05590627982804E-19));
#34067=CARTESIAN_POINT('',(-0.0033118988125,0.0114375000020484,0.));
#34068=CARTESIAN_POINT('',(2.35858394177587E-50,0.006,1.92592994438723E-34));
#34069=CARTESIAN_POINT('',(0.0025,0.006,-3.38118020664279E-19));
#34070=CARTESIAN_POINT('',(0.0025,0.00614062500204839,-3.06161699786838E-19));
#34071=CARTESIAN_POINT('',(-0.0033118988125,0.0114375000020484,0.));
#34072=CARTESIAN_POINT('',(-0.0025,0.0114375000020484,0.));
#34073=CARTESIAN_POINT('',(0.,0.012,0.));
#34074=CARTESIAN_POINT('',(0.,0.012,0.));
#34075=CARTESIAN_POINT('',(0.,0.012,0.));
#34076=CARTESIAN_POINT('',(0.,0.012,0.002));
#34077=CARTESIAN_POINT('',(0.,0.,0.));
#34078=CARTESIAN_POINT('',(0.005,0.,0.));
#34079=CARTESIAN_POINT('',(0.00449037034920393,0.,0.000294234816074125));
#34080=CARTESIAN_POINT('',(0.005,2.89120579329468E-19,0.));
#34081=CARTESIAN_POINT('',(0.,0.,0.));
#34082=CARTESIAN_POINT('',(0.00449035995854428,0.,0.000294393346905451));
#34083=CARTESIAN_POINT('',(0.00495722430686905,0.,0.000652630961100258));
#34084=CARTESIAN_POINT('',(0.00495722430686905,2.89120579329468E-19,0.000652630961100258));
#34085=CARTESIAN_POINT('',(0.00495722430686905,0.,0.000652630961100258));
#34086=CARTESIAN_POINT('',(0.00441354925822283,0.,0.000877828539773374));
#34087=CARTESIAN_POINT('',(0.,0.,0.));
#34088=CARTESIAN_POINT('',(0.00441351826403096,0.,0.000877984358098221));
#34089=CARTESIAN_POINT('',(0.00482962913144534,0.,0.0012940952255126));
#34090=CARTESIAN_POINT('',(0.00482962913144534,0.,0.0012940952255126));
#34091=CARTESIAN_POINT('',(0.00482962913144534,0.,0.0012940952255126));
#34092=CARTESIAN_POINT('',(0.00426121111576652,2.89120579329468E-19,0.00144640237377705));
#34093=CARTESIAN_POINT('',(0.,0.,0.));
#34094=CARTESIAN_POINT('',(0.00426116004836162,0.,0.00144655281350068));
#34095=CARTESIAN_POINT('',(0.00461939766255643,0.,0.00191341716182545));
#34096=CARTESIAN_POINT('',(0.00461939766255643,0.,0.00191341716182545));
#34097=CARTESIAN_POINT('',(0.00461939766255643,0.,0.00191341716182545));
#34098=CARTESIAN_POINT('',(0.00403596246968851,0.,0.00199022786214689));
#34099=CARTESIAN_POINT('',(0.,0.,0.));
#34100=CARTESIAN_POINT('',(0.00403589220284807,0.,0.00199037034920393));
#34101=CARTESIAN_POINT('',(0.00433012701892219,0.,0.0025));
#34102=CARTESIAN_POINT('',(0.00433012701892219,2.89120579329468E-19,0.0025));
#34103=CARTESIAN_POINT('',(0.00433012701892219,0.,0.0025));
#34104=CARTESIAN_POINT('',(0.00374165738677394,0.,0.0025));
#34105=CARTESIAN_POINT('',(0.,0.,0.));
#34106=CARTESIAN_POINT('',(0.00374156912278306,0.,0.00250013209639738));
#34107=CARTESIAN_POINT('',(0.00396676670145617,0.,0.0030438071450436));
#34108=CARTESIAN_POINT('',(0.00396676670145617,2.89120579329468E-19,0.0030438071450436));
#34109=CARTESIAN_POINT('',(0.00396676670145617,0.,0.0030438071450436));
#34110=CARTESIAN_POINT('',(0.00338333150858826,2.89120579329468E-19,0.00296699644472216));
#34111=CARTESIAN_POINT('',(0.,0.,0.));
#34112=CARTESIAN_POINT('',(0.00338322675766829,0.,0.00296711589025391));
#34113=CARTESIAN_POINT('',(0.00353553390593274,0.,0.00353553390593274));
#34114=CARTESIAN_POINT('',(0.00353553390593274,0.,0.00353553390593274));
#34115=CARTESIAN_POINT('',(0.00353553390593274,0.,0.00353553390593274));
#34116=CARTESIAN_POINT('',(0.00296711589025391,0.,0.00338322675766829));
#34117=CARTESIAN_POINT('',(0.,0.,0.));
#34118=CARTESIAN_POINT('',(0.00296699644472216,0.,0.00338333150858826));
#34119=CARTESIAN_POINT('',(0.0030438071450436,0.,0.00396676670145617));
#34120=CARTESIAN_POINT('',(0.0030438071450436,0.,0.00396676670145617));
#34121=CARTESIAN_POINT('',(0.0030438071450436,0.,0.00396676670145617));
#34122=CARTESIAN_POINT('',(0.00250013209639738,0.,0.00374156912278306));
#34123=CARTESIAN_POINT('',(0.,0.,0.));
#34124=CARTESIAN_POINT('',(0.0025,0.,0.00374165738677394));
#34125=CARTESIAN_POINT('',(0.0025,0.,0.00433012701892219));
#34126=CARTESIAN_POINT('',(0.0025,0.,0.00433012701892219));
#34127=CARTESIAN_POINT('',(0.0025,0.,0.00433012701892219));
#34128=CARTESIAN_POINT('',(0.00199037034920393,0.,0.00403589220284807));
#34129=CARTESIAN_POINT('',(0.,0.,0.));
#34130=CARTESIAN_POINT('',(0.00199022786214689,0.,0.00403596246968851));
#34131=CARTESIAN_POINT('',(0.00191341716182545,0.,0.00461939766255643));
#34132=CARTESIAN_POINT('',(0.00191341716182545,0.,0.00461939766255643));
#34133=CARTESIAN_POINT('',(0.00191341716182545,0.,0.00461939766255643));
#34134=CARTESIAN_POINT('',(0.00144655281350068,0.,0.00426116004836163));
#34135=CARTESIAN_POINT('',(0.,0.,0.));
#34136=CARTESIAN_POINT('',(0.00144640237377705,0.,0.00426121111576652));
#34137=CARTESIAN_POINT('',(0.0012940952255126,0.,0.00482962913144534));
#34138=CARTESIAN_POINT('',(0.0012940952255126,0.,0.00482962913144534));
#34139=CARTESIAN_POINT('',(0.0012940952255126,0.,0.00482962913144534));
#34140=CARTESIAN_POINT('',(0.000877984358098221,2.89120579329468E-19,0.00441351826403096));
#34141=CARTESIAN_POINT('',(0.,0.,0.));
#34142=CARTESIAN_POINT('',(0.000877828539773374,0.,0.00441354925822283));
#34143=CARTESIAN_POINT('',(0.000652630961100259,0.,0.00495722430686905));
#34144=CARTESIAN_POINT('',(0.000652630961100259,2.89120579329468E-19,0.00495722430686905));
#34145=CARTESIAN_POINT('',(0.000652630961100259,0.,0.00495722430686905));
#34146=CARTESIAN_POINT('',(0.000294393346905451,0.,0.00449035995854428));
#34147=CARTESIAN_POINT('',(0.,0.,0.));
#34148=CARTESIAN_POINT('',(0.000294234816074127,0.,0.00449037034920393));
#34149=CARTESIAN_POINT('',(3.06161699786893E-19,0.,0.005));
#34150=CARTESIAN_POINT('',(3.06161699786893E-19,2.89120579329468E-19,0.005));
#34151=CARTESIAN_POINT('',(3.06161699786893E-19,0.,0.005));
#34152=CARTESIAN_POINT('',(-0.000294234816074128,0.,0.00449037034920393));
#34153=CARTESIAN_POINT('',(0.,0.,0.));
#34154=CARTESIAN_POINT('',(-0.00029439334690545,0.,0.00449035995854428));
#34155=CARTESIAN_POINT('',(-0.000652630961100257,0.,0.00495722430686905));
#34156=CARTESIAN_POINT('',(-0.000652630961100257,0.,0.00495722430686905));
#34157=CARTESIAN_POINT('',(-0.000652630961100257,0.,0.00495722430686905));
#34158=CARTESIAN_POINT('',(-0.000877828539773374,0.,0.00441354925822283));
#34159=CARTESIAN_POINT('',(0.,0.,0.));
#34160=CARTESIAN_POINT('',(-0.000877984358098222,0.,0.00441351826403096));
#34161=CARTESIAN_POINT('',(-0.0012940952255126,0.,0.00482962913144534));
#34162=CARTESIAN_POINT('',(-0.0012940952255126,0.,0.00482962913144534));
#34163=CARTESIAN_POINT('',(-0.0012940952255126,0.,0.00482962913144534));
#34164=CARTESIAN_POINT('',(-0.00144640237377705,0.,0.00426121111576652));
#34165=CARTESIAN_POINT('',(0.,0.,0.));
#34166=CARTESIAN_POINT('',(-0.00144655281350068,0.,0.00426116004836162));
#34167=CARTESIAN_POINT('',(-0.00191341716182545,0.,0.00461939766255643));
#34168=CARTESIAN_POINT('',(-0.00191341716182545,0.,0.00461939766255643));
#34169=CARTESIAN_POINT('',(-0.00191341716182545,0.,0.00461939766255643));
#34170=CARTESIAN_POINT('',(-0.00199022786214689,2.16840434497101E-19,0.00403596246968851));
#34171=CARTESIAN_POINT('',(0.,0.,0.));
#34172=CARTESIAN_POINT('',(-0.00199037034920393,0.,0.00403589220284807));
#34173=CARTESIAN_POINT('',(-0.0025,0.,0.00433012701892219));
#34174=CARTESIAN_POINT('',(-0.0025,2.89120579329468E-19,0.00433012701892219));
#34175=CARTESIAN_POINT('',(-0.0025,0.,0.00433012701892219));
#34176=CARTESIAN_POINT('',(-0.0025,0.,0.00374165738677394));
#34177=CARTESIAN_POINT('',(0.,0.,0.));
#34178=CARTESIAN_POINT('',(-0.00250013209639738,0.,0.00374156912278306));
#34179=CARTESIAN_POINT('',(-0.0030438071450436,0.,0.00396676670145617));
#34180=CARTESIAN_POINT('',(-0.0030438071450436,0.,0.00396676670145617));
#34181=CARTESIAN_POINT('',(-0.0030438071450436,0.,0.00396676670145617));
#34182=CARTESIAN_POINT('',(-0.00296699644472215,0.,0.00338333150858826));
#34183=CARTESIAN_POINT('',(0.,0.,0.));
#34184=CARTESIAN_POINT('',(-0.00296711589025392,0.,0.00338322675766829));
#34185=CARTESIAN_POINT('',(-0.00353553390593274,0.,0.00353553390593274));
#34186=CARTESIAN_POINT('',(-0.00353553390593274,0.,0.00353553390593274));
#34187=CARTESIAN_POINT('',(-0.00353553390593274,0.,0.00353553390593274));
#34188=CARTESIAN_POINT('',(-0.00338322675766829,0.,0.00296711589025391));
#34189=CARTESIAN_POINT('',(0.,0.,0.));
#34190=CARTESIAN_POINT('',(-0.00338333150858826,0.,0.00296699644472216));
#34191=CARTESIAN_POINT('',(-0.00396676670145617,0.,0.0030438071450436));
#34192=CARTESIAN_POINT('',(-0.00396676670145617,0.,0.0030438071450436));
#34193=CARTESIAN_POINT('',(-0.00396676670145617,0.,0.0030438071450436));
#34194=CARTESIAN_POINT('',(-0.00374156912278306,0.,0.00250013209639738));
#34195=CARTESIAN_POINT('',(0.,0.,0.));
#34196=CARTESIAN_POINT('',(-0.00374165738677394,0.,0.0025));
#34197=CARTESIAN_POINT('',(-0.00433012701892219,0.,0.0025));
#34198=CARTESIAN_POINT('',(-0.00433012701892219,0.,0.0025));
#34199=CARTESIAN_POINT('',(-0.00433012701892219,0.,0.0025));
#34200=CARTESIAN_POINT('',(-0.00403589220284807,0.,0.00199037034920393));
#34201=CARTESIAN_POINT('',(0.,0.,0.));
#34202=CARTESIAN_POINT('',(-0.00403596246968851,0.,0.00199022786214689));
#34203=CARTESIAN_POINT('',(-0.00461939766255643,0.,0.00191341716182545));
#34204=CARTESIAN_POINT('',(-0.00461939766255643,0.,0.00191341716182545));
#34205=CARTESIAN_POINT('',(-0.00461939766255643,0.,0.00191341716182545));
#34206=CARTESIAN_POINT('',(-0.00426116004836163,0.,0.00144655281350068));
#34207=CARTESIAN_POINT('',(0.,0.,0.));
#34208=CARTESIAN_POINT('',(-0.00426121111576652,0.,0.00144640237377705));
#34209=CARTESIAN_POINT('',(-0.00482962913144534,0.,0.0012940952255126));
#34210=CARTESIAN_POINT('',(-0.00482962913144534,0.,0.0012940952255126));
#34211=CARTESIAN_POINT('',(-0.00482962913144534,0.,0.0012940952255126));
#34212=CARTESIAN_POINT('',(-0.00441351826403096,2.89120579329468E-19,0.000877984358098221));
#34213=CARTESIAN_POINT('',(0.,0.,0.));
#34214=CARTESIAN_POINT('',(-0.00441354925822283,0.,0.000877828539773374));
#34215=CARTESIAN_POINT('',(-0.00495722430686905,0.,0.00065263096110026));
#34216=CARTESIAN_POINT('',(-0.00495722430686905,0.,0.00065263096110026));
#34217=CARTESIAN_POINT('',(-0.00495722430686905,0.,0.00065263096110026));
#34218=CARTESIAN_POINT('',(-0.00449035995854428,0.,0.000294393346905453));
#34219=CARTESIAN_POINT('',(0.,0.,0.));
#34220=CARTESIAN_POINT('',(-0.00449037034920393,0.,0.000294234816074127));
#34221=CARTESIAN_POINT('',(-0.005,0.,6.12323399573786E-19));
#34222=CARTESIAN_POINT('',(-0.005,0.,6.12323399573786E-19));
#34223=CARTESIAN_POINT('',(-0.005,0.,6.12323399573786E-19));
#34224=CARTESIAN_POINT('',(-0.00449037034920393,0.,-0.000294234816074128));
#34225=CARTESIAN_POINT('',(0.,0.,0.));
#34226=CARTESIAN_POINT('',(-0.00449035995854428,0.,-0.000294393346905449));
#34227=CARTESIAN_POINT('',(-0.00495722430686905,0.,-0.000652630961100257));
#34228=CARTESIAN_POINT('',(-0.00495722430686905,0.,-0.000652630961100257));
#34229=CARTESIAN_POINT('',(-0.00495722430686905,0.,-0.000652630961100257));
#34230=CARTESIAN_POINT('',(-0.00441354925822283,0.,-0.000877828539773374));
#34231=CARTESIAN_POINT('',(0.,0.,0.));
#34232=CARTESIAN_POINT('',(-0.00441351826403096,0.,-0.000877984358098219));
#34233=CARTESIAN_POINT('',(-0.00482962913144534,0.,-0.0012940952255126));
#34234=CARTESIAN_POINT('',(-0.00482962913144534,2.89120579329468E-19,-0.0012940952255126));
#34235=CARTESIAN_POINT('',(-0.00482962913144534,0.,-0.0012940952255126));
#34236=CARTESIAN_POINT('',(-0.00426121111576652,0.,-0.00144640237377705));
#34237=CARTESIAN_POINT('',(0.,0.,0.));
#34238=CARTESIAN_POINT('',(-0.00426116004836163,0.,-0.00144655281350068));
#34239=CARTESIAN_POINT('',(-0.00461939766255644,0.,-0.00191341716182544));
#34240=CARTESIAN_POINT('',(-0.00461939766255644,0.,-0.00191341716182544));
#34241=CARTESIAN_POINT('',(-0.00461939766255644,0.,-0.00191341716182544));
#34242=CARTESIAN_POINT('',(-0.00403596246968851,0.,-0.00199022786214689));
#34243=CARTESIAN_POINT('',(0.,0.,0.));
#34244=CARTESIAN_POINT('',(-0.00403589220284807,0.,-0.00199037034920393));
#34245=CARTESIAN_POINT('',(-0.00433012701892219,0.,-0.0025));
#34246=CARTESIAN_POINT('',(-0.00433012701892219,2.89120579329468E-19,-0.0025));
#34247=CARTESIAN_POINT('',(-0.00433012701892219,0.,-0.0025));
#34248=CARTESIAN_POINT('',(-0.00374165738677394,0.,-0.0025));
#34249=CARTESIAN_POINT('',(0.,0.,0.));
#34250=CARTESIAN_POINT('',(-0.00374156912278306,0.,-0.00250013209639738));
#34251=CARTESIAN_POINT('',(-0.00396676670145617,0.,-0.0030438071450436));
#34252=CARTESIAN_POINT('',(-0.00396676670145617,0.,-0.0030438071450436));
#34253=CARTESIAN_POINT('',(-0.00396676670145617,0.,-0.0030438071450436));
#34254=CARTESIAN_POINT('',(-0.00338333150858826,0.,-0.00296699644472216));
#34255=CARTESIAN_POINT('',(0.,0.,0.));
#34256=CARTESIAN_POINT('',(-0.00338322675766829,0.,-0.00296711589025391));
#34257=CARTESIAN_POINT('',(-0.00353553390593274,0.,-0.00353553390593274));
#34258=CARTESIAN_POINT('',(-0.00353553390593274,0.,-0.00353553390593274));
#34259=CARTESIAN_POINT('',(-0.00353553390593274,0.,-0.00353553390593274));
#34260=CARTESIAN_POINT('',(-0.00296711589025391,0.,-0.00338322675766829));
#34261=CARTESIAN_POINT('',(0.,0.,0.));
#34262=CARTESIAN_POINT('',(-0.00296699644472216,0.,-0.00338333150858826));
#34263=CARTESIAN_POINT('',(-0.0030438071450436,0.,-0.00396676670145617));
#34264=CARTESIAN_POINT('',(-0.0030438071450436,0.,-0.00396676670145617));
#34265=CARTESIAN_POINT('',(-0.0030438071450436,0.,-0.00396676670145617));
#34266=CARTESIAN_POINT('',(-0.00250013209639738,0.,-0.00374156912278306));
#34267=CARTESIAN_POINT('',(0.,0.,0.));
#34268=CARTESIAN_POINT('',(-0.0025,0.,-0.00374165738677394));
#34269=CARTESIAN_POINT('',(-0.0025,0.,-0.00433012701892219));
#34270=CARTESIAN_POINT('',(-0.0025,0.,-0.00433012701892219));
#34271=CARTESIAN_POINT('',(-0.0025,0.,-0.00433012701892219));
#34272=CARTESIAN_POINT('',(-0.00199037034920393,0.,-0.00403589220284807));
#34273=CARTESIAN_POINT('',(0.,0.,0.));
#34274=CARTESIAN_POINT('',(-0.0019902278621469,0.,-0.00403596246968851));
#34275=CARTESIAN_POINT('',(-0.00191341716182545,0.,-0.00461939766255643));
#34276=CARTESIAN_POINT('',(-0.00191341716182545,0.,-0.00461939766255643));
#34277=CARTESIAN_POINT('',(-0.00191341716182545,0.,-0.00461939766255643));
#34278=CARTESIAN_POINT('',(-0.00144655281350068,0.,-0.00426116004836162));
#34279=CARTESIAN_POINT('',(0.,0.,0.));
#34280=CARTESIAN_POINT('',(-0.00144640237377705,0.,-0.00426121111576652));
#34281=CARTESIAN_POINT('',(-0.00129409522551261,0.,-0.00482962913144534));
#34282=CARTESIAN_POINT('',(-0.00129409522551261,0.,-0.00482962913144534));
#34283=CARTESIAN_POINT('',(-0.00129409522551261,0.,-0.00482962913144534));
#34284=CARTESIAN_POINT('',(-0.000877984358098223,0.,-0.00441351826403096));
#34285=CARTESIAN_POINT('',(0.,0.,0.));
#34286=CARTESIAN_POINT('',(-0.000877828539773377,0.,-0.00441354925822283));
#34287=CARTESIAN_POINT('',(-0.000652630961100263,0.,-0.00495722430686905));
#34288=CARTESIAN_POINT('',(-0.000652630961100263,0.,-0.00495722430686905));
#34289=CARTESIAN_POINT('',(-0.000652630961100263,0.,-0.00495722430686905));
#34290=CARTESIAN_POINT('',(-0.000294393346905453,0.,-0.00449035995854428));
#34291=CARTESIAN_POINT('',(0.,0.,0.));
#34292=CARTESIAN_POINT('',(-0.000294234816074127,0.,-0.00449037034920393));
#34293=CARTESIAN_POINT('',(-9.18485099360482E-19,0.,-0.005));
#34294=CARTESIAN_POINT('',(-9.18485099360482E-19,0.,-0.005));
#34295=CARTESIAN_POINT('',(-9.18485099360482E-19,0.,-0.005));
#34296=CARTESIAN_POINT('',(0.000294234816074127,0.,-0.00449037034920393));
#34297=CARTESIAN_POINT('',(0.,0.,0.));
#34298=CARTESIAN_POINT('',(0.00029439334690545,0.,-0.00449035995854428));
#34299=CARTESIAN_POINT('',(0.000652630961100256,0.,-0.00495722430686905));
#34300=CARTESIAN_POINT('',(0.000652630961100256,0.,-0.00495722430686905));
#34301=CARTESIAN_POINT('',(0.000652630961100256,0.,-0.00495722430686905));
#34302=CARTESIAN_POINT('',(0.000877828539773373,0.,-0.00441354925822283));
#34303=CARTESIAN_POINT('',(0.,0.,0.));
#34304=CARTESIAN_POINT('',(0.000877984358098219,0.,-0.00441351826403096));
#34305=CARTESIAN_POINT('',(0.0012940952255126,0.,-0.00482962913144534));
#34306=CARTESIAN_POINT('',(0.0012940952255126,0.,-0.00482962913144534));
#34307=CARTESIAN_POINT('',(0.0012940952255126,0.,-0.00482962913144534));
#34308=CARTESIAN_POINT('',(0.00144640237377704,1.44560289664734E-19,-0.00426121111576652));
#34309=CARTESIAN_POINT('',(0.,0.,0.));
#34310=CARTESIAN_POINT('',(0.00144655281350067,0.,-0.00426116004836163));
#34311=CARTESIAN_POINT('',(0.00191341716182544,0.,-0.00461939766255644));
#34312=CARTESIAN_POINT('',(0.00191341716182544,0.,-0.00461939766255644));
#34313=CARTESIAN_POINT('',(0.00191341716182544,0.,-0.00461939766255644));
#34314=CARTESIAN_POINT('',(0.00199022786214689,0.,-0.00403596246968851));
#34315=CARTESIAN_POINT('',(0.,0.,0.));
#34316=CARTESIAN_POINT('',(0.00199037034920392,0.,-0.00403589220284807));
#34317=CARTESIAN_POINT('',(0.0025,0.,-0.00433012701892219));
#34318=CARTESIAN_POINT('',(0.0025,0.,-0.00433012701892219));
#34319=CARTESIAN_POINT('',(0.0025,0.,-0.00433012701892219));
#34320=CARTESIAN_POINT('',(0.0025,0.,-0.00374165738677394));
#34321=CARTESIAN_POINT('',(0.,0.,0.));
#34322=CARTESIAN_POINT('',(0.00250013209639738,0.,-0.00374156912278307));
#34323=CARTESIAN_POINT('',(0.0030438071450436,0.,-0.00396676670145618));
#34324=CARTESIAN_POINT('',(0.0030438071450436,2.89120579329468E-19,-0.00396676670145618));
#34325=CARTESIAN_POINT('',(0.0030438071450436,0.,-0.00396676670145618));
#34326=CARTESIAN_POINT('',(0.00296699644472215,0.,-0.00338333150858826));
#34327=CARTESIAN_POINT('',(0.,0.,0.));
#34328=CARTESIAN_POINT('',(0.00296711589025391,0.,-0.00338322675766829));
#34329=CARTESIAN_POINT('',(0.00353553390593274,0.,-0.00353553390593274));
#34330=CARTESIAN_POINT('',(0.00353553390593274,0.,-0.00353553390593274));
#34331=CARTESIAN_POINT('',(0.00353553390593274,0.,-0.00353553390593274));
#34332=CARTESIAN_POINT('',(0.00338322675766829,0.,-0.00296711589025392));
#34333=CARTESIAN_POINT('',(0.,0.,0.));
#34334=CARTESIAN_POINT('',(0.00338333150858826,0.,-0.00296699644472216));
#34335=CARTESIAN_POINT('',(0.00396676670145617,0.,-0.0030438071450436));
#34336=CARTESIAN_POINT('',(0.00396676670145617,0.,-0.0030438071450436));
#34337=CARTESIAN_POINT('',(0.00396676670145617,0.,-0.0030438071450436));
#34338=CARTESIAN_POINT('',(0.00374165738677394,0.,-0.0025));
#34339=CARTESIAN_POINT('',(0.00433012701892219,0.,-0.0025));
#34340=CARTESIAN_POINT('',(0.00433012701892219,0.,-0.0025));
#34341=CARTESIAN_POINT('',(0.00433012701892219,0.,-0.0025));
#34342=CARTESIAN_POINT('',(0.00403589220284806,0.,-0.00199037034920393));
#34343=CARTESIAN_POINT('',(0.,0.,0.));
#34344=CARTESIAN_POINT('',(0.00403596246968851,0.,-0.0019902278621469));
#34345=CARTESIAN_POINT('',(0.00461939766255643,0.,-0.00191341716182545));
#34346=CARTESIAN_POINT('',(0.00461939766255643,0.,-0.00191341716182545));
#34347=CARTESIAN_POINT('',(0.00461939766255643,0.,-0.00191341716182545));
#34348=CARTESIAN_POINT('',(0.00426116004836162,0.,-0.00144655281350068));
#34349=CARTESIAN_POINT('',(0.,0.,0.));
#34350=CARTESIAN_POINT('',(0.00426121111576652,0.,-0.00144640237377705));
#34351=CARTESIAN_POINT('',(0.00482962913144534,0.,-0.00129409522551261));
#34352=CARTESIAN_POINT('',(0.00482962913144534,2.89120579329468E-19,-0.00129409522551261));
#34353=CARTESIAN_POINT('',(0.00482962913144534,0.,-0.00129409522551261));
#34354=CARTESIAN_POINT('',(0.00441351826403096,2.89120579329468E-19,-0.000877984358098224));
#34355=CARTESIAN_POINT('',(0.,0.,0.));
#34356=CARTESIAN_POINT('',(0.00441354925822283,0.,-0.000877828539773378));
#34357=CARTESIAN_POINT('',(0.00495722430686905,0.,-0.000652630961100263));
#34358=CARTESIAN_POINT('',(0.00495722430686905,0.,-0.000652630961100263));
#34359=CARTESIAN_POINT('',(0.00495722430686905,0.,-0.000652630961100263));
#34360=CARTESIAN_POINT('',(0.00449035995854428,0.,-0.000294393346905455));
#34361=CARTESIAN_POINT('',(0.,0.,0.));
#34362=CARTESIAN_POINT('',(0.00449037034920393,0.,-0.000294234816074128));
#34363=CARTESIAN_POINT('',(0.005,0.,0.));
#34364=CARTESIAN_POINT('',(0.,0.,0.));
#34365=CARTESIAN_POINT('',(0.,0.,-0.00025));
#34366=CARTESIAN_POINT('',(0.,0.004,0.));
#34367=CARTESIAN_POINT('',(0.005,0.004,0.));
#34368=CARTESIAN_POINT('',(0.00449037034920393,0.004,0.000294234816074125));
#34369=CARTESIAN_POINT('',(0.005,0.004,0.));
#34370=CARTESIAN_POINT('',(0.005,0.004,0.));
#34371=CARTESIAN_POINT('',(0.00449037034920393,0.004,-0.000294234816074128));
#34372=CARTESIAN_POINT('',(0.,0.004,0.));
#34373=CARTESIAN_POINT('',(0.00449035995854428,0.004,-0.000294393346905455));
#34374=CARTESIAN_POINT('',(0.00495722430686905,0.004,-0.000652630961100263));
#34375=CARTESIAN_POINT('',(0.00495722430686905,0.004,-0.000652630961100263));
#34376=CARTESIAN_POINT('',(0.00495722430686905,0.004,-0.000652630961100263));
#34377=CARTESIAN_POINT('',(0.00441354925822283,0.004,-0.000877828539773378));
#34378=CARTESIAN_POINT('',(0.,0.004,0.));
#34379=CARTESIAN_POINT('',(0.00441351826403096,0.004,-0.000877984358098224));
#34380=CARTESIAN_POINT('',(0.00482962913144534,0.004,-0.00129409522551261));
#34381=CARTESIAN_POINT('',(0.00482962913144534,0.004,-0.00129409522551261));
#34382=CARTESIAN_POINT('',(0.00482962913144534,0.004,-0.00129409522551261));
#34383=CARTESIAN_POINT('',(0.00426121111576652,0.004,-0.00144640237377705));
#34384=CARTESIAN_POINT('',(0.,0.004,0.));
#34385=CARTESIAN_POINT('',(0.00426116004836162,0.004,-0.00144655281350068));
#34386=CARTESIAN_POINT('',(0.00461939766255643,0.004,-0.00191341716182545));
#34387=CARTESIAN_POINT('',(0.00461939766255643,0.004,-0.00191341716182545));
#34388=CARTESIAN_POINT('',(0.00461939766255643,0.004,-0.00191341716182545));
#34389=CARTESIAN_POINT('',(0.00403596246968851,0.004,-0.0019902278621469));
#34390=CARTESIAN_POINT('',(0.,0.004,0.));
#34391=CARTESIAN_POINT('',(0.00403589220284806,0.004,-0.00199037034920393));
#34392=CARTESIAN_POINT('',(0.00433012701892219,0.004,-0.0025));
#34393=CARTESIAN_POINT('',(0.00433012701892219,0.004,-0.0025));
#34394=CARTESIAN_POINT('',(0.00433012701892219,0.004,-0.0025));
#34395=CARTESIAN_POINT('',(0.00374165738677394,0.004,-0.0025));
#34396=CARTESIAN_POINT('',(0.00396676670145617,0.004,-0.0030438071450436));
#34397=CARTESIAN_POINT('',(0.00396676670145617,0.004,-0.0030438071450436));
#34398=CARTESIAN_POINT('',(0.00396676670145617,0.004,-0.0030438071450436));
#34399=CARTESIAN_POINT('',(0.00338333150858826,0.004,-0.00296699644472216));
#34400=CARTESIAN_POINT('',(0.,0.004,0.));
#34401=CARTESIAN_POINT('',(0.00338322675766829,0.004,-0.00296711589025392));
#34402=CARTESIAN_POINT('',(0.00353553390593274,0.004,-0.00353553390593274));
#34403=CARTESIAN_POINT('',(0.00353553390593274,0.004,-0.00353553390593274));
#34404=CARTESIAN_POINT('',(0.00353553390593274,0.004,-0.00353553390593274));
#34405=CARTESIAN_POINT('',(0.00296711589025391,0.004,-0.00338322675766829));
#34406=CARTESIAN_POINT('',(0.,0.004,0.));
#34407=CARTESIAN_POINT('',(0.00296699644472215,0.004,-0.00338333150858826));
#34408=CARTESIAN_POINT('',(0.0030438071450436,0.004,-0.00396676670145618));
#34409=CARTESIAN_POINT('',(0.0030438071450436,0.004,-0.00396676670145618));
#34410=CARTESIAN_POINT('',(0.0030438071450436,0.004,-0.00396676670145618));
#34411=CARTESIAN_POINT('',(0.00250013209639738,0.004,-0.00374156912278307));
#34412=CARTESIAN_POINT('',(0.,0.004,0.));
#34413=CARTESIAN_POINT('',(0.0025,0.004,-0.00374165738677394));
#34414=CARTESIAN_POINT('',(0.0025,0.004,-0.00433012701892219));
#34415=CARTESIAN_POINT('',(0.0025,0.004,-0.00433012701892219));
#34416=CARTESIAN_POINT('',(0.0025,0.004,-0.00433012701892219));
#34417=CARTESIAN_POINT('',(0.00199037034920392,0.004,-0.00403589220284807));
#34418=CARTESIAN_POINT('',(0.,0.004,0.));
#34419=CARTESIAN_POINT('',(0.00199022786214689,0.004,-0.00403596246968851));
#34420=CARTESIAN_POINT('',(0.00191341716182544,0.004,-0.00461939766255644));
#34421=CARTESIAN_POINT('',(0.00191341716182544,0.004,-0.00461939766255644));
#34422=CARTESIAN_POINT('',(0.00191341716182544,0.004,-0.00461939766255644));
#34423=CARTESIAN_POINT('',(0.00144655281350068,0.004,-0.00426116004836163));
#34424=CARTESIAN_POINT('',(0.,0.004,0.));
#34425=CARTESIAN_POINT('',(0.00144640237377704,0.004,-0.00426121111576652));
#34426=CARTESIAN_POINT('',(0.0012940952255126,0.004,-0.00482962913144534));
#34427=CARTESIAN_POINT('',(0.0012940952255126,0.004,-0.00482962913144534));
#34428=CARTESIAN_POINT('',(0.0012940952255126,0.004,-0.00482962913144534));
#34429=CARTESIAN_POINT('',(0.000877984358098219,0.004,-0.00441351826403096));
#34430=CARTESIAN_POINT('',(0.,0.004,0.));
#34431=CARTESIAN_POINT('',(0.000877828539773373,0.004,-0.00441354925822283));
#34432=CARTESIAN_POINT('',(0.000652630961100256,0.004,-0.00495722430686905));
#34433=CARTESIAN_POINT('',(0.000652630961100256,0.004,-0.00495722430686905));
#34434=CARTESIAN_POINT('',(0.000652630961100256,0.004,-0.00495722430686905));
#34435=CARTESIAN_POINT('',(0.00029439334690545,0.004,-0.00449035995854428));
#34436=CARTESIAN_POINT('',(0.,0.004,0.));
#34437=CARTESIAN_POINT('',(0.000294234816074127,0.004,-0.00449037034920393));
#34438=CARTESIAN_POINT('',(-9.18485099360482E-19,0.004,-0.005));
#34439=CARTESIAN_POINT('',(-9.18485099360482E-19,0.004,-0.005));
#34440=CARTESIAN_POINT('',(-9.18485099360482E-19,0.004,-0.005));
#34441=CARTESIAN_POINT('',(-0.000294234816074127,0.004,-0.00449037034920393));
#34442=CARTESIAN_POINT('',(0.,0.004,0.));
#34443=CARTESIAN_POINT('',(-0.000294393346905453,0.004,-0.00449035995854428));
#34444=CARTESIAN_POINT('',(-0.000652630961100263,0.004,-0.00495722430686905));
#34445=CARTESIAN_POINT('',(-0.000652630961100263,0.004,-0.00495722430686905));
#34446=CARTESIAN_POINT('',(-0.000652630961100263,0.004,-0.00495722430686905));
#34447=CARTESIAN_POINT('',(-0.000877828539773377,0.004,-0.00441354925822283));
#34448=CARTESIAN_POINT('',(0.,0.004,0.));
#34449=CARTESIAN_POINT('',(-0.000877984358098223,0.004,-0.00441351826403096));
#34450=CARTESIAN_POINT('',(-0.00129409522551261,0.004,-0.00482962913144534));
#34451=CARTESIAN_POINT('',(-0.00129409522551261,0.004,-0.00482962913144534));
#34452=CARTESIAN_POINT('',(-0.00129409522551261,0.004,-0.00482962913144534));
#34453=CARTESIAN_POINT('',(-0.00144640237377705,0.004,-0.00426121111576652));
#34454=CARTESIAN_POINT('',(0.,0.004,0.));
#34455=CARTESIAN_POINT('',(-0.00144655281350068,0.004,-0.00426116004836162));
#34456=CARTESIAN_POINT('',(-0.00191341716182545,0.004,-0.00461939766255643));
#34457=CARTESIAN_POINT('',(-0.00191341716182545,0.004,-0.00461939766255643));
#34458=CARTESIAN_POINT('',(-0.00191341716182545,0.004,-0.00461939766255643));
#34459=CARTESIAN_POINT('',(-0.0019902278621469,0.004,-0.00403596246968851));
#34460=CARTESIAN_POINT('',(0.,0.004,0.));
#34461=CARTESIAN_POINT('',(-0.00199037034920393,0.004,-0.00403589220284807));
#34462=CARTESIAN_POINT('',(-0.0025,0.004,-0.00433012701892219));
#34463=CARTESIAN_POINT('',(-0.0025,0.004,-0.00433012701892219));
#34464=CARTESIAN_POINT('',(-0.0025,0.004,-0.00433012701892219));
#34465=CARTESIAN_POINT('',(-0.0025,0.004,-0.00374165738677394));
#34466=CARTESIAN_POINT('',(0.,0.004,0.));
#34467=CARTESIAN_POINT('',(-0.00250013209639738,0.004,-0.00374156912278306));
#34468=CARTESIAN_POINT('',(-0.0030438071450436,0.004,-0.00396676670145617));
#34469=CARTESIAN_POINT('',(-0.0030438071450436,0.004,-0.00396676670145617));
#34470=CARTESIAN_POINT('',(-0.0030438071450436,0.004,-0.00396676670145617));
#34471=CARTESIAN_POINT('',(-0.00296699644472216,0.004,-0.00338333150858826));
#34472=CARTESIAN_POINT('',(0.,0.004,0.));
#34473=CARTESIAN_POINT('',(-0.00296711589025392,0.004,-0.00338322675766829));
#34474=CARTESIAN_POINT('',(-0.00353553390593274,0.004,-0.00353553390593274));
#34475=CARTESIAN_POINT('',(-0.00353553390593274,0.004,-0.00353553390593274));
#34476=CARTESIAN_POINT('',(-0.00353553390593274,0.004,-0.00353553390593274));
#34477=CARTESIAN_POINT('',(-0.0033832267576683,0.004,-0.00296711589025391));
#34478=CARTESIAN_POINT('',(0.,0.004,0.));
#34479=CARTESIAN_POINT('',(-0.00338333150858826,0.004,-0.00296699644472216));
#34480=CARTESIAN_POINT('',(-0.00396676670145617,0.004,-0.0030438071450436));
#34481=CARTESIAN_POINT('',(-0.00396676670145617,0.004,-0.0030438071450436));
#34482=CARTESIAN_POINT('',(-0.00396676670145617,0.004,-0.0030438071450436));
#34483=CARTESIAN_POINT('',(-0.00374156912278306,0.004,-0.00250013209639738));
#34484=CARTESIAN_POINT('',(0.,0.004,0.));
#34485=CARTESIAN_POINT('',(-0.00374165738677394,0.004,-0.0025));
#34486=CARTESIAN_POINT('',(-0.00433012701892219,0.004,-0.0025));
#34487=CARTESIAN_POINT('',(-0.00433012701892219,0.004,-0.0025));
#34488=CARTESIAN_POINT('',(-0.00433012701892219,0.004,-0.0025));
#34489=CARTESIAN_POINT('',(-0.00403589220284807,0.004,-0.00199037034920393));
#34490=CARTESIAN_POINT('',(0.,0.004,0.));
#34491=CARTESIAN_POINT('',(-0.00403596246968851,0.004,-0.00199022786214689));
#34492=CARTESIAN_POINT('',(-0.00461939766255644,0.004,-0.00191341716182544));
#34493=CARTESIAN_POINT('',(-0.00461939766255644,0.004,-0.00191341716182544));
#34494=CARTESIAN_POINT('',(-0.00461939766255644,0.004,-0.00191341716182544));
#34495=CARTESIAN_POINT('',(-0.00426116004836163,0.004,-0.00144655281350068));
#34496=CARTESIAN_POINT('',(0.,0.004,0.));
#34497=CARTESIAN_POINT('',(-0.00426121111576652,0.004,-0.00144640237377705));
#34498=CARTESIAN_POINT('',(-0.00482962913144534,0.004,-0.0012940952255126));
#34499=CARTESIAN_POINT('',(-0.00482962913144534,0.004,-0.0012940952255126));
#34500=CARTESIAN_POINT('',(-0.00482962913144534,0.004,-0.0012940952255126));
#34501=CARTESIAN_POINT('',(-0.00441351826403096,0.004,-0.00087798435809822));
#34502=CARTESIAN_POINT('',(0.,0.004,0.));
#34503=CARTESIAN_POINT('',(-0.00441354925822283,0.004,-0.000877828539773374));
#34504=CARTESIAN_POINT('',(-0.00495722430686905,0.004,-0.000652630961100257));
#34505=CARTESIAN_POINT('',(-0.00495722430686905,0.004,-0.000652630961100257));
#34506=CARTESIAN_POINT('',(-0.00495722430686905,0.004,-0.000652630961100257));
#34507=CARTESIAN_POINT('',(-0.00449035995854428,0.004,-0.00029439334690545));
#34508=CARTESIAN_POINT('',(0.,0.004,0.));
#34509=CARTESIAN_POINT('',(-0.00449037034920393,0.004,-0.000294234816074128));
#34510=CARTESIAN_POINT('',(-0.005,0.004,6.12323399573786E-19));
#34511=CARTESIAN_POINT('',(-0.005,0.004,6.12323399573786E-19));
#34512=CARTESIAN_POINT('',(-0.005,0.004,6.12323399573786E-19));
#34513=CARTESIAN_POINT('',(-0.00449037034920393,0.004,0.000294234816074127));
#34514=CARTESIAN_POINT('',(0.,0.004,0.));
#34515=CARTESIAN_POINT('',(-0.00449035995854428,0.004,0.000294393346905453));
#34516=CARTESIAN_POINT('',(-0.00495722430686905,0.004,0.00065263096110026));
#34517=CARTESIAN_POINT('',(-0.00495722430686905,0.004,0.00065263096110026));
#34518=CARTESIAN_POINT('',(-0.00495722430686905,0.004,0.00065263096110026));
#34519=CARTESIAN_POINT('',(-0.00441354925822283,0.004,0.000877828539773374));
#34520=CARTESIAN_POINT('',(0.,0.004,0.));
#34521=CARTESIAN_POINT('',(-0.00441351826403096,0.004,0.000877984358098221));
#34522=CARTESIAN_POINT('',(-0.00482962913144534,0.004,0.0012940952255126));
#34523=CARTESIAN_POINT('',(-0.00482962913144534,0.004,0.0012940952255126));
#34524=CARTESIAN_POINT('',(-0.00482962913144534,0.004,0.0012940952255126));
#34525=CARTESIAN_POINT('',(-0.00426121111576652,0.004,0.00144640237377705));
#34526=CARTESIAN_POINT('',(0.,0.004,0.));
#34527=CARTESIAN_POINT('',(-0.00426116004836163,0.004,0.00144655281350068));
#34528=CARTESIAN_POINT('',(-0.00461939766255643,0.004,0.00191341716182545));
#34529=CARTESIAN_POINT('',(-0.00461939766255643,0.004,0.00191341716182545));
#34530=CARTESIAN_POINT('',(-0.00461939766255643,0.004,0.00191341716182545));
#34531=CARTESIAN_POINT('',(-0.00403596246968851,0.004,0.00199022786214689));
#34532=CARTESIAN_POINT('',(0.,0.004,0.));
#34533=CARTESIAN_POINT('',(-0.00403589220284807,0.004,0.00199037034920393));
#34534=CARTESIAN_POINT('',(-0.00433012701892219,0.004,0.0025));
#34535=CARTESIAN_POINT('',(-0.00433012701892219,0.004,0.0025));
#34536=CARTESIAN_POINT('',(-0.00433012701892219,0.004,0.0025));
#34537=CARTESIAN_POINT('',(-0.00374165738677394,0.004,0.0025));
#34538=CARTESIAN_POINT('',(0.,0.004,0.));
#34539=CARTESIAN_POINT('',(-0.00374156912278306,0.004,0.00250013209639738));
#34540=CARTESIAN_POINT('',(-0.00396676670145617,0.004,0.0030438071450436));
#34541=CARTESIAN_POINT('',(-0.00396676670145617,0.004,0.0030438071450436));
#34542=CARTESIAN_POINT('',(-0.00396676670145617,0.004,0.0030438071450436));
#34543=CARTESIAN_POINT('',(-0.00338333150858826,0.004,0.00296699644472216));
#34544=CARTESIAN_POINT('',(0.,0.004,0.));
#34545=CARTESIAN_POINT('',(-0.00338322675766829,0.004,0.00296711589025391));
#34546=CARTESIAN_POINT('',(-0.00353553390593274,0.004,0.00353553390593274));
#34547=CARTESIAN_POINT('',(-0.00353553390593274,0.004,0.00353553390593274));
#34548=CARTESIAN_POINT('',(-0.00353553390593274,0.004,0.00353553390593274));
#34549=CARTESIAN_POINT('',(-0.00296711589025392,0.004,0.00338322675766829));
#34550=CARTESIAN_POINT('',(0.,0.004,0.));
#34551=CARTESIAN_POINT('',(-0.00296699644472215,0.004,0.00338333150858826));
#34552=CARTESIAN_POINT('',(-0.0030438071450436,0.004,0.00396676670145617));
#34553=CARTESIAN_POINT('',(-0.0030438071450436,0.004,0.00396676670145617));
#34554=CARTESIAN_POINT('',(-0.0030438071450436,0.004,0.00396676670145617));
#34555=CARTESIAN_POINT('',(-0.00250013209639738,0.004,0.00374156912278307));
#34556=CARTESIAN_POINT('',(0.,0.004,0.));
#34557=CARTESIAN_POINT('',(-0.0025,0.004,0.00374165738677394));
#34558=CARTESIAN_POINT('',(-0.0025,0.004,0.00433012701892219));
#34559=CARTESIAN_POINT('',(-0.0025,0.004,0.00433012701892219));
#34560=CARTESIAN_POINT('',(-0.0025,0.004,0.00433012701892219));
#34561=CARTESIAN_POINT('',(-0.00199037034920393,0.004,0.00403589220284807));
#34562=CARTESIAN_POINT('',(0.,0.004,0.));
#34563=CARTESIAN_POINT('',(-0.00199022786214689,0.004,0.00403596246968851));
#34564=CARTESIAN_POINT('',(-0.00191341716182545,0.004,0.00461939766255643));
#34565=CARTESIAN_POINT('',(-0.00191341716182545,0.004,0.00461939766255643));
#34566=CARTESIAN_POINT('',(-0.00191341716182545,0.004,0.00461939766255643));
#34567=CARTESIAN_POINT('',(-0.00144655281350068,0.004,0.00426116004836162));
#34568=CARTESIAN_POINT('',(0.,0.004,0.));
#34569=CARTESIAN_POINT('',(-0.00144640237377705,0.004,0.00426121111576652));
#34570=CARTESIAN_POINT('',(-0.0012940952255126,0.004,0.00482962913144534));
#34571=CARTESIAN_POINT('',(-0.0012940952255126,0.004,0.00482962913144534));
#34572=CARTESIAN_POINT('',(-0.0012940952255126,0.004,0.00482962913144534));
#34573=CARTESIAN_POINT('',(-0.000877984358098222,0.004,0.00441351826403096));
#34574=CARTESIAN_POINT('',(0.,0.004,0.));
#34575=CARTESIAN_POINT('',(-0.000877828539773373,0.004,0.00441354925822283));
#34576=CARTESIAN_POINT('',(-0.000652630961100257,0.004,0.00495722430686905));
#34577=CARTESIAN_POINT('',(-0.000652630961100257,0.004,0.00495722430686905));
#34578=CARTESIAN_POINT('',(-0.000652630961100257,0.004,0.00495722430686905));
#34579=CARTESIAN_POINT('',(-0.00029439334690545,0.004,0.00449035995854428));
#34580=CARTESIAN_POINT('',(0.,0.004,0.));
#34581=CARTESIAN_POINT('',(-0.000294234816074128,0.004,0.00449037034920393));
#34582=CARTESIAN_POINT('',(3.06161699786893E-19,0.004,0.005));
#34583=CARTESIAN_POINT('',(3.06161699786893E-19,0.004,0.005));
#34584=CARTESIAN_POINT('',(3.06161699786893E-19,0.004,0.005));
#34585=CARTESIAN_POINT('',(0.000294234816074127,0.004,0.00449037034920393));
#34586=CARTESIAN_POINT('',(0.,0.004,0.));
#34587=CARTESIAN_POINT('',(0.000294393346905452,0.004,0.00449035995854428));
#34588=CARTESIAN_POINT('',(0.000652630961100259,0.004,0.00495722430686905));
#34589=CARTESIAN_POINT('',(0.000652630961100259,0.004,0.00495722430686905));
#34590=CARTESIAN_POINT('',(0.000652630961100259,0.004,0.00495722430686905));
#34591=CARTESIAN_POINT('',(0.000877828539773374,0.004,0.00441354925822283));
#34592=CARTESIAN_POINT('',(0.,0.004,0.));
#34593=CARTESIAN_POINT('',(0.000877984358098221,0.004,0.00441351826403096));
#34594=CARTESIAN_POINT('',(0.0012940952255126,0.004,0.00482962913144534));
#34595=CARTESIAN_POINT('',(0.0012940952255126,0.004,0.00482962913144534));
#34596=CARTESIAN_POINT('',(0.0012940952255126,0.004,0.00482962913144534));
#34597=CARTESIAN_POINT('',(0.00144640237377705,0.004,0.00426121111576652));
#34598=CARTESIAN_POINT('',(0.,0.004,0.));
#34599=CARTESIAN_POINT('',(0.00144655281350068,0.004,0.00426116004836163));
#34600=CARTESIAN_POINT('',(0.00191341716182545,0.004,0.00461939766255643));
#34601=CARTESIAN_POINT('',(0.00191341716182545,0.004,0.00461939766255643));
#34602=CARTESIAN_POINT('',(0.00191341716182545,0.004,0.00461939766255643));
#34603=CARTESIAN_POINT('',(0.00199022786214689,0.004,0.00403596246968851));
#34604=CARTESIAN_POINT('',(0.,0.004,0.));
#34605=CARTESIAN_POINT('',(0.00199037034920393,0.004,0.00403589220284807));
#34606=CARTESIAN_POINT('',(0.0025,0.004,0.00433012701892219));
#34607=CARTESIAN_POINT('',(0.0025,0.004,0.00433012701892219));
#34608=CARTESIAN_POINT('',(0.0025,0.004,0.00433012701892219));
#34609=CARTESIAN_POINT('',(0.0025,0.004,0.00374165738677394));
#34610=CARTESIAN_POINT('',(0.,0.004,0.));
#34611=CARTESIAN_POINT('',(0.00250013209639738,0.004,0.00374156912278306));
#34612=CARTESIAN_POINT('',(0.0030438071450436,0.004,0.00396676670145617));
#34613=CARTESIAN_POINT('',(0.0030438071450436,0.004,0.00396676670145617));
#34614=CARTESIAN_POINT('',(0.0030438071450436,0.004,0.00396676670145617));
#34615=CARTESIAN_POINT('',(0.00296699644472216,0.004,0.00338333150858826));
#34616=CARTESIAN_POINT('',(0.,0.004,0.));
#34617=CARTESIAN_POINT('',(0.00296711589025392,0.004,0.00338322675766829));
#34618=CARTESIAN_POINT('',(0.00353553390593274,0.004,0.00353553390593274));
#34619=CARTESIAN_POINT('',(0.00353553390593274,0.004,0.00353553390593274));
#34620=CARTESIAN_POINT('',(0.00353553390593274,0.004,0.00353553390593274));
#34621=CARTESIAN_POINT('',(0.00338322675766829,0.004,0.00296711589025392));
#34622=CARTESIAN_POINT('',(0.,0.004,0.));
#34623=CARTESIAN_POINT('',(0.00338333150858826,0.004,0.00296699644472216));
#34624=CARTESIAN_POINT('',(0.00396676670145617,0.004,0.0030438071450436));
#34625=CARTESIAN_POINT('',(0.00396676670145617,0.004,0.0030438071450436));
#34626=CARTESIAN_POINT('',(0.00396676670145617,0.004,0.0030438071450436));
#34627=CARTESIAN_POINT('',(0.00374156912278307,0.004,0.00250013209639738));
#34628=CARTESIAN_POINT('',(0.,0.004,0.));
#34629=CARTESIAN_POINT('',(0.00374165738677394,0.004,0.0025));
#34630=CARTESIAN_POINT('',(0.00433012701892219,0.004,0.0025));
#34631=CARTESIAN_POINT('',(0.00433012701892219,0.004,0.0025));
#34632=CARTESIAN_POINT('',(0.00433012701892219,0.004,0.0025));
#34633=CARTESIAN_POINT('',(0.00403589220284807,0.004,0.00199037034920393));
#34634=CARTESIAN_POINT('',(0.,0.004,0.));
#34635=CARTESIAN_POINT('',(0.00403596246968851,0.004,0.00199022786214689));
#34636=CARTESIAN_POINT('',(0.00461939766255643,0.004,0.00191341716182545));
#34637=CARTESIAN_POINT('',(0.00461939766255643,0.004,0.00191341716182545));
#34638=CARTESIAN_POINT('',(0.00461939766255643,0.004,0.00191341716182545));
#34639=CARTESIAN_POINT('',(0.00426116004836162,0.004,0.00144655281350068));
#34640=CARTESIAN_POINT('',(0.,0.004,0.));
#34641=CARTESIAN_POINT('',(0.00426121111576652,0.004,0.00144640237377705));
#34642=CARTESIAN_POINT('',(0.00482962913144534,0.004,0.0012940952255126));
#34643=CARTESIAN_POINT('',(0.00482962913144534,0.004,0.0012940952255126));
#34644=CARTESIAN_POINT('',(0.00482962913144534,0.004,0.0012940952255126));
#34645=CARTESIAN_POINT('',(0.00441351826403096,0.004,0.000877984358098221));
#34646=CARTESIAN_POINT('',(0.,0.004,0.));
#34647=CARTESIAN_POINT('',(0.00441354925822283,0.004,0.000877828539773374));
#34648=CARTESIAN_POINT('',(0.00495722430686905,0.004,0.000652630961100258));
#34649=CARTESIAN_POINT('',(0.00495722430686905,0.004,0.000652630961100258));
#34650=CARTESIAN_POINT('',(0.00495722430686905,0.004,0.000652630961100258));
#34651=CARTESIAN_POINT('',(0.00449035995854428,0.004,0.000294393346905452));
#34652=CARTESIAN_POINT('',(0.,0.004,0.));
#34653=CARTESIAN_POINT('',(0.,0.004,0.));
#34654=CARTESIAN_POINT('',(0.,0.004,0.004));
#34655=CARTESIAN_POINT('',(0.,0.004,0.));
#34656=CARTESIAN_POINT('',(0.00449037034920393,0.004,0.000294234816074125));
#34657=CARTESIAN_POINT('',(0.00449035995854428,0.004,0.000294393346905452));
#34658=CARTESIAN_POINT('',(-0.00191341716182545,0.004,-0.00461939766255643));
#34659=CARTESIAN_POINT('',(0.00495722430686905,0.004,0.000652630961100258));
#34660=CARTESIAN_POINT('',(-0.0030438071450436,0.004,0.00396676670145617));
#34661=CARTESIAN_POINT('',(0.00441354925822283,0.004,0.000877828539773374));
#34662=CARTESIAN_POINT('',(0.,0.004,0.));
#34663=CARTESIAN_POINT('',(0.00441351826403096,0.004,0.000877984358098221));
#34664=CARTESIAN_POINT('',(-0.00129409522551261,0.004,-0.00482962913144534));
#34665=CARTESIAN_POINT('',(0.00482962913144534,0.004,0.0012940952255126));
#34666=CARTESIAN_POINT('',(-0.00353553390593274,0.004,0.00353553390593274));
#34667=CARTESIAN_POINT('',(0.00426121111576652,0.004,0.00144640237377705));
#34668=CARTESIAN_POINT('',(0.,0.004,0.));
#34669=CARTESIAN_POINT('',(0.00426116004836163,0.004,0.00144655281350068));
#34670=CARTESIAN_POINT('',(-0.000652630961100263,0.004,-0.00495722430686905));
#34671=CARTESIAN_POINT('',(0.00461939766255643,0.004,0.00191341716182545));
#34672=CARTESIAN_POINT('',(-0.00396676670145617,0.004,0.0030438071450436));
#34673=CARTESIAN_POINT('',(0.00403596246968851,0.004,0.00199022786214689));
#34674=CARTESIAN_POINT('',(0.,0.004,0.));
#34675=CARTESIAN_POINT('',(0.00403589220284807,0.004,0.00199037034920393));
#34676=CARTESIAN_POINT('',(-9.18485099360482E-19,0.004,-0.005));
#34677=CARTESIAN_POINT('',(0.00433012701892219,0.004,0.0025));
#34678=CARTESIAN_POINT('',(-0.00433012701892219,0.004,0.0025));
#34679=CARTESIAN_POINT('',(0.00374165738677394,0.004,0.0025));
#34680=CARTESIAN_POINT('',(0.,0.004,0.));
#34681=CARTESIAN_POINT('',(0.00374156912278306,0.004,0.00250013209639738));
#34682=CARTESIAN_POINT('',(0.000652630961100256,0.004,-0.00495722430686905));
#34683=CARTESIAN_POINT('',(0.00396676670145617,0.004,0.0030438071450436));
#34684=CARTESIAN_POINT('',(-0.00461939766255643,0.004,0.00191341716182545));
#34685=CARTESIAN_POINT('',(0.00338333150858826,0.004,0.00296699644472216));
#34686=CARTESIAN_POINT('',(0.,0.004,0.));
#34687=CARTESIAN_POINT('',(0.00338322675766829,0.004,0.00296711589025392));
#34688=CARTESIAN_POINT('',(0.00353553390593274,0.004,0.00353553390593274));
#34689=CARTESIAN_POINT('',(0.00353553390593274,0.004,0.00353553390593274));
#34690=CARTESIAN_POINT('',(-0.00482962913144534,0.004,0.0012940952255126));
#34691=CARTESIAN_POINT('',(0.00296711589025392,0.004,0.00338322675766829));
#34692=CARTESIAN_POINT('',(0.,0.004,0.));
#34693=CARTESIAN_POINT('',(0.00296699644472216,0.004,0.00338333150858826));
#34694=CARTESIAN_POINT('',(0.0030438071450436,0.004,0.00396676670145617));
#34695=CARTESIAN_POINT('',(0.0030438071450436,0.004,0.00396676670145617));
#34696=CARTESIAN_POINT('',(-0.00495722430686905,0.004,0.00065263096110026));
#34697=CARTESIAN_POINT('',(0.00250013209639738,0.004,0.00374156912278306));
#34698=CARTESIAN_POINT('',(0.,0.004,0.));
#34699=CARTESIAN_POINT('',(0.0025,0.004,0.00374165738677394));
#34700=CARTESIAN_POINT('',(0.0025,0.004,0.00433012701892219));
#34701=CARTESIAN_POINT('',(0.0025,0.004,0.00433012701892219));
#34702=CARTESIAN_POINT('',(-0.005,0.004,6.12323399573786E-19));
#34703=CARTESIAN_POINT('',(0.00199037034920393,0.004,0.00403589220284807));
#34704=CARTESIAN_POINT('',(0.,0.004,0.));
#34705=CARTESIAN_POINT('',(0.00199022786214689,0.004,0.00403596246968851));
#34706=CARTESIAN_POINT('',(0.00191341716182545,0.004,0.00461939766255643));
#34707=CARTESIAN_POINT('',(0.00191341716182545,0.004,0.00461939766255643));
#34708=CARTESIAN_POINT('',(-0.00495722430686905,0.004,-0.000652630961100257));
#34709=CARTESIAN_POINT('',(0.00144655281350068,0.004,0.00426116004836163));
#34710=CARTESIAN_POINT('',(0.,0.004,0.));
#34711=CARTESIAN_POINT('',(0.00144640237377705,0.004,0.00426121111576652));
#34712=CARTESIAN_POINT('',(0.0012940952255126,0.004,0.00482962913144534));
#34713=CARTESIAN_POINT('',(0.0012940952255126,0.004,0.00482962913144534));
#34714=CARTESIAN_POINT('',(-0.00482962913144534,0.004,-0.0012940952255126));
#34715=CARTESIAN_POINT('',(0.000877984358098221,0.004,0.00441351826403096));
#34716=CARTESIAN_POINT('',(0.,0.004,0.));
#34717=CARTESIAN_POINT('',(0.000877828539773374,0.004,0.00441354925822283));
#34718=CARTESIAN_POINT('',(0.000652630961100259,0.004,0.00495722430686905));
#34719=CARTESIAN_POINT('',(0.000652630961100259,0.004,0.00495722430686905));
#34720=CARTESIAN_POINT('',(-0.00461939766255644,0.004,-0.00191341716182544));
#34721=CARTESIAN_POINT('',(0.000294393346905451,0.004,0.00449035995854428));
#34722=CARTESIAN_POINT('',(0.,0.004,0.));
#34723=CARTESIAN_POINT('',(0.000294234816074127,0.004,0.00449037034920393));
#34724=CARTESIAN_POINT('',(3.06161699786893E-19,0.004,0.005));
#34725=CARTESIAN_POINT('',(3.06161699786893E-19,0.004,0.005));
#34726=CARTESIAN_POINT('',(-0.00433012701892219,0.004,-0.0025));
#34727=CARTESIAN_POINT('',(-0.000294234816074129,0.004,0.00449037034920393));
#34728=CARTESIAN_POINT('',(0.,0.004,0.));
#34729=CARTESIAN_POINT('',(-0.000294393346905451,0.004,0.00449035995854428));
#34730=CARTESIAN_POINT('',(-0.000652630961100257,0.004,0.00495722430686905));
#34731=CARTESIAN_POINT('',(-0.000652630961100257,0.004,0.00495722430686905));
#34732=CARTESIAN_POINT('',(-0.00396676670145617,0.004,-0.0030438071450436));
#34733=CARTESIAN_POINT('',(-0.000877828539773375,0.004,0.00441354925822283));
#34734=CARTESIAN_POINT('',(0.,0.004,0.));
#34735=CARTESIAN_POINT('',(-0.000877984358098221,0.004,0.00441351826403096));
#34736=CARTESIAN_POINT('',(-0.0012940952255126,0.004,0.00482962913144534));
#34737=CARTESIAN_POINT('',(-0.0012940952255126,0.004,0.00482962913144534));
#34738=CARTESIAN_POINT('',(-0.0012940952255126,0.004,0.00482962913144534));
#34739=CARTESIAN_POINT('',(-0.00144640237377705,0.004,0.00426121111576652));
#34740=CARTESIAN_POINT('',(0.,0.004,0.));
#34741=CARTESIAN_POINT('',(-0.00144655281350068,0.004,0.00426116004836163));
#34742=CARTESIAN_POINT('',(-0.00191341716182545,0.004,0.00461939766255643));
#34743=CARTESIAN_POINT('',(-0.00191341716182545,0.004,0.00461939766255643));
#34744=CARTESIAN_POINT('',(-0.00191341716182545,0.004,0.00461939766255643));
#34745=CARTESIAN_POINT('',(-0.00199022786214689,0.004,0.00403596246968851));
#34746=CARTESIAN_POINT('',(0.,0.004,0.));
#34747=CARTESIAN_POINT('',(-0.00199037034920393,0.004,0.00403589220284807));
#34748=CARTESIAN_POINT('',(-0.0025,0.004,0.00433012701892219));
#34749=CARTESIAN_POINT('',(-0.0025,0.004,0.00433012701892219));
#34750=CARTESIAN_POINT('',(-0.0025,0.004,0.00433012701892219));
#34751=CARTESIAN_POINT('',(-0.0025,0.004,0.00374165738677394));
#34752=CARTESIAN_POINT('',(0.,0.004,0.));
#34753=CARTESIAN_POINT('',(-0.00250013209639738,0.004,0.00374156912278307));
#34754=CARTESIAN_POINT('',(-0.0030438071450436,0.004,0.00396676670145617));
#34755=CARTESIAN_POINT('',(-0.0030438071450436,0.004,0.00396676670145617));
#34756=CARTESIAN_POINT('',(-0.0030438071450436,0.004,0.00396676670145617));
#34757=CARTESIAN_POINT('',(-0.00296699644472215,0.004,0.00338333150858826));
#34758=CARTESIAN_POINT('',(0.,0.004,0.));
#34759=CARTESIAN_POINT('',(-0.00296711589025392,0.004,0.00338322675766829));
#34760=CARTESIAN_POINT('',(-0.00353553390593274,0.004,0.00353553390593274));
#34761=CARTESIAN_POINT('',(-0.00353553390593274,0.004,0.00353553390593274));
#34762=CARTESIAN_POINT('',(-0.00353553390593274,0.004,0.00353553390593274));
#34763=CARTESIAN_POINT('',(-0.0033832267576683,0.004,0.00296711589025391));
#34764=CARTESIAN_POINT('',(0.,0.004,0.));
#34765=CARTESIAN_POINT('',(-0.00338333150858826,0.004,0.00296699644472216));
#34766=CARTESIAN_POINT('',(-0.00396676670145617,0.004,0.0030438071450436));
#34767=CARTESIAN_POINT('',(-0.00396676670145617,0.004,0.0030438071450436));
#34768=CARTESIAN_POINT('',(-0.00396676670145617,0.004,0.0030438071450436));
#34769=CARTESIAN_POINT('',(-0.00374156912278306,0.004,0.00250013209639738));
#34770=CARTESIAN_POINT('',(0.,0.004,0.));
#34771=CARTESIAN_POINT('',(-0.00374165738677394,0.004,0.0025));
#34772=CARTESIAN_POINT('',(-0.00433012701892219,0.004,0.0025));
#34773=CARTESIAN_POINT('',(-0.00433012701892219,0.004,0.0025));
#34774=CARTESIAN_POINT('',(-0.00433012701892219,0.004,0.0025));
#34775=CARTESIAN_POINT('',(-0.00403589220284807,0.004,0.00199037034920393));
#34776=CARTESIAN_POINT('',(0.,0.004,0.));
#34777=CARTESIAN_POINT('',(-0.00403596246968851,0.004,0.00199022786214689));
#34778=CARTESIAN_POINT('',(-0.00461939766255643,0.004,0.00191341716182545));
#34779=CARTESIAN_POINT('',(-0.00461939766255643,0.004,0.00191341716182545));
#34780=CARTESIAN_POINT('',(-0.00461939766255643,0.004,0.00191341716182545));
#34781=CARTESIAN_POINT('',(-0.00426116004836163,0.004,0.00144655281350067));
#34782=CARTESIAN_POINT('',(0.,0.004,0.));
#34783=CARTESIAN_POINT('',(-0.00426121111576652,0.004,0.00144640237377705));
#34784=CARTESIAN_POINT('',(-0.00482962913144534,0.004,0.0012940952255126));
#34785=CARTESIAN_POINT('',(-0.00482962913144534,0.004,0.0012940952255126));
#34786=CARTESIAN_POINT('',(-0.00482962913144534,0.004,0.0012940952255126));
#34787=CARTESIAN_POINT('',(-0.00441351826403096,0.004,0.000877984358098221));
#34788=CARTESIAN_POINT('',(0.,0.004,0.));
#34789=CARTESIAN_POINT('',(-0.00441354925822283,0.004,0.000877828539773375));
#34790=CARTESIAN_POINT('',(-0.00495722430686905,0.004,0.00065263096110026));
#34791=CARTESIAN_POINT('',(-0.00495722430686905,0.004,0.00065263096110026));
#34792=CARTESIAN_POINT('',(-0.00495722430686905,0.004,0.00065263096110026));
#34793=CARTESIAN_POINT('',(-0.00449035995854428,0.004,0.000294393346905453));
#34794=CARTESIAN_POINT('',(0.,0.004,0.));
#34795=CARTESIAN_POINT('',(-0.00449037034920393,0.004,0.000294234816074127));
#34796=CARTESIAN_POINT('',(-0.005,0.004,6.12323399573786E-19));
#34797=CARTESIAN_POINT('',(-0.005,0.004,6.12323399573786E-19));
#34798=CARTESIAN_POINT('',(-0.005,0.004,6.12323399573786E-19));
#34799=CARTESIAN_POINT('',(-0.00449037034920393,0.004,-0.000294234816074129));
#34800=CARTESIAN_POINT('',(0.,0.004,0.));
#34801=CARTESIAN_POINT('',(-0.00449035995854428,0.004,-0.000294393346905451));
#34802=CARTESIAN_POINT('',(-0.00495722430686905,0.004,-0.000652630961100257));
#34803=CARTESIAN_POINT('',(-0.00495722430686905,0.004,-0.000652630961100257));
#34804=CARTESIAN_POINT('',(-0.00495722430686905,0.004,-0.000652630961100257));
#34805=CARTESIAN_POINT('',(-0.00441354925822283,0.004,-0.000877828539773375));
#34806=CARTESIAN_POINT('',(0.,0.004,0.));
#34807=CARTESIAN_POINT('',(-0.00441351826403096,0.004,-0.00087798435809822));
#34808=CARTESIAN_POINT('',(-0.00482962913144534,0.004,-0.0012940952255126));
#34809=CARTESIAN_POINT('',(-0.00482962913144534,0.004,-0.0012940952255126));
#34810=CARTESIAN_POINT('',(-0.00482962913144534,0.004,-0.0012940952255126));
#34811=CARTESIAN_POINT('',(-0.00426121111576652,0.004,-0.00144640237377705));
#34812=CARTESIAN_POINT('',(0.,0.004,0.));
#34813=CARTESIAN_POINT('',(-0.00426116004836163,0.004,-0.00144655281350068));
#34814=CARTESIAN_POINT('',(-0.00461939766255644,0.004,-0.00191341716182544));
#34815=CARTESIAN_POINT('',(-0.00461939766255644,0.004,-0.00191341716182544));
#34816=CARTESIAN_POINT('',(-0.00461939766255644,0.004,-0.00191341716182544));
#34817=CARTESIAN_POINT('',(-0.00403596246968851,0.004,-0.00199022786214689));
#34818=CARTESIAN_POINT('',(0.,0.004,0.));
#34819=CARTESIAN_POINT('',(-0.00403589220284807,0.004,-0.00199037034920393));
#34820=CARTESIAN_POINT('',(-0.00433012701892219,0.004,-0.0025));
#34821=CARTESIAN_POINT('',(-0.00433012701892219,0.004,-0.0025));
#34822=CARTESIAN_POINT('',(-0.00433012701892219,0.004,-0.0025));
#34823=CARTESIAN_POINT('',(-0.00374165738677394,0.004,-0.0025));
#34824=CARTESIAN_POINT('',(0.,0.004,0.));
#34825=CARTESIAN_POINT('',(-0.00374156912278307,0.004,-0.00250013209639738));
#34826=CARTESIAN_POINT('',(-0.00396676670145617,0.004,-0.0030438071450436));
#34827=CARTESIAN_POINT('',(-0.00396676670145617,0.004,-0.0030438071450436));
#34828=CARTESIAN_POINT('',(-0.00396676670145617,0.004,-0.0030438071450436));
#34829=CARTESIAN_POINT('',(-0.00338333150858826,0.004,-0.00296699644472216));
#34830=CARTESIAN_POINT('',(0.,0.004,0.));
#34831=CARTESIAN_POINT('',(-0.0033832267576683,0.004,-0.00296711589025391));
#34832=CARTESIAN_POINT('',(-0.0012940952255126,0.004,0.00482962913144534));
#34833=CARTESIAN_POINT('',(-0.00353553390593274,0.004,-0.00353553390593274));
#34834=CARTESIAN_POINT('',(-0.00353553390593274,0.004,-0.00353553390593274));
#34835=CARTESIAN_POINT('',(-0.00296711589025392,0.004,-0.00338322675766829));
#34836=CARTESIAN_POINT('',(0.,0.004,0.));
#34837=CARTESIAN_POINT('',(-0.00296699644472216,0.004,-0.00338333150858826));
#34838=CARTESIAN_POINT('',(-0.00191341716182545,0.004,0.00461939766255643));
#34839=CARTESIAN_POINT('',(-0.0030438071450436,0.004,-0.00396676670145617));
#34840=CARTESIAN_POINT('',(-0.0030438071450436,0.004,-0.00396676670145617));
#34841=CARTESIAN_POINT('',(-0.00250013209639738,0.004,-0.00374156912278306));
#34842=CARTESIAN_POINT('',(0.,0.004,0.));
#34843=CARTESIAN_POINT('',(-0.0025,0.004,-0.00374165738677394));
#34844=CARTESIAN_POINT('',(-0.0025,0.004,0.00433012701892219));
#34845=CARTESIAN_POINT('',(-0.0025,0.004,-0.00433012701892219));
#34846=CARTESIAN_POINT('',(-0.0025,0.004,-0.00433012701892219));
#34847=CARTESIAN_POINT('',(-0.00199037034920393,0.004,-0.00403589220284807));
#34848=CARTESIAN_POINT('',(0.,0.004,0.));
#34849=CARTESIAN_POINT('',(-0.0019902278621469,0.004,-0.00403596246968851));
#34850=CARTESIAN_POINT('',(-0.0030438071450436,0.004,0.00396676670145617));
#34851=CARTESIAN_POINT('',(-0.00191341716182545,0.004,-0.00461939766255643));
#34852=CARTESIAN_POINT('',(-0.00191341716182545,0.004,-0.00461939766255643));
#34853=CARTESIAN_POINT('',(-0.00144655281350068,0.004,-0.00426116004836162));
#34854=CARTESIAN_POINT('',(0.,0.004,0.));
#34855=CARTESIAN_POINT('',(-0.00144640237377705,0.004,-0.00426121111576652));
#34856=CARTESIAN_POINT('',(-0.00353553390593274,0.004,0.00353553390593274));
#34857=CARTESIAN_POINT('',(-0.00129409522551261,0.004,-0.00482962913144534));
#34858=CARTESIAN_POINT('',(-0.00129409522551261,0.004,-0.00482962913144534));
#34859=CARTESIAN_POINT('',(-0.000877984358098222,0.004,-0.00441351826403096));
#34860=CARTESIAN_POINT('',(0.,0.004,0.));
#34861=CARTESIAN_POINT('',(-0.000877828539773377,0.004,-0.00441354925822283));
#34862=CARTESIAN_POINT('',(-0.00396676670145617,0.004,0.0030438071450436));
#34863=CARTESIAN_POINT('',(-0.000652630961100263,0.004,-0.00495722430686905));
#34864=CARTESIAN_POINT('',(-0.000652630961100263,0.004,-0.00495722430686905));
#34865=CARTESIAN_POINT('',(-0.000294393346905453,0.004,-0.00449035995854428));
#34866=CARTESIAN_POINT('',(0.,0.004,0.));
#34867=CARTESIAN_POINT('',(-0.000294234816074127,0.004,-0.00449037034920393));
#34868=CARTESIAN_POINT('',(-0.00433012701892219,0.004,0.0025));
#34869=CARTESIAN_POINT('',(-9.18485099360482E-19,0.004,-0.005));
#34870=CARTESIAN_POINT('',(-9.18485099360482E-19,0.004,-0.005));
#34871=CARTESIAN_POINT('',(0.000294234816074127,0.004,-0.00449037034920393));
#34872=CARTESIAN_POINT('',(0.,0.004,0.));
#34873=CARTESIAN_POINT('',(0.000294393346905451,0.004,-0.00449035995854428));
#34874=CARTESIAN_POINT('',(-0.00461939766255643,0.004,0.00191341716182545));
#34875=CARTESIAN_POINT('',(0.000652630961100256,0.004,-0.00495722430686905));
#34876=CARTESIAN_POINT('',(0.000652630961100256,0.004,-0.00495722430686905));
#34877=CARTESIAN_POINT('',(0.000877828539773373,0.004,-0.00441354925822283));
#34878=CARTESIAN_POINT('',(0.,0.004,0.));
#34879=CARTESIAN_POINT('',(0.000877984358098219,0.004,-0.00441351826403096));
#34880=CARTESIAN_POINT('',(-0.00482962913144534,0.004,0.0012940952255126));
#34881=CARTESIAN_POINT('',(0.0012940952255126,0.004,-0.00482962913144534));
#34882=CARTESIAN_POINT('',(0.00353553390593274,0.004,0.00353553390593274));
#34883=CARTESIAN_POINT('',(0.00144640237377704,0.004,-0.00426121111576652));
#34884=CARTESIAN_POINT('',(0.,0.004,0.));
#34885=CARTESIAN_POINT('',(0.00144655281350068,0.004,-0.00426116004836163));
#34886=CARTESIAN_POINT('',(-0.00495722430686905,0.004,0.00065263096110026));
#34887=CARTESIAN_POINT('',(0.00191341716182544,0.004,-0.00461939766255644));
#34888=CARTESIAN_POINT('',(0.0030438071450436,0.004,0.00396676670145617));
#34889=CARTESIAN_POINT('',(0.00199022786214689,0.004,-0.00403596246968851));
#34890=CARTESIAN_POINT('',(0.,0.004,0.));
#34891=CARTESIAN_POINT('',(0.00199037034920392,0.004,-0.00403589220284807));
#34892=CARTESIAN_POINT('',(-0.005,0.004,6.12323399573786E-19));
#34893=CARTESIAN_POINT('',(0.0025,0.004,-0.00433012701892219));
#34894=CARTESIAN_POINT('',(0.0025,0.004,0.00433012701892219));
#34895=CARTESIAN_POINT('',(0.0025,0.004,-0.00374165738677394));
#34896=CARTESIAN_POINT('',(0.,0.004,0.));
#34897=CARTESIAN_POINT('',(0.00250013209639738,0.004,-0.00374156912278307));
#34898=CARTESIAN_POINT('',(-0.00495722430686905,0.004,-0.000652630961100257));
#34899=CARTESIAN_POINT('',(0.0030438071450436,0.004,-0.00396676670145618));
#34900=CARTESIAN_POINT('',(0.00191341716182545,0.004,0.00461939766255643));
#34901=CARTESIAN_POINT('',(0.00296699644472215,0.004,-0.00338333150858826));
#34902=CARTESIAN_POINT('',(0.,0.004,0.));
#34903=CARTESIAN_POINT('',(0.00296711589025392,0.004,-0.00338322675766829));
#34904=CARTESIAN_POINT('',(-0.00482962913144534,0.004,-0.0012940952255126));
#34905=CARTESIAN_POINT('',(0.00353553390593274,0.004,-0.00353553390593274));
#34906=CARTESIAN_POINT('',(0.0012940952255126,0.004,0.00482962913144534));
#34907=CARTESIAN_POINT('',(0.00338322675766829,0.004,-0.00296711589025392));
#34908=CARTESIAN_POINT('',(0.,0.004,0.));
#34909=CARTESIAN_POINT('',(0.00338333150858826,0.004,-0.00296699644472216));
#34910=CARTESIAN_POINT('',(-0.00461939766255644,0.004,-0.00191341716182544));
#34911=CARTESIAN_POINT('',(0.00396676670145617,0.004,-0.0030438071450436));
#34912=CARTESIAN_POINT('',(0.00396676670145617,0.004,-0.0030438071450436));
#34913=CARTESIAN_POINT('',(0.00374165738677394,0.004,-0.0025));
#34914=CARTESIAN_POINT('',(-0.00433012701892219,0.004,-0.0025));
#34915=CARTESIAN_POINT('',(0.00433012701892219,0.004,-0.0025));
#34916=CARTESIAN_POINT('',(3.06161699786893E-19,0.004,0.005));
#34917=CARTESIAN_POINT('',(0.00403589220284806,0.004,-0.00199037034920393));
#34918=CARTESIAN_POINT('',(0.,0.004,0.));
#34919=CARTESIAN_POINT('',(0.00403596246968851,0.004,-0.0019902278621469));
#34920=CARTESIAN_POINT('',(-0.00396676670145617,0.004,-0.0030438071450436));
#34921=CARTESIAN_POINT('',(0.00461939766255643,0.004,-0.00191341716182545));
#34922=CARTESIAN_POINT('',(-0.000652630961100257,0.004,0.00495722430686905));
#34923=CARTESIAN_POINT('',(0.00426116004836162,0.004,-0.00144655281350068));
#34924=CARTESIAN_POINT('',(0.,0.004,0.));
#34925=CARTESIAN_POINT('',(0.00426121111576652,0.004,-0.00144640237377705));
#34926=CARTESIAN_POINT('',(-0.00353553390593274,0.004,-0.00353553390593274));
#34927=CARTESIAN_POINT('',(0.00482962913144534,0.004,-0.00129409522551261));
#34928=CARTESIAN_POINT('',(-0.0012940952255126,0.004,0.00482962913144534));
#34929=CARTESIAN_POINT('',(0.00441351826403096,0.004,-0.000877984358098224));
#34930=CARTESIAN_POINT('',(0.,0.004,0.));
#34931=CARTESIAN_POINT('',(0.00441354925822283,0.004,-0.000877828539773378));
#34932=CARTESIAN_POINT('',(-0.0030438071450436,0.004,-0.00396676670145617));
#34933=CARTESIAN_POINT('',(0.00495722430686905,0.004,-0.000652630961100263));
#34934=CARTESIAN_POINT('',(-0.00191341716182545,0.004,0.00461939766255643));
#34935=CARTESIAN_POINT('',(0.00449035995854428,0.004,-0.000294393346905455));
#34936=CARTESIAN_POINT('',(0.,0.004,0.));
#34937=CARTESIAN_POINT('',(0.00449037034920393,0.004,-0.000294234816074128));
#34938=CARTESIAN_POINT('',(-0.0025,0.004,-0.00433012701892219));
#34939=CARTESIAN_POINT('',(0.005,0.004,0.));
#34940=CARTESIAN_POINT('',(-0.0025,0.004,0.00433012701892219));
#34941=CARTESIAN_POINT('',(0.,0.006,0.));
#34942=CARTESIAN_POINT('',(0.,0.006,0.));
#34943=CARTESIAN_POINT('',(0.,0.006,0.));
#34944=CARTESIAN_POINT('',(0.,0.006,0.004));
#34945=CARTESIAN_POINT('',(0.,0.012,0.));
#34946=CARTESIAN_POINT('',(0.,0.006,0.));
#34947=CARTESIAN_POINT('',(0.,0.001,0.));
#34948=CARTESIAN_POINT('',(0.,3.17541634481466E-5,0.));
#34949=CARTESIAN_POINT('',(0.,3.17541634481466E-5,0.00025));
#34950=CARTESIAN_POINT('',(0.,0.022,0.));
#34951=CARTESIAN_POINT('',(0.,0.011,0.));
#34952=CARTESIAN_POINT('',(0.,0.011,0.001));
#34953=CARTESIAN_POINT('',(0.,0.011,0.));
#34954=CARTESIAN_POINT('',(0.,3.17541634481466E-5,0.));
#34955=CARTESIAN_POINT('',(0.,0.,0.107));
#34956=CARTESIAN_POINT('',(0.,0.,-0.0620923697749146));
#34957=CARTESIAN_POINT('',(0.,0.,-0.0620923697749146));
#34958=CARTESIAN_POINT('',(-0.00325,0.,-0.0620923697749146));
#34959=CARTESIAN_POINT('',(0.,0.,-0.0620923697749146));
#34960=CARTESIAN_POINT('',(-0.00375,0.,-0.0620923697749146));
#34961=CARTESIAN_POINT('',(0.,0.,-0.0234923697749146));
#34962=CARTESIAN_POINT('',(0.,0.,-0.0234923697749146));
#34963=CARTESIAN_POINT('',(-0.00375,0.,-0.0234923697749146));
#34964=CARTESIAN_POINT('',(0.,0.,-0.0234923697749146));
#34965=CARTESIAN_POINT('',(-0.00325,0.,-0.0234923697749146));
#34966=CARTESIAN_POINT('',(0.,0.,-0.0234923697749146));
#34967=CARTESIAN_POINT('',(0.,0.,-0.0234923697749146));
#34968=CARTESIAN_POINT('',(-2.09094396436286E-18,-3.13451728873585E-18,
0.023807215148666));
#34969=CARTESIAN_POINT('',(0.,0.,0.046));
#34970=CARTESIAN_POINT('',(0.,0.,0.046));
#34971=CARTESIAN_POINT('',(0.0123,0.,0.046));
#34972=CARTESIAN_POINT('',(0.,0.,0.046));
#34973=CARTESIAN_POINT('',(0.0188,0.,0.046));
#34974=CARTESIAN_POINT('',(0.,0.,0.0469));
#34975=CARTESIAN_POINT('',(0.,0.,0.0469));
#34976=CARTESIAN_POINT('',(0.0123,0.,0.0469));
#34977=CARTESIAN_POINT('',(0.,0.,0.0469));
#34978=CARTESIAN_POINT('',(0.0188,0.,0.0469));
#34979=CARTESIAN_POINT('',(0.,0.,0.0469));
#34980=CARTESIAN_POINT('',(0.,0.,0.0469));
#34981=CARTESIAN_POINT('',(0.,0.,0.));
#34982=CARTESIAN_POINT('',(-0.025980762113538,-0.0149999999999972,0.11392908368361));
#34983=CARTESIAN_POINT('',(-0.012852081728299,0.0305608891324553,0.026));
#34984=CARTESIAN_POINT('',(-0.014204163456598,0.0308108891324553,0.026));
#34985=CARTESIAN_POINT('',(-0.0146732429566961,0.0308976219627052,0.026));
#34986=CARTESIAN_POINT('',(-0.0137350839565,0.0307241563022055,0.026));
#34987=CARTESIAN_POINT('',(-0.0115,0.0303108891324553,0.026));
#34988=CARTESIAN_POINT('',(-0.0146732429566961,0.0297241563022054,0.026));
#34989=CARTESIAN_POINT('',(-0.014204163456598,0.0298108891324554,0.026));
#34990=CARTESIAN_POINT('',(-0.0137350839565,0.0298976219627052,0.026));
#34991=CARTESIAN_POINT('',(-0.0115,0.0303108891324553,0.026));
#34992=CARTESIAN_POINT('',(-0.014204163456598,0.0298108891324554,0.026));
#34993=CARTESIAN_POINT('',(-0.014204163456598,0.0298108891324554,0.021));
#34994=CARTESIAN_POINT('',(-0.0137350839565,0.0298976219627052,0.021));
#34995=CARTESIAN_POINT('',(-0.0146732429566961,0.0297241563022054,0.021));
#34996=CARTESIAN_POINT('',(-0.0137350839565,0.0298976219627052,0.026));
#34997=CARTESIAN_POINT('',(-0.0146732429566961,0.0297241563022054,0.026));
#34998=CARTESIAN_POINT('',(-0.014204163456598,0.0308108891324553,0.026));
#34999=CARTESIAN_POINT('',(-0.014204163456598,0.0308108891324553,0.021));
#35000=CARTESIAN_POINT('',(-0.0146732429566961,0.0308976219627052,0.021));
#35001=CARTESIAN_POINT('',(-0.0137350839565,0.0307241563022055,0.021));
#35002=CARTESIAN_POINT('',(-0.0146732429566961,0.0308976219627052,0.026));
#35003=CARTESIAN_POINT('',(-0.0137350839565,0.0307241563022055,0.026));
#35004=CARTESIAN_POINT('',(-0.012852081728299,0.0305608891324553,0.026));
#35005=CARTESIAN_POINT('',(-0.00879583654340205,0.0308108891324553,0.026));
#35006=CARTESIAN_POINT('',(-0.0092649160435001,0.0307241563022055,0.026));
#35007=CARTESIAN_POINT('',(-0.008326757043304,0.0308976219627052,0.026));
#35008=CARTESIAN_POINT('',(-0.0115,0.0303108891324553,0.026));
#35009=CARTESIAN_POINT('',(-0.0092649160435001,0.0298976219627052,0.026));
#35010=CARTESIAN_POINT('',(-0.00879583654340205,0.0298108891324554,0.026));
#35011=CARTESIAN_POINT('',(-0.00832675704330399,0.0297241563022054,0.026));
#35012=CARTESIAN_POINT('',(-0.0115,0.0303108891324553,0.026));
#35013=CARTESIAN_POINT('',(-0.0115,0.0303108891324553,0.026));
#35014=CARTESIAN_POINT('',(-0.0115,0.0303108891324553,0.021));
#35015=CARTESIAN_POINT('',(-0.00832675704330399,0.0308976219627052,0.021));
#35016=CARTESIAN_POINT('',(-0.008326757043304,0.0297241563022054,0.021));
#35017=CARTESIAN_POINT('',(-0.008326757043304,0.0308976219627052,0.026));
#35018=CARTESIAN_POINT('',(-0.008326757043304,0.0297241563022054,0.026));
#35019=CARTESIAN_POINT('',(-0.0115,0.0303108891324553,0.026));
#35020=CARTESIAN_POINT('',(-0.0115,0.0303108891324553,0.021));
#35021=CARTESIAN_POINT('',(-0.0092649160435001,0.0298976219627052,0.021));
#35022=CARTESIAN_POINT('',(-0.0092649160435001,0.0307241563022055,0.021));
#35023=CARTESIAN_POINT('',(-0.0092649160435001,0.0298976219627052,0.026));
#35024=CARTESIAN_POINT('',(-0.0092649160435001,0.0307241563022055,0.026));
#35025=CARTESIAN_POINT('',(-0.0115,0.0303108891324553,0.018));
#35026=CARTESIAN_POINT('',(-0.0115,0.0303108891324553,0.018));
#35027=CARTESIAN_POINT('',(-0.015,0.0303108891324553,0.018));
#35028=CARTESIAN_POINT('',(0.,0.,0.025));
#35029=CARTESIAN_POINT('',(-0.0115,0.0303108891324553,0.025));
#35030=CARTESIAN_POINT('',(-0.0125,0.0303108891324553,0.025));
#35031=CARTESIAN_POINT('',(-0.0115,0.0303108891324553,0.021));
#35032=CARTESIAN_POINT('',(-0.0115,0.0303108891324553,0.021));
#35033=CARTESIAN_POINT('',(-0.0115,0.0303108891324553,0.021));
#35034=CARTESIAN_POINT('',(-0.0115,0.0303108891324553,0.021));
#35035=CARTESIAN_POINT('',(-0.015,0.0303108891324553,0.021));
#35036=CARTESIAN_POINT('',(-0.0115,0.0303108891324553,0.021));
#35037=CARTESIAN_POINT('',(-0.0125,0.0303108891324553,0.021));
#35038=CARTESIAN_POINT('',(-0.00879583654340205,0.0308108891324553,0.021));
#35039=CARTESIAN_POINT('',(-0.00879583654340205,0.0298108891324554,0.021));
#35040=CARTESIAN_POINT('',(-0.0115,0.0303108891324553,0.025));
#35041=CARTESIAN_POINT('',(-0.0115,0.0303108891324553,0.018));
#35042=CARTESIAN_POINT('',(-0.00879583654340205,0.0308108891324553,0.026));
#35043=CARTESIAN_POINT('',(-0.00879583654340205,0.0298108891324554,0.026));
#35044=CARTESIAN_POINT('',(-0.0115,0.0303108891324553,0.026));
#35045=CARTESIAN_POINT('',(-0.0115,0.0303108891324553,0.026));
#35046=CARTESIAN_POINT('',(-0.00427548757800061,-0.0020945466955101,4.21297175334708E-35));
#35047=CARTESIAN_POINT('',(0.,0.,0.));
#35048=CARTESIAN_POINT('',(9.18485099360515E-20,0.0015,0.));
#35049=CARTESIAN_POINT('',(6.37211816187961E-19,-1.8047270239716E-18,0.0933179000348155));
#35050=CARTESIAN_POINT('',(0.00350000000000028,-0.037,0.092));
#35051=CARTESIAN_POINT('',(0.00350000000000028,-0.037,0.092));
#35052=CARTESIAN_POINT('',(0.00350000000000027,-0.037,0.1));
#35053=CARTESIAN_POINT('',(0.00350000000000027,-0.037,0.103));
#35054=CARTESIAN_POINT('',(0.00350000000000028,-0.037,0.103));
#35055=CARTESIAN_POINT('',(-0.00349999999999974,-0.037,0.103));
#35056=CARTESIAN_POINT('',(-0.00349999999999974,-0.037,0.092));
#35057=CARTESIAN_POINT('',(-0.00349999999999974,-0.037,0.1));
#35058=CARTESIAN_POINT('',(2.69062550017907E-16,-0.037,0.1));
#35059=CARTESIAN_POINT('',(-0.00349999999999973,-0.038,0.092));
#35060=CARTESIAN_POINT('',(-0.00349999999999973,-0.038,0.103));
#35061=CARTESIAN_POINT('',(-0.00349999999999972,-0.039,0.103));
#35062=CARTESIAN_POINT('',(-0.00349999999999972,-0.039,0.092));
#35063=CARTESIAN_POINT('',(-0.00349999999999972,-0.039,0.1));
#35064=CARTESIAN_POINT('',(-0.00349999999999973,-0.038,0.1));
#35065=CARTESIAN_POINT('',(0.00350000000000029,-0.039,0.092));
#35066=CARTESIAN_POINT('',(0.00350000000000029,-0.039,0.103));
#35067=CARTESIAN_POINT('',(0.00350000000000029,-0.039,0.103));
#35068=CARTESIAN_POINT('',(0.00350000000000029,-0.039,0.092));
#35069=CARTESIAN_POINT('',(0.00350000000000029,-0.039,0.1));
#35070=CARTESIAN_POINT('',(2.9876101592663E-16,-0.039,0.1));
#35071=CARTESIAN_POINT('',(0.030292939940024,0.0215310889132459,0.092));
#35072=CARTESIAN_POINT('',(0.030292939940024,0.0215310889132459,0.092));
#35073=CARTESIAN_POINT('',(0.030292939940024,0.0215310889132459,0.1));
#35074=CARTESIAN_POINT('',(0.030292939940024,0.0215310889132459,0.103));
#35075=CARTESIAN_POINT('',(0.030292939940024,0.0215310889132459,0.103));
#35076=CARTESIAN_POINT('',(0.033792939940024,0.0154689110867548,0.103));
#35077=CARTESIAN_POINT('',(0.033792939940024,0.0154689110867548,0.092));
#35078=CARTESIAN_POINT('',(0.033792939940024,0.0154689110867548,0.1));
#35079=CARTESIAN_POINT('',(0.032042939940024,0.0185000000000004,0.1));
#35080=CARTESIAN_POINT('',(0.0320249907475929,0.0225310889132459,0.092));
#35081=CARTESIAN_POINT('',(0.0355249907475929,0.0164689110867549,0.092));
#35082=CARTESIAN_POINT('',(0.0355249907475929,0.0164689110867549,0.1));
#35083=CARTESIAN_POINT('',(0.0355249907475929,0.0164689110867549,0.103));
#35084=CARTESIAN_POINT('',(0.0320249907475929,0.0225310889132459,0.103));
#35085=CARTESIAN_POINT('',(0.0320249907475929,0.0225310889132459,0.103));
#35086=CARTESIAN_POINT('',(0.0320249907475929,0.0225310889132459,0.092));
#35087=CARTESIAN_POINT('',(0.0320249907475929,0.0225310889132459,0.1));
#35088=CARTESIAN_POINT('',(0.0337749907475929,0.0195000000000004,0.1));
#35089=CARTESIAN_POINT('',(0.0311589653438084,0.0220310889132459,0.092));
#35090=CARTESIAN_POINT('',(0.0311589653438084,0.0220310889132459,0.103));
#35091=CARTESIAN_POINT('',(0.0311589653438084,0.0220310889132459,0.1));
#35092=CARTESIAN_POINT('',(-0.0337929399400243,0.0154689110867544,0.092));
#35093=CARTESIAN_POINT('',(-0.0337929399400243,0.0154689110867544,0.092));
#35094=CARTESIAN_POINT('',(-0.0337929399400243,0.0154689110867544,0.1));
#35095=CARTESIAN_POINT('',(-0.0337929399400243,0.0154689110867544,0.103));
#35096=CARTESIAN_POINT('',(-0.0337929399400243,0.0154689110867544,0.103));
#35097=CARTESIAN_POINT('',(-0.0302929399400243,0.0215310889132454,0.103));
#35098=CARTESIAN_POINT('',(-0.0302929399400243,0.0215310889132454,0.092));
#35099=CARTESIAN_POINT('',(-0.0302929399400243,0.0215310889132454,0.1));
#35100=CARTESIAN_POINT('',(-0.0320429399400243,0.0185,0.1));
#35101=CARTESIAN_POINT('',(-0.0355249907475932,0.0164689110867543,0.092));
#35102=CARTESIAN_POINT('',(-0.0320249907475932,0.0225310889132454,0.092));
#35103=CARTESIAN_POINT('',(-0.0320249907475932,0.0225310889132454,0.1));
#35104=CARTESIAN_POINT('',(-0.0320249907475932,0.0225310889132454,0.103));
#35105=CARTESIAN_POINT('',(-0.0355249907475932,0.0164689110867543,0.103));
#35106=CARTESIAN_POINT('',(-0.0355249907475932,0.0164689110867543,0.103));
#35107=CARTESIAN_POINT('',(-0.0355249907475932,0.0164689110867543,0.092));
#35108=CARTESIAN_POINT('',(-0.0355249907475932,0.0164689110867543,0.1));
#35109=CARTESIAN_POINT('',(-0.0337749907475932,0.0195,0.1));
#35110=CARTESIAN_POINT('',(-0.0346589653438087,0.0159689110867543,0.092));
#35111=CARTESIAN_POINT('',(-0.0346589653438087,0.0159689110867543,0.103));
#35112=CARTESIAN_POINT('',(-0.0346589653438087,0.0159689110867543,0.1));
#35113=CARTESIAN_POINT('',(-0.024761562113538,-0.0149999999999972,0.10173));
#35114=CARTESIAN_POINT('',(0.,0.03,0.10173));
#35115=CARTESIAN_POINT('',(0.00277876,0.03,0.10173));
#35116=CARTESIAN_POINT('',(0.,0.03,0.10173));
#35117=CARTESIAN_POINT('',(0.0012192,0.03,0.10173));
#35118=CARTESIAN_POINT('',(-0.024761562113538,-0.0149999999999972,0.10173));
#35119=CARTESIAN_POINT('',(-0.025980762113538,-0.0149999999999972,0.10173));
#35120=CARTESIAN_POINT('',(-0.023202002113538,-0.0149999999999972,0.10173));
#35121=CARTESIAN_POINT('',(-0.025980762113538,-0.0149999999999972,0.10173));
#35122=CARTESIAN_POINT('',(-0.024761562113538,-0.0149999999999972,0.10173));
#35123=CARTESIAN_POINT('',(-0.024761562113538,-0.0149999999999972,0.10173));
#35124=CARTESIAN_POINT('',(0.0259807621135283,-0.0150000000000028,0.10173));
#35125=CARTESIAN_POINT('',(0.0287595221135283,-0.0150000000000028,0.10173));
#35126=CARTESIAN_POINT('',(0.0259807621135283,-0.0150000000000028,0.10173));
#35127=CARTESIAN_POINT('',(0.0271999621135283,-0.0150000000000028,0.10173));
#35128=CARTESIAN_POINT('',(0.,0.,0.103));
#35129=CARTESIAN_POINT('',(0.0259807621135283,-0.0150000000000028,0.103));
#35130=CARTESIAN_POINT('',(0.0287595221135283,-0.0150000000000028,0.103));
#35131=CARTESIAN_POINT('',(-0.025980762113538,-0.0149999999999972,0.103));
#35132=CARTESIAN_POINT('',(-0.023202002113538,-0.0149999999999972,0.103));
#35133=CARTESIAN_POINT('',(0.,0.03,0.103));
#35134=CARTESIAN_POINT('',(0.00277876,0.03,0.103));
#35135=CARTESIAN_POINT('',(-0.0311589653438087,0.0220310889132454,0.103));
#35136=CARTESIAN_POINT('',(0.0346589653438085,0.0159689110867548,0.103));
#35137=CARTESIAN_POINT('',(0.00350000000000028,-0.038,0.103));
#35138=CARTESIAN_POINT('',(0.,0.,0.103));
#35139=CARTESIAN_POINT('',(0.0104331778036387,0.,0.103));
#35140=CARTESIAN_POINT('',(0.,0.,0.103));
#35141=CARTESIAN_POINT('',(0.044,0.,0.103));
#35142=CARTESIAN_POINT('',(0.,0.,0.1));
#35143=CARTESIAN_POINT('',(0.0259807621135283,-0.0150000000000028,0.1));
#35144=CARTESIAN_POINT('',(0.0271999621135283,-0.0150000000000028,0.1));
#35145=CARTESIAN_POINT('',(-0.025980762113538,-0.0149999999999972,0.1));
#35146=CARTESIAN_POINT('',(-0.024761562113538,-0.0149999999999972,0.1));
#35147=CARTESIAN_POINT('',(0.,0.03,0.1));
#35148=CARTESIAN_POINT('',(0.0012192,0.03,0.1));
#35149=CARTESIAN_POINT('',(-0.0311589653438087,0.0220310889132454,0.1));
#35150=CARTESIAN_POINT('',(0.0346589653438085,0.0159689110867548,0.1));
#35151=CARTESIAN_POINT('',(0.00350000000000028,-0.038,0.1));
#35152=CARTESIAN_POINT('',(0.,0.,0.1));
#35153=CARTESIAN_POINT('',(0.044,0.,0.1));
#35154=CARTESIAN_POINT('',(0.,0.,0.1));
#35155=CARTESIAN_POINT('',(0.0104331778036387,0.,0.1));
#35156=CARTESIAN_POINT('',(0.,0.,0.1));
#35157=CARTESIAN_POINT('',(0.,0.,0.102));
#35158=CARTESIAN_POINT('',(0.045,0.,0.102));
#35159=CARTESIAN_POINT('',(0.,0.,0.101));
#35160=CARTESIAN_POINT('',(0.045,0.,0.101));
#35161=CARTESIAN_POINT('',(0.,0.,0.083));
#35162=CARTESIAN_POINT('',(0.,0.,0.102));
#35163=CARTESIAN_POINT('',(0.00943317780363869,0.,0.102));
#35164=CARTESIAN_POINT('',(0.,0.,0.101));
#35165=CARTESIAN_POINT('',(0.00943317780363869,0.,0.101));
#35166=CARTESIAN_POINT('',(0.0259807621135283,-0.0150000000000028,0.103));
#35167=CARTESIAN_POINT('',(0.0259807621135283,-0.0150000000000028,0.103));
#35168=CARTESIAN_POINT('',(-0.025980762113538,-0.0149999999999972,0.103));
#35169=CARTESIAN_POINT('',(-0.025980762113538,-0.0149999999999972,0.103));
#35170=CARTESIAN_POINT('',(0.,0.03,0.103));
#35171=CARTESIAN_POINT('',(0.,0.03,0.103));
#35172=CARTESIAN_POINT('',(-0.0311589653438087,0.0220310889132454,0.092));
#35173=CARTESIAN_POINT('',(0.0346589653438085,0.0159689110867548,0.092));
#35174=CARTESIAN_POINT('',(0.00350000000000028,-0.038,0.092));
#35175=CARTESIAN_POINT('',(0.,0.,0.101));
#35176=CARTESIAN_POINT('',(0.,0.,0.101));
#35177=CARTESIAN_POINT('',(0.,0.,0.102));
#35178=CARTESIAN_POINT('',(0.,0.,0.102));
#35179=CARTESIAN_POINT('',(0.,0.,0.0107004836836099));
#35180=CARTESIAN_POINT('',(0.,0.,-0.0245189377942895));
#35181=CARTESIAN_POINT('',(-1.53080849893419E-19,0.0025,-0.0245189377942895));
#35182=CARTESIAN_POINT('',(8.11448407488054E-18,2.50982061068968E-18,0.0288076302250854));
#35183=CARTESIAN_POINT('',(4.23272528138341E-16,-0.043,0.083));
#35184=CARTESIAN_POINT('',(0.0429027729595412,0.00977187011365056,0.0107004836836099));
#35185=CARTESIAN_POINT('',(0.,0.,0.1));
#35186=CARTESIAN_POINT('',(0.0311589653438084,0.0220310889132459,0.1));
#35187=CARTESIAN_POINT('',(0.030292939940024,0.0215310889132459,0.1));
#35188=CARTESIAN_POINT('',(0.0320249907475929,0.0225310889132459,0.1));
#35189=CARTESIAN_POINT('',(0.0320249907475929,0.0225310889132459,0.1));
#35190=CARTESIAN_POINT('',(0.0355249907475929,0.0164689110867549,0.1));
#35191=CARTESIAN_POINT('',(0.0346589653438085,0.0159689110867548,0.1));
#35192=CARTESIAN_POINT('',(0.033792939940024,0.0154689110867548,0.1));
#35193=CARTESIAN_POINT('',(0.030292939940024,0.0215310889132459,0.1));
#35194=CARTESIAN_POINT('',(0.030292939940024,0.0215310889132459,0.0902404553740472));
#35195=CARTESIAN_POINT('',(0.033792939940024,0.0154689110867548,0.0902404553740472));
#35196=CARTESIAN_POINT('',(0.033792939940024,0.0154689110867548,0.103));
#35197=CARTESIAN_POINT('',(0.030292939940024,0.0215310889132459,0.103));
#35198=CARTESIAN_POINT('',(0.030292939940024,0.0215310889132459,0.103));
#35199=CARTESIAN_POINT('',(0.030292939940024,0.0215310889132459,0.0902404553740472));
#35200=CARTESIAN_POINT('',(0.0320249907475929,0.0225310889132459,0.0902404553740472));
#35201=CARTESIAN_POINT('',(0.0320249907475929,0.0225310889132459,0.0902404553740472));
#35202=CARTESIAN_POINT('',(0.0320249907475929,0.0225310889132459,0.103));
#35203=CARTESIAN_POINT('',(0.0320249907475929,0.0225310889132459,0.103));
#35204=CARTESIAN_POINT('',(0.0355249907475929,0.0164689110867549,0.103));
#35205=CARTESIAN_POINT('',(0.0355249907475929,0.0164689110867549,0.0902404553740472));
#35206=CARTESIAN_POINT('',(0.0311589653438084,0.0220310889132459,0.0902404553740472));
#35207=CARTESIAN_POINT('',(0.0311589653438084,0.0220310889132459,0.103));
#35208=CARTESIAN_POINT('',(0.,0.,0.1));
#35209=CARTESIAN_POINT('',(0.00350000000000028,-0.038,0.1));
#35210=CARTESIAN_POINT('',(0.00350000000000027,-0.037,0.1));
#35211=CARTESIAN_POINT('',(0.00350000000000029,-0.039,0.1));
#35212=CARTESIAN_POINT('',(0.00350000000000029,-0.039,0.1));
#35213=CARTESIAN_POINT('',(-0.00349999999999972,-0.039,0.1));
#35214=CARTESIAN_POINT('',(-0.00349999999999973,-0.038,0.1));
#35215=CARTESIAN_POINT('',(-0.00349999999999974,-0.037,0.1));
#35216=CARTESIAN_POINT('',(0.00350000000000028,-0.037,0.1));
#35217=CARTESIAN_POINT('',(0.00350000000000028,-0.037,0.0902404553740472));
#35218=CARTESIAN_POINT('',(-0.00349999999999974,-0.037,0.0902404553740472));
#35219=CARTESIAN_POINT('',(-0.00349999999999974,-0.037,0.103));
#35220=CARTESIAN_POINT('',(0.00350000000000028,-0.037,0.103));
#35221=CARTESIAN_POINT('',(0.00350000000000027,-0.037,0.103));
#35222=CARTESIAN_POINT('',(0.00350000000000028,-0.037,0.0902404553740472));
#35223=CARTESIAN_POINT('',(0.00350000000000029,-0.039,0.0902404553740472));
#35224=CARTESIAN_POINT('',(0.00350000000000029,-0.039,0.0902404553740472));
#35225=CARTESIAN_POINT('',(0.00350000000000029,-0.039,0.103));
#35226=CARTESIAN_POINT('',(0.00350000000000029,-0.039,0.103));
#35227=CARTESIAN_POINT('',(-0.00349999999999972,-0.039,0.103));
#35228=CARTESIAN_POINT('',(-0.00349999999999972,-0.039,0.0902404553740472));
#35229=CARTESIAN_POINT('',(0.00350000000000028,-0.038,0.0902404553740472));
#35230=CARTESIAN_POINT('',(0.00350000000000028,-0.038,0.103));
#35231=CARTESIAN_POINT('',(0.,0.,0.1));
#35232=CARTESIAN_POINT('',(-0.0346589653438087,0.0159689110867543,0.1));
#35233=CARTESIAN_POINT('',(-0.0337929399400243,0.0154689110867544,0.1));
#35234=CARTESIAN_POINT('',(-0.0355249907475932,0.0164689110867543,0.1));
#35235=CARTESIAN_POINT('',(-0.0355249907475932,0.0164689110867543,0.1));
#35236=CARTESIAN_POINT('',(-0.0320249907475932,0.0225310889132454,0.1));
#35237=CARTESIAN_POINT('',(-0.0311589653438087,0.0220310889132454,0.1));
#35238=CARTESIAN_POINT('',(-0.0302929399400243,0.0215310889132454,0.1));
#35239=CARTESIAN_POINT('',(-0.0337929399400243,0.0154689110867544,0.1));
#35240=CARTESIAN_POINT('',(-0.0337929399400243,0.0154689110867544,0.0902404553740472));
#35241=CARTESIAN_POINT('',(-0.0302929399400243,0.0215310889132454,0.0902404553740472));
#35242=CARTESIAN_POINT('',(-0.0302929399400243,0.0215310889132454,0.103));
#35243=CARTESIAN_POINT('',(-0.0337929399400243,0.0154689110867544,0.103));
#35244=CARTESIAN_POINT('',(-0.0337929399400243,0.0154689110867544,0.103));
#35245=CARTESIAN_POINT('',(-0.0337929399400243,0.0154689110867544,0.0902404553740472));
#35246=CARTESIAN_POINT('',(-0.0355249907475932,0.0164689110867543,0.0902404553740472));
#35247=CARTESIAN_POINT('',(-0.0355249907475932,0.0164689110867543,0.0902404553740472));
#35248=CARTESIAN_POINT('',(-0.0355249907475932,0.0164689110867543,0.103));
#35249=CARTESIAN_POINT('',(-0.0355249907475932,0.0164689110867543,0.103));
#35250=CARTESIAN_POINT('',(-0.0320249907475932,0.0225310889132454,0.103));
#35251=CARTESIAN_POINT('',(-0.0320249907475932,0.0225310889132454,0.0902404553740472));
#35252=CARTESIAN_POINT('',(-0.0346589653438087,0.0159689110867543,0.0902404553740472));
#35253=CARTESIAN_POINT('',(-0.0346589653438087,0.0159689110867543,0.103));
#35254=CARTESIAN_POINT('',(0.,0.,0.103));
#35255=CARTESIAN_POINT('',(0.,0.,0.103));
#35256=CARTESIAN_POINT('',(0.00943317780363869,0.,0.103));
#35257=CARTESIAN_POINT('',(0.,0.,0.103));
#35258=CARTESIAN_POINT('',(0.045,0.,0.103));
#35259=CARTESIAN_POINT('',(-0.0311589653438087,0.0220310889132454,0.103));
#35260=CARTESIAN_POINT('',(-0.00349999999999973,-0.038,0.103));
#35261=CARTESIAN_POINT('',(0.0346589653438085,0.0159689110867548,0.103));
#35262=CARTESIAN_POINT('',(0.,0.,0.104));
#35263=CARTESIAN_POINT('',(0.,0.,0.104));
#35264=CARTESIAN_POINT('',(0.00943317780363869,0.,0.104));
#35265=CARTESIAN_POINT('',(0.,0.,0.104));
#35266=CARTESIAN_POINT('',(0.045,0.,0.104));
#35267=CARTESIAN_POINT('',(0.,0.,0.104));
#35268=CARTESIAN_POINT('',(0.,0.,0.104));
#35269=CARTESIAN_POINT('',(-0.0311589653438087,0.0220310889132454,0.0902404553740472));
#35270=CARTESIAN_POINT('',(-0.00349999999999973,-0.038,0.0902404553740472));
#35271=CARTESIAN_POINT('',(0.0346589653438085,0.0159689110867548,0.0902404553740472));
#35272=CARTESIAN_POINT('',(-1.86123235344752E-18,6.93495810333095E-19,0.0107004836836099));
#35273=CARTESIAN_POINT('',(-0.012319152044289,0.0297373126961043,0.011));
#35274=CARTESIAN_POINT('',(-0.0115,0.0303108891324553,0.018));
#35275=CARTESIAN_POINT('',(-0.00863296784498857,0.032318406659684,0.018));
#35276=CARTESIAN_POINT('',(-0.010680847955711,0.0308844655688064,0.018));
#35277=CARTESIAN_POINT('',(-0.010680847955711,0.0308844655688064,0.011));
#35278=CARTESIAN_POINT('',(-0.010680847955711,0.0308844655688064,0.021));
#35279=CARTESIAN_POINT('',(-0.010680847955711,0.0308844655688064,0.021));
#35280=CARTESIAN_POINT('',(-0.00863296784498857,0.032318406659684,0.021));
#35281=CARTESIAN_POINT('',(-0.00863296784498857,0.032318406659684,0.011));
#35282=CARTESIAN_POINT('',(-0.010680847955711,0.0297373126961043,0.011));
#35283=CARTESIAN_POINT('',(-0.0115,0.0303108891324553,0.018));
#35284=CARTESIAN_POINT('',(-0.012319152044289,0.0308844655688064,0.018));
#35285=CARTESIAN_POINT('',(-0.0143670321550115,0.032318406659684,0.018));
#35286=CARTESIAN_POINT('',(-0.0143670321550115,0.032318406659684,0.011));
#35287=CARTESIAN_POINT('',(-0.0143670321550115,0.032318406659684,0.021));
#35288=CARTESIAN_POINT('',(-0.012319152044289,0.0308844655688064,0.021));
#35289=CARTESIAN_POINT('',(-0.012319152044289,0.0308844655688064,0.021));
#35290=CARTESIAN_POINT('',(-0.012319152044289,0.0308844655688064,0.011));
#35291=CARTESIAN_POINT('',(-0.012319152044289,0.0297373126961043,0.011));
#35292=CARTESIAN_POINT('',(-0.0115,0.0303108891324553,0.018));
#35293=CARTESIAN_POINT('',(-0.0143670321550115,0.0283033716052267,0.018));
#35294=CARTESIAN_POINT('',(-0.012319152044289,0.0297373126961043,0.018));
#35295=CARTESIAN_POINT('',(-0.012319152044289,0.0297373126961043,0.011));
#35296=CARTESIAN_POINT('',(-0.012319152044289,0.0297373126961043,0.021));
#35297=CARTESIAN_POINT('',(-0.012319152044289,0.0297373126961043,0.021));
#35298=CARTESIAN_POINT('',(-0.0143670321550115,0.0283033716052267,0.021));
#35299=CARTESIAN_POINT('',(-0.0143670321550115,0.0283033716052267,0.011));
#35300=CARTESIAN_POINT('',(-0.010680847955711,0.0297373126961043,0.011));
#35301=CARTESIAN_POINT('',(-0.0115,0.0303108891324553,0.018));
#35302=CARTESIAN_POINT('',(-0.010680847955711,0.0297373126961043,0.018));
#35303=CARTESIAN_POINT('',(-0.00863296784498857,0.0283033716052267,0.018));
#35304=CARTESIAN_POINT('',(-0.00863296784498857,0.0283033716052267,0.011));
#35305=CARTESIAN_POINT('',(-0.00863296784498857,0.0283033716052267,0.021));
#35306=CARTESIAN_POINT('',(-0.010680847955711,0.0297373126961043,0.021));
#35307=CARTESIAN_POINT('',(-0.010680847955711,0.0297373126961043,0.021));
#35308=CARTESIAN_POINT('',(-0.010680847955711,0.0297373126961043,0.011));
#35309=CARTESIAN_POINT('',(-0.012852081728299,0.0305608891324553,0.026));
#35310=CARTESIAN_POINT('',(-0.014204163456598,0.0308108891324553,0.026));
#35311=CARTESIAN_POINT('',(-0.0146732429566961,0.0308976219627052,0.026));
#35312=CARTESIAN_POINT('',(-0.0137350839565,0.0307241563022055,0.026));
#35313=CARTESIAN_POINT('',(-0.0115,0.0303108891324553,0.026));
#35314=CARTESIAN_POINT('',(-0.0146732429566961,0.0297241563022054,0.026));
#35315=CARTESIAN_POINT('',(-0.014204163456598,0.0298108891324554,0.026));
#35316=CARTESIAN_POINT('',(-0.0137350839565,0.0298976219627052,0.026));
#35317=CARTESIAN_POINT('',(-0.0115,0.0303108891324553,0.026));
#35318=CARTESIAN_POINT('',(-0.014204163456598,0.0298108891324554,0.026));
#35319=CARTESIAN_POINT('',(-0.014204163456598,0.0298108891324554,0.021));
#35320=CARTESIAN_POINT('',(-0.0137350839565,0.0298976219627052,0.021));
#35321=CARTESIAN_POINT('',(-0.0146732429566961,0.0297241563022054,0.021));
#35322=CARTESIAN_POINT('',(-0.0137350839565,0.0298976219627052,0.026));
#35323=CARTESIAN_POINT('',(-0.0146732429566961,0.0297241563022054,0.026));
#35324=CARTESIAN_POINT('',(-0.014204163456598,0.0308108891324553,0.026));
#35325=CARTESIAN_POINT('',(-0.014204163456598,0.0308108891324553,0.021));
#35326=CARTESIAN_POINT('',(-0.0146732429566961,0.0308976219627052,0.021));
#35327=CARTESIAN_POINT('',(-0.0137350839565,0.0307241563022055,0.021));
#35328=CARTESIAN_POINT('',(-0.0146732429566961,0.0308976219627052,0.026));
#35329=CARTESIAN_POINT('',(-0.0137350839565,0.0307241563022055,0.026));
#35330=CARTESIAN_POINT('',(-0.012852081728299,0.0305608891324553,0.026));
#35331=CARTESIAN_POINT('',(-0.00879583654340205,0.0308108891324553,0.026));
#35332=CARTESIAN_POINT('',(-0.0092649160435001,0.0307241563022055,0.026));
#35333=CARTESIAN_POINT('',(-0.008326757043304,0.0308976219627052,0.026));
#35334=CARTESIAN_POINT('',(-0.0115,0.0303108891324553,0.026));
#35335=CARTESIAN_POINT('',(-0.0092649160435001,0.0298976219627052,0.026));
#35336=CARTESIAN_POINT('',(-0.00879583654340205,0.0298108891324554,0.026));
#35337=CARTESIAN_POINT('',(-0.00832675704330399,0.0297241563022054,0.026));
#35338=CARTESIAN_POINT('',(-0.0115,0.0303108891324553,0.026));
#35339=CARTESIAN_POINT('',(-0.0115,0.0303108891324553,0.026));
#35340=CARTESIAN_POINT('',(-0.0115,0.0303108891324553,0.021));
#35341=CARTESIAN_POINT('',(-0.00832675704330399,0.0308976219627052,0.021));
#35342=CARTESIAN_POINT('',(-0.008326757043304,0.0297241563022054,0.021));
#35343=CARTESIAN_POINT('',(-0.008326757043304,0.0308976219627052,0.026));
#35344=CARTESIAN_POINT('',(-0.008326757043304,0.0297241563022054,0.026));
#35345=CARTESIAN_POINT('',(-0.0115,0.0303108891324553,0.026));
#35346=CARTESIAN_POINT('',(-0.0115,0.0303108891324553,0.021));
#35347=CARTESIAN_POINT('',(-0.0092649160435001,0.0298976219627052,0.021));
#35348=CARTESIAN_POINT('',(-0.0092649160435001,0.0307241563022055,0.021));
#35349=CARTESIAN_POINT('',(-0.0092649160435001,0.0298976219627052,0.026));
#35350=CARTESIAN_POINT('',(-0.0092649160435001,0.0307241563022055,0.026));
#35351=CARTESIAN_POINT('',(-0.0115,0.0303108891324553,0.018));
#35352=CARTESIAN_POINT('',(-0.0115,0.0303108891324553,0.018));
#35353=CARTESIAN_POINT('',(-0.0115,0.0303108891324553,0.018));
#35354=CARTESIAN_POINT('',(-0.0115,0.0303108891324553,0.018));
#35355=CARTESIAN_POINT('',(-0.0115,0.0303108891324553,0.018));
#35356=CARTESIAN_POINT('',(0.,0.,0.025));
#35357=CARTESIAN_POINT('',(-0.0115,0.0303108891324553,0.025));
#35358=CARTESIAN_POINT('',(-0.0125,0.0303108891324553,0.025));
#35359=CARTESIAN_POINT('',(-0.0115,0.0303108891324553,0.021));
#35360=CARTESIAN_POINT('',(-0.0115,0.0303108891324553,0.021));
#35361=CARTESIAN_POINT('',(-0.0115,0.0303108891324553,0.021));
#35362=CARTESIAN_POINT('',(-0.00879583654340205,0.0308108891324553,0.021));
#35363=CARTESIAN_POINT('',(-0.00879583654340205,0.0298108891324554,0.021));
#35364=CARTESIAN_POINT('',(-0.0115,0.0303108891324553,0.018));
#35365=CARTESIAN_POINT('',(-0.0115,0.0303108891324553,0.021));
#35366=CARTESIAN_POINT('',(-0.0115,0.0303108891324553,0.021));
#35367=CARTESIAN_POINT('',(-0.0115,0.0303108891324553,0.021));
#35368=CARTESIAN_POINT('',(-0.0115,0.0303108891324553,0.021));
#35369=CARTESIAN_POINT('',(-0.0115,0.0303108891324553,0.021));
#35370=CARTESIAN_POINT('',(-0.0115,0.0303108891324553,0.025));
#35371=CARTESIAN_POINT('',(-0.0115,0.0303108891324553,0.018));
#35372=CARTESIAN_POINT('',(-0.00879583654340205,0.0308108891324553,0.026));
#35373=CARTESIAN_POINT('',(-0.00879583654340205,0.0298108891324554,0.026));
#35374=CARTESIAN_POINT('',(-0.0115,0.0303108891324553,0.026));
#35375=CARTESIAN_POINT('',(-0.0115,0.0303108891324553,0.026));
#35376=CARTESIAN_POINT('',(-0.00427548757800059,-0.00209454669551009,-3.46944695195361E-18));
#35377=CARTESIAN_POINT('',(0.,0.,0.0840000001));
#35378=CARTESIAN_POINT('',(0.,0.,0.0840000001));
#35379=CARTESIAN_POINT('',(0.05,0.,0.0840000001));
#35380=CARTESIAN_POINT('',(0.,0.,0.0840000001));
#35381=CARTESIAN_POINT('',(0.053,0.,0.0840000001));
#35382=CARTESIAN_POINT('',(0.04368363807983,0.0108046177216235,0.083));
#35383=CARTESIAN_POINT('',(0.04368363807983,0.0108046177216235,0.071));
#35384=CARTESIAN_POINT('',(0.0439923368914681,0.00581415631573189,0.071));
#35385=CARTESIAN_POINT('',(0.0485373756442556,0.0120051308018038,0.071));
#35386=CARTESIAN_POINT('',(0.0439923368914681,0.00581415631573189,0.071));
#35387=CARTESIAN_POINT('',(0.0439923368914681,0.00581415631573189,0.081));
#35388=CARTESIAN_POINT('',(0.04368363807983,0.0108046177216235,0.081));
#35389=CARTESIAN_POINT('',(0.0485373756442556,0.0120051308018038,0.081));
#35390=CARTESIAN_POINT('',(0.0485373756442556,0.0120051308018038,0.083));
#35391=CARTESIAN_POINT('',(0.00256146516479152,-0.04,0.081));
#35392=CARTESIAN_POINT('',(0.043,-1.7347234759768E-17,0.081));
#35393=CARTESIAN_POINT('',(0.041603,-1.7347234759768E-17,0.081));
#35394=CARTESIAN_POINT('',(0.04,0.0025614651647911,0.081));
#35395=CARTESIAN_POINT('',(0.037,0.0025614651647911,0.081));
#35396=CARTESIAN_POINT('',(0.0398147807130172,0.00555574200832604,0.081));
#35397=CARTESIAN_POINT('',(0.037,0.00256146516479108,0.081));
#35398=CARTESIAN_POINT('',(0.037,-0.00256146516479112,0.081));
#35399=CARTESIAN_POINT('',(0.04,-0.00256146516479113,0.081));
#35400=CARTESIAN_POINT('',(0.0398147807130172,-0.00555574200832608,0.081));
#35401=CARTESIAN_POINT('',(0.049618820174773,-0.00616219802209742,0.081));
#35402=CARTESIAN_POINT('',(0.0439923368914681,-0.00581415631573192,0.081));
#35403=CARTESIAN_POINT('',(0.04368363807983,-0.0108046177216235,0.081));
#35404=CARTESIAN_POINT('',(0.0485373756442556,-0.0120051308018039,0.081));
#35405=CARTESIAN_POINT('',(0.,0.,0.081));
#35406=CARTESIAN_POINT('',(0.049618820174773,0.00616219802209738,0.081));
#35407=CARTESIAN_POINT('',(0.04368363807983,-0.0108046177216235,0.083));
#35408=CARTESIAN_POINT('',(0.04368363807983,-0.0108046177216235,0.071));
#35409=CARTESIAN_POINT('',(0.0485373756442556,-0.0120051308018039,0.071));
#35410=CARTESIAN_POINT('',(0.0439923368914681,-0.00581415631573192,0.071));
#35411=CARTESIAN_POINT('',(0.0485373756442556,-0.0120051308018039,0.083));
#35412=CARTESIAN_POINT('',(0.0439923368914681,-0.00581415631573192,0.071));
#35413=CARTESIAN_POINT('',(0.00256146516479152,-0.04,0.071));
#35414=CARTESIAN_POINT('',(0.043,-1.7347234759768E-17,0.071));
#35415=CARTESIAN_POINT('',(0.041603,-1.7347234759768E-17,0.071));
#35416=CARTESIAN_POINT('',(0.04,0.0025614651647911,0.071));
#35417=CARTESIAN_POINT('',(0.037,0.0025614651647911,0.071));
#35418=CARTESIAN_POINT('',(0.0398147807130172,0.00555574200832604,0.071));
#35419=CARTESIAN_POINT('',(0.049618820174773,0.00616219802209738,0.071));
#35420=CARTESIAN_POINT('',(0.,0.,0.071));
#35421=CARTESIAN_POINT('',(0.049618820174773,-0.00616219802209742,0.071));
#35422=CARTESIAN_POINT('',(0.0398147807130172,-0.00555574200832608,0.071));
#35423=CARTESIAN_POINT('',(0.04,-0.00256146516479113,0.071));
#35424=CARTESIAN_POINT('',(0.037,-0.00256146516479112,0.071));
#35425=CARTESIAN_POINT('',(0.037,0.00256146516479108,0.071));
#35426=CARTESIAN_POINT('',(0.00256146516479152,-0.04,0.081));
#35427=CARTESIAN_POINT('',(-1.32786462810487E-16,0.043,0.081));
#35428=CARTESIAN_POINT('',(-1.27908863380123E-16,0.041603,0.081));
#35429=CARTESIAN_POINT('',(-0.00256146516479124,0.04,0.081));
#35430=CARTESIAN_POINT('',(-0.00256146516479123,0.037,0.081));
#35431=CARTESIAN_POINT('',(-0.00555574200832618,0.0398147807130172,0.081));
#35432=CARTESIAN_POINT('',(-0.00256146516479121,0.037,0.081));
#35433=CARTESIAN_POINT('',(0.002561465164791,0.037,0.081));
#35434=CARTESIAN_POINT('',(0.00256146516479099,0.04,0.081));
#35435=CARTESIAN_POINT('',(0.00555574200832594,0.0398147807130172,0.081));
#35436=CARTESIAN_POINT('',(0.00616219802209724,0.049618820174773,0.081));
#35437=CARTESIAN_POINT('',(0.00581415631573177,0.0439923368914681,0.081));
#35438=CARTESIAN_POINT('',(0.0108046177216233,0.0436836380798301,0.081));
#35439=CARTESIAN_POINT('',(0.0120051308018037,0.0485373756442557,0.081));
#35440=CARTESIAN_POINT('',(0.,0.,0.081));
#35441=CARTESIAN_POINT('',(-0.012005130801804,0.0485373756442556,0.081));
#35442=CARTESIAN_POINT('',(-0.0108046177216236,0.04368363807983,0.081));
#35443=CARTESIAN_POINT('',(-0.00581415631573204,0.0439923368914681,0.081));
#35444=CARTESIAN_POINT('',(-0.00616219802209755,0.049618820174773,0.081));
#35445=CARTESIAN_POINT('',(0.0108046177216233,0.0436836380798301,0.083));
#35446=CARTESIAN_POINT('',(0.0108046177216233,0.0436836380798301,0.071));
#35447=CARTESIAN_POINT('',(0.0120051308018037,0.0485373756442557,0.071));
#35448=CARTESIAN_POINT('',(0.00581415631573177,0.0439923368914681,0.071));
#35449=CARTESIAN_POINT('',(0.0120051308018037,0.0485373756442557,0.083));
#35450=CARTESIAN_POINT('',(0.00581415631573177,0.0439923368914681,0.071));
#35451=CARTESIAN_POINT('',(0.00256146516479152,-0.04,0.071));
#35452=CARTESIAN_POINT('',(-1.32786462810487E-16,0.043,0.071));
#35453=CARTESIAN_POINT('',(-1.27908863380123E-16,0.041603,0.071));
#35454=CARTESIAN_POINT('',(-0.00256146516479124,0.04,0.071));
#35455=CARTESIAN_POINT('',(-0.00256146516479123,0.037,0.071));
#35456=CARTESIAN_POINT('',(-0.00555574200832618,0.0398147807130172,0.071));
#35457=CARTESIAN_POINT('',(-0.00616219802209755,0.049618820174773,0.071));
#35458=CARTESIAN_POINT('',(-0.00581415631573204,0.0439923368914681,0.071));
#35459=CARTESIAN_POINT('',(-0.0108046177216236,0.04368363807983,0.071));
#35460=CARTESIAN_POINT('',(-0.012005130801804,0.0485373756442556,0.071));
#35461=CARTESIAN_POINT('',(0.,0.,0.071));
#35462=CARTESIAN_POINT('',(0.00616219802209724,0.049618820174773,0.071));
#35463=CARTESIAN_POINT('',(0.00555574200832594,0.0398147807130172,0.071));
#35464=CARTESIAN_POINT('',(0.00256146516479099,0.04,0.071));
#35465=CARTESIAN_POINT('',(0.002561465164791,0.037,0.071));
#35466=CARTESIAN_POINT('',(-0.00256146516479121,0.037,0.071));
#35467=CARTESIAN_POINT('',(-0.0108046177216236,0.04368363807983,0.083));
#35468=CARTESIAN_POINT('',(-0.00581415631573204,0.0439923368914681,0.071));
#35469=CARTESIAN_POINT('',(-0.012005130801804,0.0485373756442556,0.083));
#35470=CARTESIAN_POINT('',(0.00256146516479152,-0.04,0.081));
#35471=CARTESIAN_POINT('',(-0.043,1.7347234759768E-17,0.081));
#35472=CARTESIAN_POINT('',(-0.041603,1.7347234759768E-17,0.081));
#35473=CARTESIAN_POINT('',(-0.04,-0.0025614651647911,0.081));
#35474=CARTESIAN_POINT('',(-0.037,-0.0025614651647911,0.081));
#35475=CARTESIAN_POINT('',(-0.0398147807130172,-0.00555574200832604,0.081));
#35476=CARTESIAN_POINT('',(-0.037,-0.00256146516479108,0.081));
#35477=CARTESIAN_POINT('',(-0.037,0.00256146516479112,0.081));
#35478=CARTESIAN_POINT('',(-0.04,0.00256146516479113,0.081));
#35479=CARTESIAN_POINT('',(-0.0398147807130172,0.00555574200832608,0.081));
#35480=CARTESIAN_POINT('',(-0.049618820174773,0.00616219802209742,0.081));
#35481=CARTESIAN_POINT('',(-0.0439923368914681,0.00581415631573192,0.081));
#35482=CARTESIAN_POINT('',(-0.04368363807983,0.0108046177216235,0.081));
#35483=CARTESIAN_POINT('',(-0.0485373756442556,0.0120051308018039,0.081));
#35484=CARTESIAN_POINT('',(0.,0.,0.081));
#35485=CARTESIAN_POINT('',(-0.0485373756442556,-0.0120051308018038,0.081));
#35486=CARTESIAN_POINT('',(-0.04368363807983,-0.0108046177216235,0.081));
#35487=CARTESIAN_POINT('',(-0.0439923368914681,-0.00581415631573189,0.081));
#35488=CARTESIAN_POINT('',(-0.049618820174773,-0.00616219802209738,0.081));
#35489=CARTESIAN_POINT('',(0.00256146516479152,-0.04,0.071));
#35490=CARTESIAN_POINT('',(-0.043,1.7347234759768E-17,0.071));
#35491=CARTESIAN_POINT('',(-0.041603,1.7347234759768E-17,0.071));
#35492=CARTESIAN_POINT('',(-0.04,-0.0025614651647911,0.071));
#35493=CARTESIAN_POINT('',(-0.037,-0.0025614651647911,0.071));
#35494=CARTESIAN_POINT('',(-0.0398147807130172,-0.00555574200832604,0.071));
#35495=CARTESIAN_POINT('',(-0.049618820174773,-0.00616219802209738,0.071));
#35496=CARTESIAN_POINT('',(-0.0439923368914681,-0.00581415631573189,0.071));
#35497=CARTESIAN_POINT('',(-0.04368363807983,-0.0108046177216235,0.071));
#35498=CARTESIAN_POINT('',(-0.0485373756442556,-0.0120051308018038,0.071));
#35499=CARTESIAN_POINT('',(0.,0.,0.071));
#35500=CARTESIAN_POINT('',(-0.0485373756442556,0.0120051308018039,0.071));
#35501=CARTESIAN_POINT('',(-0.04368363807983,0.0108046177216235,0.071));
#35502=CARTESIAN_POINT('',(-0.0439923368914681,0.00581415631573192,0.071));
#35503=CARTESIAN_POINT('',(-0.049618820174773,0.00616219802209742,0.071));
#35504=CARTESIAN_POINT('',(-0.0398147807130172,0.00555574200832608,0.071));
#35505=CARTESIAN_POINT('',(-0.04,0.00256146516479113,0.071));
#35506=CARTESIAN_POINT('',(-0.037,0.00256146516479112,0.071));
#35507=CARTESIAN_POINT('',(-0.037,-0.00256146516479108,0.071));
#35508=CARTESIAN_POINT('',(0.00256146516479152,-0.04,0.081));
#35509=CARTESIAN_POINT('',(4.33053857950996E-16,-0.043,0.081));
#35510=CARTESIAN_POINT('',(4.18421059659904E-16,-0.041603,0.081));
#35511=CARTESIAN_POINT('',(0.00256146516479152,-0.04,0.081));
#35512=CARTESIAN_POINT('',(0.00256146516479148,-0.037,0.081));
#35513=CARTESIAN_POINT('',(0.00555574200832646,-0.0398147807130171,0.081));
#35514=CARTESIAN_POINT('',(0.00256146516479147,-0.037,0.081));
#35515=CARTESIAN_POINT('',(-0.00256146516479074,-0.037,0.081));
#35516=CARTESIAN_POINT('',(-0.00256146516479072,-0.04,0.081));
#35517=CARTESIAN_POINT('',(-0.00555574200832566,-0.0398147807130173,0.081));
#35518=CARTESIAN_POINT('',(-0.0061621980220969,-0.049618820174773,0.081));
#35519=CARTESIAN_POINT('',(-0.00581415631573146,-0.0439923368914682,0.081));
#35520=CARTESIAN_POINT('',(-0.010804617721623,-0.0436836380798302,0.081));
#35521=CARTESIAN_POINT('',(-0.0120051308018034,-0.0485373756442558,0.081));
#35522=CARTESIAN_POINT('',(0.,0.,0.081));
#35523=CARTESIAN_POINT('',(0.0120051308018043,-0.0485373756442555,0.081));
#35524=CARTESIAN_POINT('',(0.0108046177216239,-0.0436836380798299,0.081));
#35525=CARTESIAN_POINT('',(0.00581415631573235,-0.043992336891468,0.081));
#35526=CARTESIAN_POINT('',(0.0061621980220979,-0.0496188201747729,0.081));
#35527=CARTESIAN_POINT('',(-0.010804617721623,-0.0436836380798302,0.083));
#35528=CARTESIAN_POINT('',(-0.010804617721623,-0.0436836380798302,0.071));
#35529=CARTESIAN_POINT('',(-0.0120051308018034,-0.0485373756442558,0.071));
#35530=CARTESIAN_POINT('',(-0.00581415631573146,-0.0439923368914682,0.071));
#35531=CARTESIAN_POINT('',(-0.0120051308018034,-0.0485373756442558,0.083));
#35532=CARTESIAN_POINT('',(-0.00581415631573146,-0.0439923368914682,0.071));
#35533=CARTESIAN_POINT('',(0.00256146516479152,-0.04,0.071));
#35534=CARTESIAN_POINT('',(4.33053857950996E-16,-0.043,0.071));
#35535=CARTESIAN_POINT('',(4.18421059659904E-16,-0.041603,0.071));
#35536=CARTESIAN_POINT('',(0.00256146516479152,-0.04,0.071));
#35537=CARTESIAN_POINT('',(0.00256146516479148,-0.037,0.071));
#35538=CARTESIAN_POINT('',(0.00555574200832646,-0.0398147807130171,0.071));
#35539=CARTESIAN_POINT('',(0.0061621980220979,-0.0496188201747729,0.071));
#35540=CARTESIAN_POINT('',(0.00581415631573235,-0.043992336891468,0.071));
#35541=CARTESIAN_POINT('',(0.0108046177216239,-0.0436836380798299,0.071));
#35542=CARTESIAN_POINT('',(0.0120051308018043,-0.0485373756442555,0.071));
#35543=CARTESIAN_POINT('',(0.,0.,0.071));
#35544=CARTESIAN_POINT('',(-0.0061621980220969,-0.049618820174773,0.071));
#35545=CARTESIAN_POINT('',(-0.00555574200832566,-0.0398147807130173,0.071));
#35546=CARTESIAN_POINT('',(-0.00256146516479072,-0.04,0.071));
#35547=CARTESIAN_POINT('',(-0.00256146516479074,-0.037,0.071));
#35548=CARTESIAN_POINT('',(0.00256146516479147,-0.037,0.071));
#35549=CARTESIAN_POINT('',(0.0108046177216239,-0.0436836380798299,0.083));
#35550=CARTESIAN_POINT('',(0.00581415631573235,-0.043992336891468,0.071));
#35551=CARTESIAN_POINT('',(0.0120051308018043,-0.0485373756442555,0.083));
#35552=CARTESIAN_POINT('',(0.049618820174773,0.00616219802209738,0.071));
#35553=CARTESIAN_POINT('',(0.0398147807130172,0.00555574200832604,0.071));
#35554=CARTESIAN_POINT('',(0.04,0.0025614651647911,0.071));
#35555=CARTESIAN_POINT('',(0.037,0.00256146516479108,0.071));
#35556=CARTESIAN_POINT('',(0.037,0.00256146516479108,0.071));
#35557=CARTESIAN_POINT('',(0.037,-0.00256146516479111,0.071));
#35558=CARTESIAN_POINT('',(0.04,-0.00256146516479113,0.071));
#35559=CARTESIAN_POINT('',(0.0398147807130172,-0.00555574200832608,0.071));
#35560=CARTESIAN_POINT('',(0.049618820174773,-0.00616219802209742,0.071));
#35561=CARTESIAN_POINT('',(-0.00256146516479124,0.04,0.071));
#35562=CARTESIAN_POINT('',(-0.00555574200832618,0.0398147807130172,0.071));
#35563=CARTESIAN_POINT('',(-0.00256146516479121,0.037,0.071));
#35564=CARTESIAN_POINT('',(-0.00256146516479121,0.037,0.071));
#35565=CARTESIAN_POINT('',(0.00256146516479098,0.037,0.071));
#35566=CARTESIAN_POINT('',(0.00256146516479099,0.04,0.071));
#35567=CARTESIAN_POINT('',(0.00555574200832594,0.0398147807130172,0.071));
#35568=CARTESIAN_POINT('',(0.00616219802209724,0.049618820174773,0.071));
#35569=CARTESIAN_POINT('',(-0.00616219802209755,0.049618820174773,0.071));
#35570=CARTESIAN_POINT('',(-0.04,-0.0025614651647911,0.071));
#35571=CARTESIAN_POINT('',(-0.0398147807130172,-0.00555574200832604,0.071));
#35572=CARTESIAN_POINT('',(-0.037,-0.00256146516479108,0.071));
#35573=CARTESIAN_POINT('',(-0.037,-0.00256146516479108,0.071));
#35574=CARTESIAN_POINT('',(-0.037,0.00256146516479111,0.071));
#35575=CARTESIAN_POINT('',(-0.04,0.00256146516479113,0.071));
#35576=CARTESIAN_POINT('',(-0.0398147807130172,0.00555574200832608,0.071));
#35577=CARTESIAN_POINT('',(-0.049618820174773,0.00616219802209742,0.071));
#35578=CARTESIAN_POINT('',(-0.0439923368914681,0.00581415631573192,0.071));
#35579=CARTESIAN_POINT('',(-0.049618820174773,-0.00616219802209738,0.071));
#35580=CARTESIAN_POINT('',(-0.0439923368914681,-0.00581415631573189,0.071));
#35581=CARTESIAN_POINT('',(0.00256146516479152,-0.04,0.071));
#35582=CARTESIAN_POINT('',(0.00555574200832646,-0.0398147807130171,0.071));
#35583=CARTESIAN_POINT('',(0.00256146516479147,-0.037,0.071));
#35584=CARTESIAN_POINT('',(0.00256146516479147,-0.037,0.071));
#35585=CARTESIAN_POINT('',(-0.00256146516479073,-0.037,0.071));
#35586=CARTESIAN_POINT('',(-0.00256146516479072,-0.04,0.071));
#35587=CARTESIAN_POINT('',(-0.00555574200832566,-0.0398147807130173,0.071));
#35588=CARTESIAN_POINT('',(-0.0061621980220969,-0.049618820174773,0.071));
#35589=CARTESIAN_POINT('',(0.0061621980220979,-0.0496188201747729,0.071));
#35590=CARTESIAN_POINT('',(-0.043,0.,-0.043));
#35591=CARTESIAN_POINT('',(0.,0.,-0.043));
#35592=CARTESIAN_POINT('',(-0.043,0.,-0.043));
#35593=CARTESIAN_POINT('',(-0.00668810118750004,0.0303108891324553,0.0216562499979517));
#35594=CARTESIAN_POINT('',(-0.00668810118750004,0.0347893242555984,0.0217499999979516));
#35595=CARTESIAN_POINT('',(-0.00985483303217851,0.0379560561002769,0.0218437499979517));
#35596=CARTESIAN_POINT('',(-0.013021564876857,0.0411227879449553,0.0219374999979516));
#35597=CARTESIAN_POINT('',(-0.0175,0.0411227879449554,0.0220312499979517));
#35598=CARTESIAN_POINT('',(-0.0219784351231431,0.0411227879449553,0.0221249999979516));
#35599=CARTESIAN_POINT('',(-0.0251451669678216,0.0379560561002769,0.0222187499979517));
#35600=CARTESIAN_POINT('',(-0.0283118988125,0.0347893242555984,0.0223124999979516));
#35601=CARTESIAN_POINT('',(-0.0283118988125,0.0303108891324553,0.0224062499979517));
#35602=CARTESIAN_POINT('',(-0.0283118988125,0.0258324540093123,0.0224999999979516));
#35603=CARTESIAN_POINT('',(-0.0251451669678216,0.0226657221646338,0.0225937499979517));
#35604=CARTESIAN_POINT('',(-0.0219784351231431,0.0194989903199553,0.0226874999979516));
#35605=CARTESIAN_POINT('',(-0.0175,0.0194989903199553,0.0227812499979517));
#35606=CARTESIAN_POINT('',(-0.013021564876857,0.0194989903199553,0.0228749999979516));
#35607=CARTESIAN_POINT('',(-0.00985483303217851,0.0226657221646338,0.0229687499979517));
#35608=CARTESIAN_POINT('',(-0.00668810118750004,0.0258324540093123,0.0230624999979516));
#35609=CARTESIAN_POINT('',(-0.00668810118750004,0.0303108891324553,0.0231562499979516));
#35610=CARTESIAN_POINT('',(-0.00668810118750004,0.0347893242555984,0.0232499999979516));
#35611=CARTESIAN_POINT('',(-0.00985483303217851,0.0379560561002769,0.0233437499979516));
#35612=CARTESIAN_POINT('',(-0.013021564876857,0.0411227879449553,0.0234374999979516));
#35613=CARTESIAN_POINT('',(-0.0175,0.0411227879449554,0.0235312499979516));
#35614=CARTESIAN_POINT('',(-0.0219784351231431,0.0411227879449553,0.0236249999979516));
#35615=CARTESIAN_POINT('',(-0.0251451669678216,0.0379560561002769,0.0237187499979516));
#35616=CARTESIAN_POINT('',(-0.0283118988125,0.0347893242555984,0.0238124999979517));
#35617=CARTESIAN_POINT('',(-0.0283118988125,0.0303108891324553,0.0239062499979516));
#35618=CARTESIAN_POINT('',(-0.0283118988125,0.0258324540093123,0.0239999999979516));
#35619=CARTESIAN_POINT('',(-0.0251451669678216,0.0226657221646338,0.0240937499979516));
#35620=CARTESIAN_POINT('',(-0.0219784351231431,0.0194989903199553,0.0241874999979516));
#35621=CARTESIAN_POINT('',(-0.0175,0.0194989903199553,0.0242812499979516));
#35622=CARTESIAN_POINT('',(-0.013021564876857,0.0194989903199553,0.0243749999979516));
#35623=CARTESIAN_POINT('',(-0.00985483303217851,0.0226657221646338,0.0244687499979516));
#35624=CARTESIAN_POINT('',(-0.00668810118750004,0.0258324540093123,0.0245624999979516));
#35625=CARTESIAN_POINT('',(-0.00668810118750004,0.0303108891324553,0.0246562499979517));
#35626=CARTESIAN_POINT('',(-0.00668810118750004,0.0347893242555984,0.0247499999979516));
#35627=CARTESIAN_POINT('',(-0.00985483303217851,0.0379560561002769,0.0248437499979517));
#35628=CARTESIAN_POINT('',(-0.013021564876857,0.0411227879449553,0.0249374999979516));
#35629=CARTESIAN_POINT('',(-0.0175,0.0411227879449554,0.0250312499979517));
#35630=CARTESIAN_POINT('',(-0.0219784351231431,0.0411227879449553,0.0251249999979516));
#35631=CARTESIAN_POINT('',(-0.0251451669678216,0.0379560561002769,0.0252187499979517));
#35632=CARTESIAN_POINT('',(-0.0283118988125,0.0347893242555984,0.0253124999979516));
#35633=CARTESIAN_POINT('',(-0.0283118988125,0.0303108891324553,0.0254062499979517));
#35634=CARTESIAN_POINT('',(-0.0283118988125,0.0258324540093123,0.0254999999979516));
#35635=CARTESIAN_POINT('',(-0.0251451669678216,0.0226657221646338,0.0255937499979517));
#35636=CARTESIAN_POINT('',(-0.0219784351231431,0.0194989903199553,0.0256874999979516));
#35637=CARTESIAN_POINT('',(-0.0175,0.0194989903199553,0.0257812499979517));
#35638=CARTESIAN_POINT('',(-0.013021564876857,0.0194989903199553,0.0258749999979516));
#35639=CARTESIAN_POINT('',(-0.00985483303217851,0.0226657221646338,0.0259687499979517));
#35640=CARTESIAN_POINT('',(-0.00668810118750004,0.0258324540093123,0.0260624999979516));
#35641=CARTESIAN_POINT('',(-0.00668810118750004,0.0303108891324553,0.0261562499979517));
#35642=CARTESIAN_POINT('',(-0.00668810118750004,0.0347893242555984,0.0262499999979516));
#35643=CARTESIAN_POINT('',(-0.00985483303217851,0.0379560561002769,0.0263437499979517));
#35644=CARTESIAN_POINT('',(-0.013021564876857,0.0411227879449553,0.0264374999979516));
#35645=CARTESIAN_POINT('',(-0.0175,0.0411227879449554,0.0265312499979517));
#35646=CARTESIAN_POINT('',(-0.0219784351231431,0.0411227879449553,0.0266249999979516));
#35647=CARTESIAN_POINT('',(-0.0251451669678216,0.0379560561002769,0.0267187499979517));
#35648=CARTESIAN_POINT('',(-0.0283118988125,0.0347893242555984,0.0268124999979516));
#35649=CARTESIAN_POINT('',(-0.0283118988125,0.0303108891324553,0.0269062499979516));
#35650=CARTESIAN_POINT('',(-0.0283118988125,0.0258324540093123,0.0269999999979516));
#35651=CARTESIAN_POINT('',(-0.0251451669678216,0.0226657221646338,0.0270937499979516));
#35652=CARTESIAN_POINT('',(-0.0219784351231431,0.0194989903199553,0.0271874999979516));
#35653=CARTESIAN_POINT('',(-0.0175,0.0194989903199553,0.0272812499979516));
#35654=CARTESIAN_POINT('',(-0.013021564876857,0.0194989903199553,0.0273749999979517));
#35655=CARTESIAN_POINT('',(-0.00985483303217851,0.0226657221646338,0.0274687499979516));
#35656=CARTESIAN_POINT('',(-0.00668810118750004,0.0258324540093123,0.0275624999979516));
#35657=CARTESIAN_POINT('',(-0.00668810118750004,0.0303108891324553,0.0276562499979516));
#35658=CARTESIAN_POINT('',(-0.0075,0.0303108891324553,0.0221249999959033));
#35659=CARTESIAN_POINT('',(-0.00750000000000004,0.0344530247561863,0.0222187499959032));
#35660=CARTESIAN_POINT('',(-0.0104289321881346,0.0373819569443208,0.0223124999959033));
#35661=CARTESIAN_POINT('',(-0.0133578643762691,0.0403108891324553,0.0224062499959032));
#35662=CARTESIAN_POINT('',(-0.0175,0.0403108891324553,0.0224999999959033));
#35663=CARTESIAN_POINT('',(-0.021642135623731,0.0403108891324553,0.0225937499959032));
#35664=CARTESIAN_POINT('',(-0.0245710678118655,0.0373819569443208,0.0226874999959033));
#35665=CARTESIAN_POINT('',(-0.0275000000000001,0.0344530247561863,0.0227812499959032));
#35666=CARTESIAN_POINT('',(-0.0275,0.0303108891324553,0.0228749999959033));
#35667=CARTESIAN_POINT('',(-0.0275000000000001,0.0261687535087244,0.0229687499959032));
#35668=CARTESIAN_POINT('',(-0.0245710678118655,0.0232398213205899,0.0230624999959032));
#35669=CARTESIAN_POINT('',(-0.021642135623731,0.0203108891324553,0.0231562499959032));
#35670=CARTESIAN_POINT('',(-0.0175,0.0203108891324553,0.0232499999959032));
#35671=CARTESIAN_POINT('',(-0.0133578643762691,0.0203108891324553,0.0233437499959032));
#35672=CARTESIAN_POINT('',(-0.0104289321881346,0.0232398213205899,0.0234374999959032));
#35673=CARTESIAN_POINT('',(-0.00750000000000004,0.0261687535087243,0.0235312499959032));
#35674=CARTESIAN_POINT('',(-0.0075,0.0303108891324553,0.0236249999959032));
#35675=CARTESIAN_POINT('',(-0.00750000000000004,0.0344530247561863,0.0237187499959032));
#35676=CARTESIAN_POINT('',(-0.0104289321881346,0.0373819569443208,0.0238124999959032));
#35677=CARTESIAN_POINT('',(-0.0133578643762691,0.0403108891324553,0.0239062499959032));
#35678=CARTESIAN_POINT('',(-0.0175,0.0403108891324553,0.0239999999959032));
#35679=CARTESIAN_POINT('',(-0.021642135623731,0.0403108891324553,0.0240937499959032));
#35680=CARTESIAN_POINT('',(-0.0245710678118655,0.0373819569443208,0.0241874999959032));
#35681=CARTESIAN_POINT('',(-0.0275000000000001,0.0344530247561863,0.0242812499959032));
#35682=CARTESIAN_POINT('',(-0.0275,0.0303108891324553,0.0243749999959033));
#35683=CARTESIAN_POINT('',(-0.0275000000000001,0.0261687535087244,0.0244687499959033));
#35684=CARTESIAN_POINT('',(-0.0245710678118655,0.0232398213205899,0.0245624999959033));
#35685=CARTESIAN_POINT('',(-0.021642135623731,0.0203108891324553,0.0246562499959032));
#35686=CARTESIAN_POINT('',(-0.0175,0.0203108891324553,0.0247499999959033));
#35687=CARTESIAN_POINT('',(-0.0133578643762691,0.0203108891324553,0.0248437499959032));
#35688=CARTESIAN_POINT('',(-0.0104289321881346,0.0232398213205899,0.0249374999959033));
#35689=CARTESIAN_POINT('',(-0.00750000000000004,0.0261687535087243,0.0250312499959033));
#35690=CARTESIAN_POINT('',(-0.0075,0.0303108891324553,0.0251249999959033));
#35691=CARTESIAN_POINT('',(-0.00750000000000004,0.0344530247561863,0.0252187499959032));
#35692=CARTESIAN_POINT('',(-0.0104289321881346,0.0373819569443208,0.0253124999959033));
#35693=CARTESIAN_POINT('',(-0.0133578643762691,0.0403108891324553,0.0254062499959032));
#35694=CARTESIAN_POINT('',(-0.0175,0.0403108891324553,0.0254999999959033));
#35695=CARTESIAN_POINT('',(-0.021642135623731,0.0403108891324553,0.0255937499959033));
#35696=CARTESIAN_POINT('',(-0.0245710678118655,0.0373819569443208,0.0256874999959033));
#35697=CARTESIAN_POINT('',(-0.0275000000000001,0.0344530247561863,0.0257812499959032));
#35698=CARTESIAN_POINT('',(-0.0275,0.0303108891324553,0.0258749999959033));
#35699=CARTESIAN_POINT('',(-0.0275000000000001,0.0261687535087244,0.0259687499959032));
#35700=CARTESIAN_POINT('',(-0.0245710678118655,0.0232398213205899,0.0260624999959033));
#35701=CARTESIAN_POINT('',(-0.021642135623731,0.0203108891324553,0.0261562499959033));
#35702=CARTESIAN_POINT('',(-0.0175,0.0203108891324553,0.0262499999959033));
#35703=CARTESIAN_POINT('',(-0.0133578643762691,0.0203108891324553,0.0263437499959032));
#35704=CARTESIAN_POINT('',(-0.0104289321881346,0.0232398213205899,0.0264374999959033));
#35705=CARTESIAN_POINT('',(-0.00750000000000004,0.0261687535087243,0.0265312499959032));
#35706=CARTESIAN_POINT('',(-0.0075,0.0303108891324553,0.0266249999959033));
#35707=CARTESIAN_POINT('',(-0.00750000000000004,0.0344530247561863,0.0267187499959033));
#35708=CARTESIAN_POINT('',(-0.0104289321881346,0.0373819569443208,0.0268124999959033));
#35709=CARTESIAN_POINT('',(-0.0133578643762691,0.0403108891324553,0.0269062499959032));
#35710=CARTESIAN_POINT('',(-0.0175,0.0403108891324553,0.0269999999959032));
#35711=CARTESIAN_POINT('',(-0.021642135623731,0.0403108891324553,0.0270937499959032));
#35712=CARTESIAN_POINT('',(-0.0245710678118655,0.0373819569443208,0.0271874999959032));
#35713=CARTESIAN_POINT('',(-0.0275000000000001,0.0344530247561863,0.0272812499959033));
#35714=CARTESIAN_POINT('',(-0.0275,0.0303108891324553,0.0273749999959032));
#35715=CARTESIAN_POINT('',(-0.0275000000000001,0.0261687535087244,0.0274687499959032));
#35716=CARTESIAN_POINT('',(-0.0245710678118655,0.0232398213205899,0.0275624999959032));
#35717=CARTESIAN_POINT('',(-0.021642135623731,0.0203108891324553,0.0276562499959032));
#35718=CARTESIAN_POINT('',(-0.0175,0.0203108891324553,0.0277499999959032));
#35719=CARTESIAN_POINT('',(-0.0133578643762691,0.0203108891324553,0.0278437499959033));
#35720=CARTESIAN_POINT('',(-0.0104289321881346,0.0232398213205899,0.0279374999959032));
#35721=CARTESIAN_POINT('',(-0.00750000000000004,0.0261687535087243,0.0280312499959032));
#35722=CARTESIAN_POINT('',(-0.0075,0.0303108891324553,0.0281249999959032));
#35723=CARTESIAN_POINT('',(-0.00709405059375004,0.0303108891324553,0.0218906249969274));
#35724=CARTESIAN_POINT('',(-0.00668810118750004,0.0303108891324553,0.0216562499979517));
#35725=CARTESIAN_POINT('',(-0.0075,0.0303108891324553,0.0221249999959033));
#35726=CARTESIAN_POINT('',(-0.0075,0.0303108891324553,0.0221249999959033));
#35727=CARTESIAN_POINT('',(-0.00750000000000004,0.0344530247561863,0.0222187499959032));
#35728=CARTESIAN_POINT('',(-0.0104289321881346,0.0373819569443208,0.0223124999959033));
#35729=CARTESIAN_POINT('',(-0.0133578643762691,0.0403108891324553,0.0224062499959032));
#35730=CARTESIAN_POINT('',(-0.0175,0.0403108891324553,0.0224999999959033));
#35731=CARTESIAN_POINT('',(-0.021642135623731,0.0403108891324553,0.0225937499959032));
#35732=CARTESIAN_POINT('',(-0.0245710678118655,0.0373819569443208,0.0226874999959033));
#35733=CARTESIAN_POINT('',(-0.0275000000000001,0.0344530247561862,0.0227812499959032));
#35734=CARTESIAN_POINT('',(-0.0275,0.0303108891324553,0.0228749999959033));
#35735=CARTESIAN_POINT('',(-0.0275,0.0303108891324553,0.0228749999959033));
#35736=CARTESIAN_POINT('',(-0.0275,0.0303108891324553,0.0228749999959033));
#35737=CARTESIAN_POINT('',(-0.0275000000000001,0.0261687535087244,0.0229687499959032));
#35738=CARTESIAN_POINT('',(-0.0245710678118655,0.0232398213205899,0.0230624999959032));
#35739=CARTESIAN_POINT('',(-0.021642135623731,0.0203108891324553,0.0231562499959032));
#35740=CARTESIAN_POINT('',(-0.0175,0.0203108891324553,0.0232499999959032));
#35741=CARTESIAN_POINT('',(-0.0133578643762691,0.0203108891324553,0.0233437499959032));
#35742=CARTESIAN_POINT('',(-0.0104289321881346,0.0232398213205899,0.0234374999959032));
#35743=CARTESIAN_POINT('',(-0.00750000000000003,0.0261687535087244,0.0235312499959033));
#35744=CARTESIAN_POINT('',(-0.0075,0.0303108891324553,0.0236249999959032));
#35745=CARTESIAN_POINT('',(-0.0075,0.0303108891324553,0.0236249999959032));
#35746=CARTESIAN_POINT('',(-0.0075,0.0303108891324553,0.0236249999959032));
#35747=CARTESIAN_POINT('',(-0.00750000000000005,0.0344530247561863,0.0237187499959033));
#35748=CARTESIAN_POINT('',(-0.0104289321881346,0.0373819569443208,0.0238124999959032));
#35749=CARTESIAN_POINT('',(-0.0133578643762691,0.0403108891324553,0.0239062499959032));
#35750=CARTESIAN_POINT('',(-0.0175,0.0403108891324553,0.0239999999959032));
#35751=CARTESIAN_POINT('',(-0.021642135623731,0.0403108891324553,0.0240937499959032));
#35752=CARTESIAN_POINT('',(-0.0245710678118655,0.0373819569443208,0.0241874999959032));
#35753=CARTESIAN_POINT('',(-0.0275,0.0344530247561863,0.0242812499959032));
#35754=CARTESIAN_POINT('',(-0.0275,0.0303108891324553,0.0243749999959032));
#35755=CARTESIAN_POINT('',(-0.0275,0.0303108891324553,0.0243749999959033));
#35756=CARTESIAN_POINT('',(-0.0275,0.0303108891324553,0.0243749999959033));
#35757=CARTESIAN_POINT('',(-0.0275000000000001,0.0261687535087244,0.0244687499959032));
#35758=CARTESIAN_POINT('',(-0.0245710678118655,0.0232398213205899,0.0245624999959033));
#35759=CARTESIAN_POINT('',(-0.021642135623731,0.0203108891324553,0.0246562499959032));
#35760=CARTESIAN_POINT('',(-0.0175,0.0203108891324553,0.0247499999959033));
#35761=CARTESIAN_POINT('',(-0.0133578643762691,0.0203108891324553,0.0248437499959032));
#35762=CARTESIAN_POINT('',(-0.0104289321881346,0.0232398213205899,0.0249374999959033));
#35763=CARTESIAN_POINT('',(-0.00750000000000006,0.0261687535087243,0.0250312499959033));
#35764=CARTESIAN_POINT('',(-0.0075,0.0303108891324553,0.0251249999959033));
#35765=CARTESIAN_POINT('',(-0.0075,0.0303108891324553,0.0251249999959033));
#35766=CARTESIAN_POINT('',(-0.0075,0.0303108891324553,0.0251249999959033));
#35767=CARTESIAN_POINT('',(-0.00750000000000002,0.0344530247561863,0.0252187499959033));
#35768=CARTESIAN_POINT('',(-0.0104289321881346,0.0373819569443208,0.0253124999959033));
#35769=CARTESIAN_POINT('',(-0.0133578643762691,0.0403108891324553,0.0254062499959032));
#35770=CARTESIAN_POINT('',(-0.0175,0.0403108891324553,0.0254999999959033));
#35771=CARTESIAN_POINT('',(-0.021642135623731,0.0403108891324553,0.0255937499959033));
#35772=CARTESIAN_POINT('',(-0.0245710678118655,0.0373819569443208,0.0256874999959033));
#35773=CARTESIAN_POINT('',(-0.0275000000000001,0.0344530247561863,0.0257812499959032));
#35774=CARTESIAN_POINT('',(-0.0275,0.0303108891324553,0.0258749999959033));
#35775=CARTESIAN_POINT('',(-0.0275,0.0303108891324553,0.0258749999959033));
#35776=CARTESIAN_POINT('',(-0.0275,0.0303108891324553,0.0258749999959033));
#35777=CARTESIAN_POINT('',(-0.0275000000000001,0.0261687535087244,0.0259687499959032));
#35778=CARTESIAN_POINT('',(-0.0245710678118655,0.0232398213205899,0.0260624999959033));
#35779=CARTESIAN_POINT('',(-0.021642135623731,0.0203108891324553,0.0261562499959033));
#35780=CARTESIAN_POINT('',(-0.0175,0.0203108891324553,0.0262499999959033));
#35781=CARTESIAN_POINT('',(-0.0133578643762691,0.0203108891324553,0.0263437499959032));
#35782=CARTESIAN_POINT('',(-0.0104289321881346,0.0232398213205899,0.0264374999959033));
#35783=CARTESIAN_POINT('',(-0.00750000000000004,0.0261687535087243,0.0265312499959032));
#35784=CARTESIAN_POINT('',(-0.0075,0.0303108891324553,0.0266249999959033));
#35785=CARTESIAN_POINT('',(-0.0075,0.0303108891324553,0.0266249999959033));
#35786=CARTESIAN_POINT('',(-0.0075,0.0303108891324553,0.0266249999959033));
#35787=CARTESIAN_POINT('',(-0.00750000000000004,0.0344530247561863,0.0267187499959033));
#35788=CARTESIAN_POINT('',(-0.0104289321881346,0.0373819569443208,0.0268124999959033));
#35789=CARTESIAN_POINT('',(-0.0133578643762691,0.0403108891324553,0.0269062499959032));
#35790=CARTESIAN_POINT('',(-0.0175,0.0403108891324553,0.0269999999959032));
#35791=CARTESIAN_POINT('',(-0.021642135623731,0.0403108891324553,0.0270937499959032));
#35792=CARTESIAN_POINT('',(-0.0245710678118655,0.0373819569443208,0.0271874999959032));
#35793=CARTESIAN_POINT('',(-0.0275000000000001,0.0344530247561863,0.0272812499959033));
#35794=CARTESIAN_POINT('',(-0.0275,0.0303108891324553,0.0273749999959032));
#35795=CARTESIAN_POINT('',(-0.0275,0.0303108891324553,0.0273749999959032));
#35796=CARTESIAN_POINT('',(-0.0275,0.0303108891324553,0.0273749999959032));
#35797=CARTESIAN_POINT('',(-0.0275000000000001,0.0261687535087244,0.0274687499959032));
#35798=CARTESIAN_POINT('',(-0.0245710678118655,0.0232398213205899,0.0275624999959032));
#35799=CARTESIAN_POINT('',(-0.021642135623731,0.0203108891324553,0.0276562499959032));
#35800=CARTESIAN_POINT('',(-0.0175,0.0203108891324553,0.0277499999959032));
#35801=CARTESIAN_POINT('',(-0.0133578643762691,0.0203108891324553,0.0278437499959033));
#35802=CARTESIAN_POINT('',(-0.0104289321881346,0.0232398213205899,0.0279374999959032));
#35803=CARTESIAN_POINT('',(-0.00750000000000004,0.0261687535087243,0.0280312499959032));
#35804=CARTESIAN_POINT('',(-0.0075,0.0303108891324553,0.0281249999959032));
#35805=CARTESIAN_POINT('',(-0.0075,0.0303108891324553,0.0281249999959032));
#35806=CARTESIAN_POINT('',(-0.00709405059375004,0.0303108891324553,0.0278906249969274));
#35807=CARTESIAN_POINT('',(-0.00668810118750004,0.0303108891324553,0.0276562499979516));
#35808=CARTESIAN_POINT('',(-0.00668810118750004,0.0303108891324553,0.0216562499979517));
#35809=CARTESIAN_POINT('',(-0.00668810118750004,0.0347893242555984,0.0217499999979516));
#35810=CARTESIAN_POINT('',(-0.00985483303217851,0.0379560561002769,0.0218437499979517));
#35811=CARTESIAN_POINT('',(-0.013021564876857,0.0411227879449553,0.0219374999979516));
#35812=CARTESIAN_POINT('',(-0.0175,0.0411227879449554,0.0220312499979517));
#35813=CARTESIAN_POINT('',(-0.0219784351231431,0.0411227879449553,0.0221249999979516));
#35814=CARTESIAN_POINT('',(-0.0251451669678216,0.0379560561002769,0.0222187499979517));
#35815=CARTESIAN_POINT('',(-0.0283118988125,0.0347893242555984,0.0223124999979516));
#35816=CARTESIAN_POINT('',(-0.0283118988125,0.0303108891324553,0.0224062499979517));
#35817=CARTESIAN_POINT('',(-0.0283118988125,0.0258324540093123,0.0224999999979516));
#35818=CARTESIAN_POINT('',(-0.0251451669678216,0.0226657221646338,0.0225937499979517));
#35819=CARTESIAN_POINT('',(-0.0219784351231431,0.0194989903199553,0.0226874999979516));
#35820=CARTESIAN_POINT('',(-0.0175,0.0194989903199553,0.0227812499979517));
#35821=CARTESIAN_POINT('',(-0.013021564876857,0.0194989903199553,0.0228749999979516));
#35822=CARTESIAN_POINT('',(-0.00985483303217851,0.0226657221646338,0.0229687499979517));
#35823=CARTESIAN_POINT('',(-0.00668810118750004,0.0258324540093123,0.0230624999979516));
#35824=CARTESIAN_POINT('',(-0.00668810118750004,0.0303108891324553,0.0231562499979516));
#35825=CARTESIAN_POINT('',(-0.00668810118750004,0.0347893242555984,0.0232499999979516));
#35826=CARTESIAN_POINT('',(-0.00985483303217851,0.0379560561002769,0.0233437499979516));
#35827=CARTESIAN_POINT('',(-0.013021564876857,0.0411227879449553,0.0234374999979516));
#35828=CARTESIAN_POINT('',(-0.0175,0.0411227879449554,0.0235312499979516));
#35829=CARTESIAN_POINT('',(-0.0219784351231431,0.0411227879449553,0.0236249999979516));
#35830=CARTESIAN_POINT('',(-0.0251451669678216,0.0379560561002769,0.0237187499979516));
#35831=CARTESIAN_POINT('',(-0.0283118988125,0.0347893242555984,0.0238124999979517));
#35832=CARTESIAN_POINT('',(-0.0283118988125,0.0303108891324553,0.0239062499979516));
#35833=CARTESIAN_POINT('',(-0.0283118988125,0.0258324540093123,0.0239999999979516));
#35834=CARTESIAN_POINT('',(-0.0251451669678216,0.0226657221646338,0.0240937499979516));
#35835=CARTESIAN_POINT('',(-0.0219784351231431,0.0194989903199553,0.0241874999979516));
#35836=CARTESIAN_POINT('',(-0.0175,0.0194989903199553,0.0242812499979516));
#35837=CARTESIAN_POINT('',(-0.013021564876857,0.0194989903199553,0.0243749999979516));
#35838=CARTESIAN_POINT('',(-0.00985483303217851,0.0226657221646338,0.0244687499979516));
#35839=CARTESIAN_POINT('',(-0.00668810118750004,0.0258324540093123,0.0245624999979516));
#35840=CARTESIAN_POINT('',(-0.00668810118750004,0.0303108891324553,0.0246562499979517));
#35841=CARTESIAN_POINT('',(-0.00668810118750004,0.0347893242555984,0.0247499999979516));
#35842=CARTESIAN_POINT('',(-0.00985483303217851,0.0379560561002769,0.0248437499979517));
#35843=CARTESIAN_POINT('',(-0.013021564876857,0.0411227879449553,0.0249374999979516));
#35844=CARTESIAN_POINT('',(-0.0175,0.0411227879449554,0.0250312499979517));
#35845=CARTESIAN_POINT('',(-0.0219784351231431,0.0411227879449553,0.0251249999979516));
#35846=CARTESIAN_POINT('',(-0.0251451669678216,0.0379560561002769,0.0252187499979517));
#35847=CARTESIAN_POINT('',(-0.0283118988125,0.0347893242555984,0.0253124999979516));
#35848=CARTESIAN_POINT('',(-0.0283118988125,0.0303108891324553,0.0254062499979517));
#35849=CARTESIAN_POINT('',(-0.0283118988125,0.0258324540093123,0.0254999999979516));
#35850=CARTESIAN_POINT('',(-0.0251451669678216,0.0226657221646338,0.0255937499979517));
#35851=CARTESIAN_POINT('',(-0.0219784351231431,0.0194989903199553,0.0256874999979516));
#35852=CARTESIAN_POINT('',(-0.0175,0.0194989903199553,0.0257812499979517));
#35853=CARTESIAN_POINT('',(-0.013021564876857,0.0194989903199553,0.0258749999979516));
#35854=CARTESIAN_POINT('',(-0.00985483303217851,0.0226657221646338,0.0259687499979517));
#35855=CARTESIAN_POINT('',(-0.00668810118750004,0.0258324540093123,0.0260624999979516));
#35856=CARTESIAN_POINT('',(-0.00668810118750004,0.0303108891324553,0.0261562499979517));
#35857=CARTESIAN_POINT('',(-0.00668810118750004,0.0347893242555984,0.0262499999979516));
#35858=CARTESIAN_POINT('',(-0.00985483303217851,0.0379560561002769,0.0263437499979517));
#35859=CARTESIAN_POINT('',(-0.013021564876857,0.0411227879449553,0.0264374999979516));
#35860=CARTESIAN_POINT('',(-0.0175,0.0411227879449554,0.0265312499979517));
#35861=CARTESIAN_POINT('',(-0.0219784351231431,0.0411227879449553,0.0266249999979516));
#35862=CARTESIAN_POINT('',(-0.0251451669678216,0.0379560561002769,0.0267187499979517));
#35863=CARTESIAN_POINT('',(-0.0283118988125,0.0347893242555984,0.0268124999979516));
#35864=CARTESIAN_POINT('',(-0.0283118988125,0.0303108891324553,0.0269062499979516));
#35865=CARTESIAN_POINT('',(-0.0283118988125,0.0258324540093123,0.0269999999979516));
#35866=CARTESIAN_POINT('',(-0.0251451669678216,0.0226657221646338,0.0270937499979516));
#35867=CARTESIAN_POINT('',(-0.0219784351231431,0.0194989903199553,0.0271874999979516));
#35868=CARTESIAN_POINT('',(-0.0175,0.0194989903199553,0.0272812499979516));
#35869=CARTESIAN_POINT('',(-0.013021564876857,0.0194989903199553,0.0273749999979517));
#35870=CARTESIAN_POINT('',(-0.00985483303217851,0.0226657221646338,0.0274687499979516));
#35871=CARTESIAN_POINT('',(-0.00668810118750004,0.0258324540093123,0.0275624999979516));
#35872=CARTESIAN_POINT('',(-0.00668810118750004,0.0303108891324553,0.0276562499979516));
#35873=CARTESIAN_POINT('',(-0.0075,0.0303108891324553,0.021));
#35874=CARTESIAN_POINT('',(-0.00750000000000004,0.0344530247561863,0.02109375));
#35875=CARTESIAN_POINT('',(-0.0104289321881346,0.0373819569443208,0.0211875));
#35876=CARTESIAN_POINT('',(-0.0133578643762691,0.0403108891324553,0.02128125));
#35877=CARTESIAN_POINT('',(-0.0175,0.0403108891324553,0.021375));
#35878=CARTESIAN_POINT('',(-0.021642135623731,0.0403108891324553,0.02146875));
#35879=CARTESIAN_POINT('',(-0.0245710678118655,0.0373819569443208,0.0215625));
#35880=CARTESIAN_POINT('',(-0.0275000000000001,0.0344530247561863,0.02165625));
#35881=CARTESIAN_POINT('',(-0.0275,0.0303108891324553,0.02175));
#35882=CARTESIAN_POINT('',(-0.0275000000000001,0.0261687535087244,0.02184375));
#35883=CARTESIAN_POINT('',(-0.0245710678118655,0.0232398213205899,0.0219375));
#35884=CARTESIAN_POINT('',(-0.021642135623731,0.0203108891324553,0.02203125));
#35885=CARTESIAN_POINT('',(-0.0175,0.0203108891324553,0.022125));
#35886=CARTESIAN_POINT('',(-0.0133578643762691,0.0203108891324553,0.02221875));
#35887=CARTESIAN_POINT('',(-0.0104289321881346,0.0232398213205899,0.0223125));
#35888=CARTESIAN_POINT('',(-0.00750000000000004,0.0261687535087243,0.02240625));
#35889=CARTESIAN_POINT('',(-0.0075,0.0303108891324553,0.0225));
#35890=CARTESIAN_POINT('',(-0.00750000000000004,0.0344530247561863,0.02259375));
#35891=CARTESIAN_POINT('',(-0.0104289321881346,0.0373819569443208,0.0226875));
#35892=CARTESIAN_POINT('',(-0.0133578643762691,0.0403108891324553,0.02278125));
#35893=CARTESIAN_POINT('',(-0.0175,0.0403108891324553,0.022875));
#35894=CARTESIAN_POINT('',(-0.021642135623731,0.0403108891324553,0.02296875));
#35895=CARTESIAN_POINT('',(-0.0245710678118655,0.0373819569443208,0.0230625));
#35896=CARTESIAN_POINT('',(-0.0275000000000001,0.0344530247561863,0.02315625));
#35897=CARTESIAN_POINT('',(-0.0275,0.0303108891324553,0.02325));
#35898=CARTESIAN_POINT('',(-0.0275000000000001,0.0261687535087244,0.02334375));
#35899=CARTESIAN_POINT('',(-0.0245710678118655,0.0232398213205899,0.0234375));
#35900=CARTESIAN_POINT('',(-0.021642135623731,0.0203108891324553,0.02353125));
#35901=CARTESIAN_POINT('',(-0.0175,0.0203108891324553,0.023625));
#35902=CARTESIAN_POINT('',(-0.0133578643762691,0.0203108891324553,0.02371875));
#35903=CARTESIAN_POINT('',(-0.0104289321881346,0.0232398213205899,0.0238125));
#35904=CARTESIAN_POINT('',(-0.00750000000000004,0.0261687535087243,0.02390625));
#35905=CARTESIAN_POINT('',(-0.0075,0.0303108891324553,0.024));
#35906=CARTESIAN_POINT('',(-0.00750000000000004,0.0344530247561863,0.02409375));
#35907=CARTESIAN_POINT('',(-0.0104289321881346,0.0373819569443208,0.0241875));
#35908=CARTESIAN_POINT('',(-0.0133578643762691,0.0403108891324553,0.02428125));
#35909=CARTESIAN_POINT('',(-0.0175,0.0403108891324553,0.024375));
#35910=CARTESIAN_POINT('',(-0.021642135623731,0.0403108891324553,0.02446875));
#35911=CARTESIAN_POINT('',(-0.0245710678118655,0.0373819569443208,0.0245625));
#35912=CARTESIAN_POINT('',(-0.0275000000000001,0.0344530247561863,0.02465625));
#35913=CARTESIAN_POINT('',(-0.0275,0.0303108891324553,0.02475));
#35914=CARTESIAN_POINT('',(-0.0275000000000001,0.0261687535087244,0.02484375));
#35915=CARTESIAN_POINT('',(-0.0245710678118655,0.0232398213205899,0.0249375));
#35916=CARTESIAN_POINT('',(-0.021642135623731,0.0203108891324553,0.02503125));
#35917=CARTESIAN_POINT('',(-0.0175,0.0203108891324553,0.025125));
#35918=CARTESIAN_POINT('',(-0.0133578643762691,0.0203108891324553,0.02521875));
#35919=CARTESIAN_POINT('',(-0.0104289321881346,0.0232398213205899,0.0253125));
#35920=CARTESIAN_POINT('',(-0.00750000000000004,0.0261687535087243,0.02540625));
#35921=CARTESIAN_POINT('',(-0.0075,0.0303108891324553,0.0255));
#35922=CARTESIAN_POINT('',(-0.00750000000000004,0.0344530247561863,0.02559375));
#35923=CARTESIAN_POINT('',(-0.0104289321881346,0.0373819569443208,0.0256875));
#35924=CARTESIAN_POINT('',(-0.0133578643762691,0.0403108891324553,0.02578125));
#35925=CARTESIAN_POINT('',(-0.0175,0.0403108891324553,0.025875));
#35926=CARTESIAN_POINT('',(-0.021642135623731,0.0403108891324553,0.02596875));
#35927=CARTESIAN_POINT('',(-0.0245710678118655,0.0373819569443208,0.0260625));
#35928=CARTESIAN_POINT('',(-0.0275000000000001,0.0344530247561863,0.02615625));
#35929=CARTESIAN_POINT('',(-0.0275,0.0303108891324553,0.02625));
#35930=CARTESIAN_POINT('',(-0.0275000000000001,0.0261687535087244,0.02634375));
#35931=CARTESIAN_POINT('',(-0.0245710678118655,0.0232398213205899,0.0264375));
#35932=CARTESIAN_POINT('',(-0.021642135623731,0.0203108891324553,0.02653125));
#35933=CARTESIAN_POINT('',(-0.0175,0.0203108891324553,0.026625));
#35934=CARTESIAN_POINT('',(-0.0133578643762691,0.0203108891324553,0.02671875));
#35935=CARTESIAN_POINT('',(-0.0104289321881346,0.0232398213205899,0.0268125));
#35936=CARTESIAN_POINT('',(-0.00750000000000004,0.0261687535087243,0.02690625));
#35937=CARTESIAN_POINT('',(-0.0075,0.0303108891324553,0.027));
#35938=CARTESIAN_POINT('',(-0.00668810118750004,0.0303108891324553,0.0214687499979517));
#35939=CARTESIAN_POINT('',(-0.00668810118750004,0.0347893242555984,0.0215624999979517));
#35940=CARTESIAN_POINT('',(-0.00985483303217851,0.0379560561002769,0.0216562499979517));
#35941=CARTESIAN_POINT('',(-0.013021564876857,0.0411227879449553,0.0217499999979516));
#35942=CARTESIAN_POINT('',(-0.0175,0.0411227879449554,0.0218437499979517));
#35943=CARTESIAN_POINT('',(-0.0219784351231431,0.0411227879449553,0.0219374999979516));
#35944=CARTESIAN_POINT('',(-0.0251451669678216,0.0379560561002769,0.0220312499979517));
#35945=CARTESIAN_POINT('',(-0.0283118988125,0.0347893242555984,0.0221249999979516));
#35946=CARTESIAN_POINT('',(-0.0283118988125,0.0303108891324553,0.0222187499979517));
#35947=CARTESIAN_POINT('',(-0.0283118988125,0.0258324540093123,0.0223124999979516));
#35948=CARTESIAN_POINT('',(-0.0251451669678216,0.0226657221646338,0.0224062499979517));
#35949=CARTESIAN_POINT('',(-0.0219784351231431,0.0194989903199553,0.0224999999979516));
#35950=CARTESIAN_POINT('',(-0.0175,0.0194989903199553,0.0225937499979517));
#35951=CARTESIAN_POINT('',(-0.013021564876857,0.0194989903199553,0.0226874999979516));
#35952=CARTESIAN_POINT('',(-0.00985483303217851,0.0226657221646338,0.0227812499979517));
#35953=CARTESIAN_POINT('',(-0.00668810118750004,0.0258324540093123,0.0228749999979516));
#35954=CARTESIAN_POINT('',(-0.00668810118750004,0.0303108891324553,0.0229687499979517));
#35955=CARTESIAN_POINT('',(-0.00668810118750004,0.0347893242555984,0.0230624999979516));
#35956=CARTESIAN_POINT('',(-0.00985483303217851,0.0379560561002769,0.0231562499979516));
#35957=CARTESIAN_POINT('',(-0.013021564876857,0.0411227879449553,0.0232499999979516));
#35958=CARTESIAN_POINT('',(-0.0175,0.0411227879449554,0.0233437499979516));
#35959=CARTESIAN_POINT('',(-0.0219784351231431,0.0411227879449553,0.0234374999979516));
#35960=CARTESIAN_POINT('',(-0.0251451669678216,0.0379560561002769,0.0235312499979516));
#35961=CARTESIAN_POINT('',(-0.0283118988125,0.0347893242555984,0.0236249999979516));
#35962=CARTESIAN_POINT('',(-0.0283118988125,0.0303108891324553,0.0237187499979516));
#35963=CARTESIAN_POINT('',(-0.0283118988125,0.0258324540093123,0.0238124999979517));
#35964=CARTESIAN_POINT('',(-0.0251451669678216,0.0226657221646338,0.0239062499979516));
#35965=CARTESIAN_POINT('',(-0.0219784351231431,0.0194989903199553,0.0239999999979516));
#35966=CARTESIAN_POINT('',(-0.0175,0.0194989903199553,0.0240937499979516));
#35967=CARTESIAN_POINT('',(-0.013021564876857,0.0194989903199553,0.0241874999979516));
#35968=CARTESIAN_POINT('',(-0.00985483303217851,0.0226657221646338,0.0242812499979516));
#35969=CARTESIAN_POINT('',(-0.00668810118750004,0.0258324540093123,0.0243749999979516));
#35970=CARTESIAN_POINT('',(-0.00668810118750004,0.0303108891324553,0.0244687499979516));
#35971=CARTESIAN_POINT('',(-0.00668810118750004,0.0347893242555984,0.0245624999979516));
#35972=CARTESIAN_POINT('',(-0.00985483303217851,0.0379560561002769,0.0246562499979517));
#35973=CARTESIAN_POINT('',(-0.013021564876857,0.0411227879449553,0.0247499999979516));
#35974=CARTESIAN_POINT('',(-0.0175,0.0411227879449554,0.0248437499979517));
#35975=CARTESIAN_POINT('',(-0.0219784351231431,0.0411227879449553,0.0249374999979516));
#35976=CARTESIAN_POINT('',(-0.0251451669678216,0.0379560561002769,0.0250312499979517));
#35977=CARTESIAN_POINT('',(-0.0283118988125,0.0347893242555984,0.0251249999979516));
#35978=CARTESIAN_POINT('',(-0.0283118988125,0.0303108891324553,0.0252187499979517));
#35979=CARTESIAN_POINT('',(-0.0283118988125,0.0258324540093123,0.0253124999979516));
#35980=CARTESIAN_POINT('',(-0.0251451669678216,0.0226657221646338,0.0254062499979517));
#35981=CARTESIAN_POINT('',(-0.0219784351231431,0.0194989903199553,0.0254999999979516));
#35982=CARTESIAN_POINT('',(-0.0175,0.0194989903199553,0.0255937499979517));
#35983=CARTESIAN_POINT('',(-0.013021564876857,0.0194989903199553,0.0256874999979516));
#35984=CARTESIAN_POINT('',(-0.00985483303217851,0.0226657221646338,0.0257812499979517));
#35985=CARTESIAN_POINT('',(-0.00668810118750004,0.0258324540093123,0.0258749999979516));
#35986=CARTESIAN_POINT('',(-0.00668810118750004,0.0303108891324553,0.0259687499979517));
#35987=CARTESIAN_POINT('',(-0.00668810118750004,0.0347893242555984,0.0260624999979516));
#35988=CARTESIAN_POINT('',(-0.00985483303217851,0.0379560561002769,0.0261562499979517));
#35989=CARTESIAN_POINT('',(-0.013021564876857,0.0411227879449553,0.0262499999979516));
#35990=CARTESIAN_POINT('',(-0.0175,0.0411227879449554,0.0263437499979517));
#35991=CARTESIAN_POINT('',(-0.0219784351231431,0.0411227879449553,0.0264374999979516));
#35992=CARTESIAN_POINT('',(-0.0251451669678216,0.0379560561002769,0.0265312499979517));
#35993=CARTESIAN_POINT('',(-0.0283118988125,0.0347893242555984,0.0266249999979516));
#35994=CARTESIAN_POINT('',(-0.0283118988125,0.0303108891324553,0.0267187499979517));
#35995=CARTESIAN_POINT('',(-0.0283118988125,0.0258324540093123,0.0268124999979516));
#35996=CARTESIAN_POINT('',(-0.0251451669678216,0.0226657221646338,0.0269062499979516));
#35997=CARTESIAN_POINT('',(-0.0219784351231431,0.0194989903199553,0.0269999999979516));
#35998=CARTESIAN_POINT('',(-0.0175,0.0194989903199553,0.0270937499979516));
#35999=CARTESIAN_POINT('',(-0.013021564876857,0.0194989903199553,0.0271874999979516));
#36000=CARTESIAN_POINT('',(-0.00985483303217851,0.0226657221646338,0.0272812499979516));
#36001=CARTESIAN_POINT('',(-0.00668810118750004,0.0258324540093123,0.0273749999979517));
#36002=CARTESIAN_POINT('',(-0.00668810118750004,0.0303108891324553,0.0274687499979516));
#36003=CARTESIAN_POINT('',(-0.00709405059375004,0.0303108891324553,0.0212343749989759));
#36004=CARTESIAN_POINT('',(-0.0075,0.0303108891324553,0.021));
#36005=CARTESIAN_POINT('',(-0.00668810118750004,0.0303108891324553,0.0214687499979517));
#36006=CARTESIAN_POINT('',(-0.00668810118750004,0.0303108891324553,0.0214687499979517));
#36007=CARTESIAN_POINT('',(-0.00668810118750004,0.0347893242555984,0.0215624999979517));
#36008=CARTESIAN_POINT('',(-0.00985483303217851,0.0379560561002769,0.0216562499979517));
#36009=CARTESIAN_POINT('',(-0.013021564876857,0.0411227879449553,0.0217499999979516));
#36010=CARTESIAN_POINT('',(-0.0175,0.0411227879449554,0.0218437499979517));
#36011=CARTESIAN_POINT('',(-0.0219784351231431,0.0411227879449553,0.0219374999979516));
#36012=CARTESIAN_POINT('',(-0.0251451669678216,0.0379560561002769,0.0220312499979517));
#36013=CARTESIAN_POINT('',(-0.0283118988125,0.0347893242555984,0.0221249999979516));
#36014=CARTESIAN_POINT('',(-0.0283118988125,0.0303108891324553,0.0222187499979517));
#36015=CARTESIAN_POINT('',(-0.0283118988125,0.0258324540093123,0.0223124999979516));
#36016=CARTESIAN_POINT('',(-0.0251451669678216,0.0226657221646338,0.0224062499979517));
#36017=CARTESIAN_POINT('',(-0.0219784351231431,0.0194989903199553,0.0224999999979516));
#36018=CARTESIAN_POINT('',(-0.0175,0.0194989903199553,0.0225937499979517));
#36019=CARTESIAN_POINT('',(-0.013021564876857,0.0194989903199553,0.0226874999979516));
#36020=CARTESIAN_POINT('',(-0.00985483303217851,0.0226657221646338,0.0227812499979517));
#36021=CARTESIAN_POINT('',(-0.00668810118750004,0.0258324540093123,0.0228749999979516));
#36022=CARTESIAN_POINT('',(-0.00668810118750004,0.0303108891324553,0.0229687499979517));
#36023=CARTESIAN_POINT('',(-0.00668810118750004,0.0347893242555984,0.0230624999979516));
#36024=CARTESIAN_POINT('',(-0.00985483303217851,0.0379560561002769,0.0231562499979516));
#36025=CARTESIAN_POINT('',(-0.013021564876857,0.0411227879449553,0.0232499999979516));
#36026=CARTESIAN_POINT('',(-0.0175,0.0411227879449554,0.0233437499979516));
#36027=CARTESIAN_POINT('',(-0.0219784351231431,0.0411227879449553,0.0234374999979516));
#36028=CARTESIAN_POINT('',(-0.0251451669678216,0.0379560561002769,0.0235312499979516));
#36029=CARTESIAN_POINT('',(-0.0283118988125,0.0347893242555984,0.0236249999979516));
#36030=CARTESIAN_POINT('',(-0.0283118988125,0.0303108891324553,0.0237187499979516));
#36031=CARTESIAN_POINT('',(-0.0283118988125,0.0258324540093123,0.0238124999979517));
#36032=CARTESIAN_POINT('',(-0.0251451669678216,0.0226657221646338,0.0239062499979516));
#36033=CARTESIAN_POINT('',(-0.0219784351231431,0.0194989903199553,0.0239999999979516));
#36034=CARTESIAN_POINT('',(-0.0175,0.0194989903199553,0.0240937499979516));
#36035=CARTESIAN_POINT('',(-0.013021564876857,0.0194989903199553,0.0241874999979516));
#36036=CARTESIAN_POINT('',(-0.00985483303217851,0.0226657221646338,0.0242812499979516));
#36037=CARTESIAN_POINT('',(-0.00668810118750004,0.0258324540093123,0.0243749999979516));
#36038=CARTESIAN_POINT('',(-0.00668810118750004,0.0303108891324553,0.0244687499979516));
#36039=CARTESIAN_POINT('',(-0.00668810118750004,0.0347893242555984,0.0245624999979516));
#36040=CARTESIAN_POINT('',(-0.00985483303217851,0.0379560561002769,0.0246562499979517));
#36041=CARTESIAN_POINT('',(-0.013021564876857,0.0411227879449553,0.0247499999979516));
#36042=CARTESIAN_POINT('',(-0.0175,0.0411227879449554,0.0248437499979517));
#36043=CARTESIAN_POINT('',(-0.0219784351231431,0.0411227879449553,0.0249374999979516));
#36044=CARTESIAN_POINT('',(-0.0251451669678216,0.0379560561002769,0.0250312499979517));
#36045=CARTESIAN_POINT('',(-0.0283118988125,0.0347893242555984,0.0251249999979516));
#36046=CARTESIAN_POINT('',(-0.0283118988125,0.0303108891324553,0.0252187499979517));
#36047=CARTESIAN_POINT('',(-0.0283118988125,0.0258324540093123,0.0253124999979516));
#36048=CARTESIAN_POINT('',(-0.0251451669678216,0.0226657221646338,0.0254062499979517));
#36049=CARTESIAN_POINT('',(-0.0219784351231431,0.0194989903199553,0.0254999999979516));
#36050=CARTESIAN_POINT('',(-0.0175,0.0194989903199553,0.0255937499979517));
#36051=CARTESIAN_POINT('',(-0.013021564876857,0.0194989903199553,0.0256874999979516));
#36052=CARTESIAN_POINT('',(-0.00985483303217851,0.0226657221646338,0.0257812499979517));
#36053=CARTESIAN_POINT('',(-0.00668810118750004,0.0258324540093123,0.0258749999979516));
#36054=CARTESIAN_POINT('',(-0.00668810118750004,0.0303108891324553,0.0259687499979517));
#36055=CARTESIAN_POINT('',(-0.00668810118750004,0.0347893242555984,0.0260624999979516));
#36056=CARTESIAN_POINT('',(-0.00985483303217851,0.0379560561002769,0.0261562499979517));
#36057=CARTESIAN_POINT('',(-0.013021564876857,0.0411227879449553,0.0262499999979516));
#36058=CARTESIAN_POINT('',(-0.0175,0.0411227879449554,0.0263437499979517));
#36059=CARTESIAN_POINT('',(-0.0219784351231431,0.0411227879449553,0.0264374999979516));
#36060=CARTESIAN_POINT('',(-0.0251451669678216,0.0379560561002769,0.0265312499979517));
#36061=CARTESIAN_POINT('',(-0.0283118988125,0.0347893242555984,0.0266249999979516));
#36062=CARTESIAN_POINT('',(-0.0283118988125,0.0303108891324553,0.0267187499979517));
#36063=CARTESIAN_POINT('',(-0.0283118988125,0.0258324540093123,0.0268124999979516));
#36064=CARTESIAN_POINT('',(-0.0251451669678216,0.0226657221646338,0.0269062499979516));
#36065=CARTESIAN_POINT('',(-0.0219784351231431,0.0194989903199553,0.0269999999979516));
#36066=CARTESIAN_POINT('',(-0.0175,0.0194989903199553,0.0270937499979516));
#36067=CARTESIAN_POINT('',(-0.013021564876857,0.0194989903199553,0.0271874999979516));
#36068=CARTESIAN_POINT('',(-0.00985483303217851,0.0226657221646338,0.0272812499979516));
#36069=CARTESIAN_POINT('',(-0.00668810118750004,0.0258324540093123,0.0273749999979517));
#36070=CARTESIAN_POINT('',(-0.00668810118750004,0.0303108891324553,0.0274687499979516));
#36071=CARTESIAN_POINT('',(-0.00668810118750004,0.0303108891324553,0.0274687499979516));
#36072=CARTESIAN_POINT('',(-0.00709405059375004,0.0303108891324553,0.0272343749989758));
#36073=CARTESIAN_POINT('',(-0.0075,0.0303108891324553,0.027));
#36074=CARTESIAN_POINT('',(-0.0275,0.0303108891324553,0.02625));
#36075=CARTESIAN_POINT('',(-0.0275000000000001,0.0261687535087244,0.02634375));
#36076=CARTESIAN_POINT('',(-0.0245710678118655,0.0232398213205899,0.0264375));
#36077=CARTESIAN_POINT('',(-0.021642135623731,0.0203108891324553,0.02653125));
#36078=CARTESIAN_POINT('',(-0.0175,0.0203108891324553,0.026625));
#36079=CARTESIAN_POINT('',(-0.0133578643762691,0.0203108891324553,0.02671875));
#36080=CARTESIAN_POINT('',(-0.0104289321881346,0.0232398213205899,0.0268125));
#36081=CARTESIAN_POINT('',(-0.00750000000000004,0.0261687535087243,0.02690625));
#36082=CARTESIAN_POINT('',(-0.0075,0.0303108891324553,0.027));
#36083=CARTESIAN_POINT('',(-0.0275,0.0303108891324553,0.02625));
#36084=CARTESIAN_POINT('',(-0.0075,0.0303108891324553,0.0255));
#36085=CARTESIAN_POINT('',(-0.00750000000000004,0.0344530247561863,0.02559375));
#36086=CARTESIAN_POINT('',(-0.0104289321881346,0.0373819569443208,0.0256875));
#36087=CARTESIAN_POINT('',(-0.0133578643762691,0.0403108891324553,0.02578125));
#36088=CARTESIAN_POINT('',(-0.0175,0.0403108891324553,0.025875));
#36089=CARTESIAN_POINT('',(-0.021642135623731,0.0403108891324553,0.02596875));
#36090=CARTESIAN_POINT('',(-0.0245710678118655,0.0373819569443208,0.0260625));
#36091=CARTESIAN_POINT('',(-0.0275000000000001,0.0344530247561863,0.02615625));
#36092=CARTESIAN_POINT('',(-0.0275,0.0303108891324553,0.02625));
#36093=CARTESIAN_POINT('',(-0.0075,0.0303108891324553,0.0255));
#36094=CARTESIAN_POINT('',(-0.0275,0.0303108891324553,0.02475));
#36095=CARTESIAN_POINT('',(-0.0275000000000001,0.0261687535087244,0.02484375));
#36096=CARTESIAN_POINT('',(-0.0245710678118655,0.0232398213205899,0.0249375));
#36097=CARTESIAN_POINT('',(-0.021642135623731,0.0203108891324553,0.02503125));
#36098=CARTESIAN_POINT('',(-0.0175,0.0203108891324553,0.025125));
#36099=CARTESIAN_POINT('',(-0.0133578643762691,0.0203108891324553,0.02521875));
#36100=CARTESIAN_POINT('',(-0.0104289321881346,0.0232398213205899,0.0253125));
#36101=CARTESIAN_POINT('',(-0.00750000000000004,0.0261687535087243,0.02540625));
#36102=CARTESIAN_POINT('',(-0.0075,0.0303108891324553,0.0255));
#36103=CARTESIAN_POINT('',(-0.0275,0.0303108891324553,0.02475));
#36104=CARTESIAN_POINT('',(-0.0075,0.0303108891324553,0.024));
#36105=CARTESIAN_POINT('',(-0.00750000000000002,0.0344530247561863,0.02409375));
#36106=CARTESIAN_POINT('',(-0.0104289321881346,0.0373819569443208,0.0241875));
#36107=CARTESIAN_POINT('',(-0.0133578643762691,0.0403108891324553,0.02428125));
#36108=CARTESIAN_POINT('',(-0.0175,0.0403108891324553,0.024375));
#36109=CARTESIAN_POINT('',(-0.021642135623731,0.0403108891324553,0.02446875));
#36110=CARTESIAN_POINT('',(-0.0245710678118655,0.0373819569443208,0.0245625));
#36111=CARTESIAN_POINT('',(-0.0275000000000001,0.0344530247561863,0.02465625));
#36112=CARTESIAN_POINT('',(-0.0275,0.0303108891324553,0.02475));
#36113=CARTESIAN_POINT('',(-0.0075,0.0303108891324553,0.024));
#36114=CARTESIAN_POINT('',(-0.0275,0.0303108891324553,0.02325));
#36115=CARTESIAN_POINT('',(-0.0275000000000001,0.0261687535087243,0.02334375));
#36116=CARTESIAN_POINT('',(-0.0245710678118655,0.0232398213205899,0.0234375));
#36117=CARTESIAN_POINT('',(-0.021642135623731,0.0203108891324553,0.02353125));
#36118=CARTESIAN_POINT('',(-0.0175,0.0203108891324553,0.023625));
#36119=CARTESIAN_POINT('',(-0.0133578643762691,0.0203108891324553,0.02371875));
#36120=CARTESIAN_POINT('',(-0.0104289321881346,0.0232398213205899,0.0238125));
#36121=CARTESIAN_POINT('',(-0.00750000000000006,0.0261687535087243,0.02390625));
#36122=CARTESIAN_POINT('',(-0.0075,0.0303108891324553,0.024));
#36123=CARTESIAN_POINT('',(-0.0275,0.0303108891324553,0.02325));
#36124=CARTESIAN_POINT('',(-0.0075,0.0303108891324553,0.0225));
#36125=CARTESIAN_POINT('',(-0.00750000000000005,0.0344530247561863,0.02259375));
#36126=CARTESIAN_POINT('',(-0.0104289321881346,0.0373819569443208,0.0226875));
#36127=CARTESIAN_POINT('',(-0.0133578643762691,0.0403108891324553,0.02278125));
#36128=CARTESIAN_POINT('',(-0.0175,0.0403108891324553,0.022875));
#36129=CARTESIAN_POINT('',(-0.021642135623731,0.0403108891324553,0.02296875));
#36130=CARTESIAN_POINT('',(-0.0245710678118655,0.0373819569443208,0.0230625));
#36131=CARTESIAN_POINT('',(-0.0275000000000001,0.0344530247561863,0.02315625));
#36132=CARTESIAN_POINT('',(-0.0275,0.0303108891324553,0.02325));
#36133=CARTESIAN_POINT('',(-0.0075,0.0303108891324553,0.0225));
#36134=CARTESIAN_POINT('',(-0.0275,0.0303108891324553,0.02175));
#36135=CARTESIAN_POINT('',(-0.0275000000000001,0.0261687535087244,0.02184375));
#36136=CARTESIAN_POINT('',(-0.0245710678118655,0.0232398213205899,0.0219375));
#36137=CARTESIAN_POINT('',(-0.021642135623731,0.0203108891324553,0.02203125));
#36138=CARTESIAN_POINT('',(-0.0175,0.0203108891324553,0.022125));
#36139=CARTESIAN_POINT('',(-0.0133578643762691,0.0203108891324553,0.02221875));
#36140=CARTESIAN_POINT('',(-0.0104289321881346,0.0232398213205899,0.0223125));
#36141=CARTESIAN_POINT('',(-0.00750000000000003,0.0261687535087244,0.0224062500000001));
#36142=CARTESIAN_POINT('',(-0.0075,0.0303108891324553,0.0225));
#36143=CARTESIAN_POINT('',(-0.0275,0.0303108891324553,0.02175));
#36144=CARTESIAN_POINT('',(-0.0075,0.0303108891324553,0.021));
#36145=CARTESIAN_POINT('',(-0.00750000000000004,0.0344530247561863,0.02109375));
#36146=CARTESIAN_POINT('',(-0.0104289321881346,0.0373819569443208,0.0211875));
#36147=CARTESIAN_POINT('',(-0.0133578643762691,0.0403108891324553,0.02128125));
#36148=CARTESIAN_POINT('',(-0.0175,0.0403108891324553,0.021375));
#36149=CARTESIAN_POINT('',(-0.021642135623731,0.0403108891324553,0.02146875));
#36150=CARTESIAN_POINT('',(-0.0245710678118655,0.0373819569443208,0.0215625));
#36151=CARTESIAN_POINT('',(-0.0275000000000001,0.0344530247561862,0.02165625));
#36152=CARTESIAN_POINT('',(-0.0275,0.0303108891324553,0.02175));
#36153=CARTESIAN_POINT('',(-0.0175,0.0303108891324553,0.0227055389329771));
#36154=CARTESIAN_POINT('',(-0.00668810118750004,0.0303108891324553,0.0215624999979517));
#36155=CARTESIAN_POINT('',(-0.00668810118750004,0.0303108891324553,0.0275624999979516));
#36156=CARTESIAN_POINT('',(-0.00668810118750004,0.0303108891324553,0.0275624999979516));
#36157=CARTESIAN_POINT('',(-0.0075,0.0303108891324553,0.0275624999979516));
#36158=CARTESIAN_POINT('',(-0.00668810118750004,0.0303108891324553,0.0275624999979516));
#36159=CARTESIAN_POINT('',(-0.0075,0.0303108891324553,0.0215624999979517));
#36160=CARTESIAN_POINT('',(-0.0175,0.0303108891324553,0.021));
#36161=CARTESIAN_POINT('',(-0.0175,0.0303108891324553,0.021));
#36162=CARTESIAN_POINT('',(-0.0175,0.0303108891324553,0.021));
#36163=CARTESIAN_POINT('',(-0.0295,0.0303108891324553,0.021));
#36164=CARTESIAN_POINT('',(0.0150054713301403,0.0116548629404355,0.0361391701443907));
#36165=CARTESIAN_POINT('',(0.0150031588763673,0.0116578401919889,0.035947934784466));
#36166=CARTESIAN_POINT('',(0.0151539652239554,0.0117751854584953,0.0359394078676464));
#36167=CARTESIAN_POINT('',(0.0147161665958775,0.0120273386973655,0.036148565230682));
#36168=CARTESIAN_POINT('',(0.0147210398289912,0.0120209153897032,0.0359662072084213));
#36169=CARTESIAN_POINT('',(0.0148546185149646,0.0121445710251608,0.0359492170745093));
#36170=CARTESIAN_POINT('',(0.0144133059896117,0.0123886722824512,0.0361546881596415));
#36171=CARTESIAN_POINT('',(0.0144143214096126,0.0123876620823172,0.0359787226980922));
#36172=CARTESIAN_POINT('',(0.0145436629927643,0.0125047669320259,0.0359563064442854));
#36173=CARTESIAN_POINT('',(0.0137806677531994,0.0130887656693854,0.0361714915612611));
#36174=CARTESIAN_POINT('',(0.0137809942375612,0.0130882928088727,0.0360024592325571));
#36175=CARTESIAN_POINT('',(0.0138987058352324,0.0132065284189183,0.0359742968067866));
#36176=CARTESIAN_POINT('',(0.0134509186271344,0.0134275053033658,0.0361831802396108));
#36177=CARTESIAN_POINT('',(0.0134479713569291,0.0134304584458767,0.0360141932545989));
#36178=CARTESIAN_POINT('',(0.013565452208009,0.0135487654179437,0.0359860369724177));
#36179=CARTESIAN_POINT('',(0.0127639622054845,0.0140821297892993,0.0362069676037666));
#36180=CARTESIAN_POINT('',(0.0127608824316598,0.0140849200425824,0.0360380293351662));
#36181=CARTESIAN_POINT('',(0.0128722761287665,0.0142089014121378,0.036009833448151));
#36182=CARTESIAN_POINT('',(0.0124055409164308,0.0143988762317392,0.0362189194690151));
#36183=CARTESIAN_POINT('',(0.0124024061219934,0.0144015785667605,0.0360500306463481));
#36184=CARTESIAN_POINT('',(0.0125105936649424,0.014528289602461,0.0360217950032614));
#36185=CARTESIAN_POINT('',(0.0116714517710063,0.0150000765239135,0.036242673130302));
#36186=CARTESIAN_POINT('',(0.0116681817468594,0.0150026195968398,0.0360738590671113));
#36187=CARTESIAN_POINT('',(0.0117698571779652,0.0151345076388992,0.0360455634085746));
#36188=CARTESIAN_POINT('',(0.0112948641563,0.0152855569023416,0.0362545093019396));
#36189=CARTESIAN_POINT('',(0.0112914933446839,0.0152880478903352,0.0360857214182595));
#36190=CARTESIAN_POINT('',(0.0113898744880696,0.0154223731515779,0.0360574046522466));
#36191=CARTESIAN_POINT('',(0.0101370220428386,0.016097503179033,0.0362900435294723));
#36192=CARTESIAN_POINT('',(0.010133457137473,0.0160997487415128,0.0361212573242105));
#36193=CARTESIAN_POINT('',(0.0102216604240609,0.0162411455678868,0.0360929396859323));
#36194=CARTESIAN_POINT('',(0.00932784277326136,0.0165797177732773,0.0363137944754649));
#36195=CARTESIAN_POINT('',(0.00932402550068061,0.0165818564949476,0.0361448926543703));
#36196=CARTESIAN_POINT('',(0.00940532350498953,0.0167275004883187,0.0361166676303393));
#36197=CARTESIAN_POINT('',(0.00805749908506388,0.0172133852439097,0.0363495830710199));
#36198=CARTESIAN_POINT('',(0.00805365291654553,0.0172151864437042,0.0361805854510368));
#36199=CARTESIAN_POINT('',(0.00812374034472282,0.017366482829951,0.0361524376560477));
#36200=CARTESIAN_POINT('',(0.00762302277337706,0.0174102228500188,0.0363615663698332));
#36201=CARTESIAN_POINT('',(0.00761917539836762,0.0174119074800385,0.0361925640669859));
#36202=CARTESIAN_POINT('',(0.00768540896722212,0.0175649362904097,0.0361644200944729));
#36203=CARTESIAN_POINT('',(0.0067421348108262,0.0177699171096375,0.0363854684767082));
#36204=CARTESIAN_POINT('',(0.00673821226469986,0.0177714051850552,0.0362164741581558));
#36205=CARTESIAN_POINT('',(0.00679670148073716,0.0179275483463163,0.0361883236436059));
#36206=CARTESIAN_POINT('',(0.00629750019405377,0.0179322032679647,0.0363973418696297));
#36207=CARTESIAN_POINT('',(0.00629354409684533,0.0179335927900506,0.0362283581420782));
#36208=CARTESIAN_POINT('',(0.00634812012471546,0.0180911321687717,0.0362001991088505));
#36209=CARTESIAN_POINT('',(0.00495135232263279,0.0183677380514857,0.0364328740623035));
#36210=CARTESIAN_POINT('',(0.00494731728573729,0.0183688244427915,0.0362639076752442));
#36211=CARTESIAN_POINT('',(0.00499004225783576,0.018530121831357,0.0362357348449958));
#36212=CARTESIAN_POINT('',(0.00403766104134308,0.0185899382196955,0.0364564584641844));
#36213=CARTESIAN_POINT('',(0.00403354391352598,0.0185908321653496,0.0362874747700997));
#36214=CARTESIAN_POINT('',(0.00406827840324674,0.0187540564461923,0.0362593158706682));
#36215=CARTESIAN_POINT('',(0.00264279108803299,0.0188212056651329,0.0364919907042367));
#36216=CARTESIAN_POINT('',(0.0026386301707038,0.0188217898732382,0.0363230061665402));
#36217=CARTESIAN_POINT('',(0.00266112044395212,0.0189869921716713,0.0362948477881039));
#36218=CARTESIAN_POINT('',(0.00217376239730524,0.0188812204022797,0.0365038571823142));
#36219=CARTESIAN_POINT('',(0.00216966039829716,0.0188816939766296,0.0363348774179181));
#36220=CARTESIAN_POINT('',(0.00218797198716229,0.0190474033987819,0.0363067152235105));
#36221=CARTESIAN_POINT('',(0.00122736168079795,0.0189662676914545,0.0365276159903745));
#36222=CARTESIAN_POINT('',(0.00122325978210865,0.0189665313786802,0.0363587404620788));
#36223=CARTESIAN_POINT('',(0.00123325939896185,0.0191328317845803,0.0363304939496865));
#36224=CARTESIAN_POINT('',(0.000750109747437154,0.0189910895629562,0.0365395229269734));
#36225=CARTESIAN_POINT('',(0.000746035312959843,0.0189912527062141,0.0363707284949299));
#36226=CARTESIAN_POINT('',(0.000751817144200152,0.0191576547601785,0.0363424168003708));
#36227=CARTESIAN_POINT('',(-0.000670065907784316,0.0190117753343796,0.0365749488927423));
#36228=CARTESIAN_POINT('',(-0.000673874856843052,0.0190116233381809,0.0364063765575926));
#36229=CARTESIAN_POINT('',(-0.000680804354205267,0.0191778946149216,0.0363778877747587));
#36230=CARTESIAN_POINT('',(-0.00160954297810004,0.0189550625967369,0.0365983944775526));
#36231=CARTESIAN_POINT('',(-0.00161373965550082,0.0189547054858199,0.0364299487070827));
#36232=CARTESIAN_POINT('',(-0.00162848218484478,0.019120310475174,0.0364013569929705));
#36233=CARTESIAN_POINT('',(-0.00300799590936611,0.0187662787272906,0.036633876228612));
#36234=CARTESIAN_POINT('',(-0.00301215150832985,0.0187656130285369,0.0364654104309061));
#36235=CARTESIAN_POINT('',(-0.00303913970831725,0.0189295349129496,0.0364368354483491));
#36236=CARTESIAN_POINT('',(-0.00347234573253729,0.0186859927943862,0.0366457512682207));
#36237=CARTESIAN_POINT('',(-0.0034765462939763,0.018685210758763,0.0364772515256066));
#36238=CARTESIAN_POINT('',(-0.00350754249106109,0.0188484660646857,0.0364487036494823));
#36239=CARTESIAN_POINT('',(-0.00439738683072631,0.0184901730835349,0.0366696406146067));
#36240=CARTESIAN_POINT('',(-0.00440155639190949,0.0184891832393428,0.0365010320369736));
#36241=CARTESIAN_POINT('',(-0.00444066149242716,0.0186508142610025,0.0364725717219389));
#36242=CARTESIAN_POINT('',(-0.00485946183245549,0.0183742272060465,0.0366816913984795));
#36243=CARTESIAN_POINT('',(-0.00486362356602114,0.0183731244670117,0.0365130094368909));
#36244=CARTESIAN_POINT('',(-0.00490677393536493,0.0185338153889762,0.0364846080278259));
#36245=CARTESIAN_POINT('',(-0.00623047589763161,0.017974636268116,0.0367178177623487));
#36246=CARTESIAN_POINT('',(-0.00623477555290467,0.0179731625453613,0.0365489393515267));
#36247=CARTESIAN_POINT('',(-0.0062897509041315,0.0181305941503993,0.0365206945255701));
#36248=CARTESIAN_POINT('',(-0.00711376035248052,0.0176430910751536,0.03674150620782));
#36249=CARTESIAN_POINT('',(-0.00711741722307947,0.0176416296124813,0.0365725725693226));
#36250=CARTESIAN_POINT('',(-0.00718068263463432,0.0177959670518017,0.0365443741266795));
#36251=CARTESIAN_POINT('',(-0.00882110726856891,0.0168544449803335,0.0367885120981666));
#36252=CARTESIAN_POINT('',(-0.00882456908118346,0.0168526183525423,0.0366197978000482));
#36253=CARTESIAN_POINT('',(-0.00890266033648855,0.0169997524596937,0.0365914224896071));
#36254=CARTESIAN_POINT('',(-0.00964516470428283,0.0163973397368115,0.0368119386239966));
#36255=CARTESIAN_POINT('',(-0.00964868426798934,0.0163952756846889,0.0366433874886977));
#36256=CARTESIAN_POINT('',(-0.00973372826951099,0.0165382735779742,0.0366148806443442));
#36257=CARTESIAN_POINT('',(-0.0108354707890685,0.015614674538188,0.0368476617333936));
#36258=CARTESIAN_POINT('',(-0.0108388931283578,0.0156122991685692,0.036679173008154));
#36259=CARTESIAN_POINT('',(-0.0109342223730294,0.0157483876887146,0.0366506162690511));
#36260=CARTESIAN_POINT('',(-0.0112248240896321,0.0153371335655903,0.036859675273099));
#36261=CARTESIAN_POINT('',(-0.01122824158708,0.0153346314501312,0.0366911815412776));
#36262=CARTESIAN_POINT('',(-0.0113269189796164,0.015468321592113,0.0366626287034684));
#36263=CARTESIAN_POINT('',(-0.0119750795926056,0.0147587875722466,0.0368835550330791));
#36264=CARTESIAN_POINT('',(-0.0119783813846664,0.014756109998839,0.0367149966242104));
#36265=CARTESIAN_POINT('',(-0.0120836443668111,0.014884773382102,0.0366864959984767));
#36266=CARTESIAN_POINT('',(-0.0123376991914475,0.0144569261127705,0.0368954714669796));
#36267=CARTESIAN_POINT('',(-0.0123409681507439,0.0144541338985067,0.0367268562151948));
#36268=CARTESIAN_POINT('',(-0.0124494054250222,0.014580224628592,0.0366984011330891));
#36269=CARTESIAN_POINT('',(-0.0133887349763937,0.0135139894778297,0.0369311963220453));
#36270=CARTESIAN_POINT('',(-0.013391980180177,0.0135107968379156,0.0367623833297108));
#36271=CARTESIAN_POINT('',(-0.0135095617900217,0.0136289283784537,0.0367340861153028));
#36272=CARTESIAN_POINT('',(-0.0140405295944604,0.0128357666330661,0.0369549874623704));
#36273=CARTESIAN_POINT('',(-0.0140433284392538,0.0128327092039008,0.0367859805271076));
#36274=CARTESIAN_POINT('',(-0.0141670411795076,0.0129447410817698,0.0367578410680902));
#36275=CARTESIAN_POINT('',(-0.0149439782060546,0.0117431196649284,0.0369905594354358));
#36276=CARTESIAN_POINT('',(-0.0149465501818784,0.0117398453202388,0.0368216051756138));
#36277=CARTESIAN_POINT('',(-0.0150780591810504,0.0118422723622672,0.0367934221024625));
#36278=CARTESIAN_POINT('',(-0.0152333218510672,0.0113654199885582,0.0370024373175107));
#36279=CARTESIAN_POINT('',(-0.0152357712602565,0.0113621402906335,0.0368335437749784));
#36280=CARTESIAN_POINT('',(-0.0153697820207074,0.0114611482845017,0.0368053119406504));
#36281=CARTESIAN_POINT('',(-0.0157836614479193,0.0105878655748921,0.0370262155197047));
#36282=CARTESIAN_POINT('',(-0.0157859353279763,0.0105844719750197,0.0368574618914034));
#36283=CARTESIAN_POINT('',(-0.0159246092661184,0.010676551792807,0.0368291173975656));
#36284=CARTESIAN_POINT('',(-0.0160425585467998,0.0101911239560025,0.0370380229775066));
#36285=CARTESIAN_POINT('',(-0.0160447576605073,0.0101876655110854,0.036869346348945));
#36286=CARTESIAN_POINT('',(-0.0161855984644101,0.0102762207197787,0.0368409399653176));
#36287=CARTESIAN_POINT('',(-0.0167717703580097,0.00897766606165621,0.0370733901805091));
#36288=CARTESIAN_POINT('',(-0.016773601611875,0.00897421684756687,0.0369048856237015));
#36289=CARTESIAN_POINT('',(-0.0169207121015404,0.00905184121412537,0.0368763424308858));
#36290=CARTESIAN_POINT('',(-0.0171948593056475,0.008137841358569,0.0370969116729273));
#36291=CARTESIAN_POINT('',(-0.0171967188294503,0.00813389456074387,0.0369284522952958));
#36292=CARTESIAN_POINT('',(-0.0173472535408609,0.00820453899863601,0.0368998711664753));
#36293=CARTESIAN_POINT('',(-0.0177354059733428,0.00683207780183144,0.0371325488546828));
#36294=CARTESIAN_POINT('',(-0.0177369368253014,0.0068281071831255,0.0369639793819681));
#36295=CARTESIAN_POINT('',(-0.0178923121707994,0.00688724367089204,0.0369354876292107));
#36296=CARTESIAN_POINT('',(-0.0178998432688179,0.00638912086206398,0.0371444827328984));
#36297=CARTESIAN_POINT('',(-0.0179012848831722,0.00638507668266705,0.0369758555020377));
#36298=CARTESIAN_POINT('',(-0.0180581382875847,0.00644038769455516,0.0369474100490041));
#36299=CARTESIAN_POINT('',(-0.0181965136995441,0.00548745329097301,0.0371684840151055));
#36300=CARTESIAN_POINT('',(-0.0181977564942562,0.00548333866730378,0.0369997311055984));
#36301=CARTESIAN_POINT('',(-0.0183573102751423,0.00553079228087688,0.03697138665641));
#36302=CARTESIAN_POINT('',(-0.0183288238059416,0.00502779906232661,0.0371805746899094));
#36303=CARTESIAN_POINT('',(-0.0183299512506326,0.00502368414452842,0.0370117539859255));
#36304=CARTESIAN_POINT('',(-0.0184907334703224,0.00506710051140986,0.0369834641380204));
#36305=CARTESIAN_POINT('',(-0.0186705908881364,0.0036479059704665,0.0372164291814345));
#36306=CARTESIAN_POINT('',(-0.0186714379034367,0.00364361154967467,0.0370475001987006));
#36307=CARTESIAN_POINT('',(-0.0188352556230713,0.0036750836839486,0.0370192962198233));
#36308=CARTESIAN_POINT('',(-0.0188278596473151,0.0027196295348313,0.0372398737540957));
#36309=CARTESIAN_POINT('',(-0.0188284295264619,0.00271578388320857,0.0370710611102305));
#36310=CARTESIAN_POINT('',(-0.0189935157205228,0.00273862512585575,0.0370427651063071));
#36311=CARTESIAN_POINT('',(-0.019004411247759,0.000846780273607725,0.0372868546796072));
#36312=CARTESIAN_POINT('',(-0.0190045699896578,0.000842898100617533,0.0371182903933998));
#36313=CARTESIAN_POINT('',(-0.0191708482586001,0.000849305940358859,0.0370897949811809));
#36314=CARTESIAN_POINT('',(-0.0190236362092071,-9.90864261468875E-5,0.0373104525234818));
#36315=CARTESIAN_POINT('',(-0.0190236105305129,-0.000103356945062465,0.0371419877495273));
#36316=CARTESIAN_POINT('',(-0.0191898952974827,-0.000104847364396079,0.0371134111251529));
#36317=CARTESIAN_POINT('',(-0.0189182036402674,-0.00200252934197603,0.0373584378295551));
#36318=CARTESIAN_POINT('',(-0.01891775574234,-0.00200680794040965,0.037189902370063));
#36319=CARTESIAN_POINT('',(-0.0190831294904098,-0.00202494445874197,0.0371613831443892));
#36320=CARTESIAN_POINT('',(-0.0187949378319753,-0.00293848570417647,0.0373822828591816));
#36321=CARTESIAN_POINT('',(-0.0187942194227897,-0.0029429785958604,0.0372135941292793));
#36322=CARTESIAN_POINT('',(-0.018958722724182,-0.00296909208963992,0.0371851970354613));
#36323=CARTESIAN_POINT('',(-0.0184129004148024,-0.00478011345639779,0.0374298727350032));
#36324=CARTESIAN_POINT('',(-0.0184117730522092,-0.00478451749490607,0.0372609113340795));
#36325=CARTESIAN_POINT('',(-0.0185731684945105,-0.00482681154353278,0.0372327333206625));
#36326=CARTESIAN_POINT('',(-0.0181541175259362,-0.00568578481567748,0.0374535194940516));
#36327=CARTESIAN_POINT('',(-0.0181529639024806,-0.00568951455252184,0.0372845076982008));
#36328=CARTESIAN_POINT('',(-0.0183119271885001,-0.00574034356679125,0.0372563723376181));
#36329=CARTESIAN_POINT('',(-0.0176615722557226,-0.00702096136471443,0.037489071103229));
#36330=CARTESIAN_POINT('',(-0.0176600569045193,-0.00702476800508173,0.0373202501340292));
#36331=CARTESIAN_POINT('',(-0.0178145277596478,-0.00708700619075372,0.037291959760207));
#36332=CARTESIAN_POINT('',(-0.0174792538599267,-0.00746327294783377,0.0375009932518153));
#36333=CARTESIAN_POINT('',(-0.0174776502739044,-0.00746703371040129,0.0373322517824091));
#36334=CARTESIAN_POINT('',(-0.0176304145384798,-0.00753310997641051,0.0373038975062605));
#36335=CARTESIAN_POINT('',(-0.0170852874983177,-0.00832572577577798,0.0375246628185486));
#36336=CARTESIAN_POINT('',(-0.0170834939788836,-0.00832940188153098,0.0373560562349849));
#36337=CARTESIAN_POINT('',(-0.0172326351947694,-0.0084029516129172,0.0373275937443767));
#36338=CARTESIAN_POINT('',(-0.0168731413930909,-0.00874750248588951,0.0375364528956926));
#36339=CARTESIAN_POINT('',(-0.0168712372089865,-0.00875117766036781,0.0373679028797414));
#36340=CARTESIAN_POINT('',(-0.0170184658140329,-0.00882833946261563,0.0373393949243217));
#36341=CARTESIAN_POINT('',(-0.0161921413199236,-0.00998505685127267,0.0375718420432244));
#36342=CARTESIAN_POINT('',(-0.0161900056026684,-0.00998850854585282,0.0374033780835406));
#36343=CARTESIAN_POINT('',(-0.0163310925976824,-0.0100765114087224,0.0373748021053271));
#36344=CARTESIAN_POINT('',(-0.0156789682144187,-0.0107732094813255,0.0375954766575031));
#36345=CARTESIAN_POINT('',(-0.015676415516236,-0.0107769012143963,0.0374269646426421));
#36346=CARTESIAN_POINT('',(-0.0158132800581132,-0.0108714680566263,0.0373984255437832));
#36347=CARTESIAN_POINT('',(-0.0145332214666613,-0.0122750788428526,0.0376432225818568));
#36348=CARTESIAN_POINT('',(-0.0145303248317423,-0.0122785300115987,0.0374744753828116));
#36349=CARTESIAN_POINT('',(-0.0146573239782155,-0.012386359365391,0.0374461253942193));
#36350=CARTESIAN_POINT('',(-0.0138956162084445,-0.0129924510713994,0.0376674711168235));
#36351=CARTESIAN_POINT('',(-0.0138928048172763,-0.0129954634359944,0.0374985473407757));
#36352=CARTESIAN_POINT('',(-0.014014094807802,-0.0131099718199376,0.0374703408547971));
#36353=CARTESIAN_POINT('',(-0.012538686354179,-0.0143064069271994,0.0377148389024716));
#36354=CARTESIAN_POINT('',(-0.0125356171246053,-0.0143090890041745,0.0375459982972597));
#36355=CARTESIAN_POINT('',(-0.0126449003590129,-0.01443499193813,0.0375177238513366));
#36356=CARTESIAN_POINT('',(-0.0118162120710391,-0.014908521985929,0.0377381964997738));
#36357=CARTESIAN_POINT('',(-0.011813116889813,-0.0149109891050472,0.0375695350497656));
#36358=CARTESIAN_POINT('',(-0.0119158089831625,-0.0150420366104124,0.0375411171558609));
#36359=CARTESIAN_POINT('',(-0.0106670601049956,-0.0157300843161944,0.03777353081355));
#36360=CARTESIAN_POINT('',(-0.0106636458051717,-0.0157323982000827,0.0376050107567335));
#36361=CARTESIAN_POINT('',(-0.0107562893339342,-0.0158703711407046,0.0375764789793572));
#36362=CARTESIAN_POINT('',(-0.0102730580316003,-0.0159902811627692,0.0377853551568641));
#36363=CARTESIAN_POINT('',(-0.0102695363870165,-0.0159925438324983,0.0376168629961018));
#36364=CARTESIAN_POINT('',(-0.010358752975961,-0.0161327200913,0.0375883087565455));
#36365=CARTESIAN_POINT('',(-0.00946269352699932,-0.0164827862996255,0.0378091861102951));
#36366=CARTESIAN_POINT('',(-0.00945905047971319,-0.0164848780244409,0.0376406911606725));
#36367=CARTESIAN_POINT('',(-0.00954116381799984,-0.0166293341277074,0.0376121395168345));
#36368=CARTESIAN_POINT('',(-0.00904482220411608,-0.0167157459689924,0.0378212343357241));
#36369=CARTESIAN_POINT('',(-0.00904106866268619,-0.0167177754852218,0.0376527111427666));
#36370=CARTESIAN_POINT('',(-0.00911958859647621,-0.0168642565158397,0.0376241820375386));
#36371=CARTESIAN_POINT('',(-0.00777683698870974,-0.0173614715524598,0.0378571713220989));
#36372=CARTESIAN_POINT('',(-0.00777276210631457,-0.0173633105843053,0.0376884999982028));
#36373=CARTESIAN_POINT('',(-0.00784040585450888,-0.0175154685207172,0.0376600892872526));
#36374=CARTESIAN_POINT('',(-0.00690784591584773,-0.0177247307802204,0.0378810100035085));
#36375=CARTESIAN_POINT('',(-0.00690373178108501,-0.0177263240799465,0.0377121389206075));
#36376=CARTESIAN_POINT('',(-0.00696379007350073,-0.0178818959862885,0.0376838892450103));
#36377=CARTESIAN_POINT('',(-0.00512374411469783,-0.0183202528005343,0.0379284549751914));
#36378=CARTESIAN_POINT('',(-0.00511953167638094,-0.01832143877845,0.0377594348084143));
#36379=CARTESIAN_POINT('',(-0.00516398405082556,-0.0184823260981536,0.037731304237429));
#36380=CARTESIAN_POINT('',(-0.0042086343984728,-0.018552526833146,0.0379519491088865));
#36381=CARTESIAN_POINT('',(-0.00420489696214683,-0.0185533920251016,0.0377830608406211));
#36382=CARTESIAN_POINT('',(-0.00424076685047704,-0.0187162358287406,0.0377548258401882));
#36383=CARTESIAN_POINT('',(-0.00233039814015239,-0.0188806276353035,0.0379995291145493));
#36384=CARTESIAN_POINT('',(-0.00232659312175988,-0.0188810801521881,0.0378309289691186));
#36385=CARTESIAN_POINT('',(-0.00234593999503727,-0.0190464021372848,0.0378024624662963));
#36386=CARTESIAN_POINT('',(-0.00138918386749588,-0.0189724749457313,0.0380230950232191));
#36387=CARTESIAN_POINT('',(-0.00138498020199089,-0.0189727818803281,0.037854613968655));
#36388=CARTESIAN_POINT('',(-0.00139644988445051,-0.0191386865299805,0.0378260505551503));
#36389=CARTESIAN_POINT('',(0.000491394329291348,-0.0190169179678846,0.0380703932917064));
#36390=CARTESIAN_POINT('',(0.000495637576888113,-0.0190168106419338,0.0379018852344002));
#36391=CARTESIAN_POINT('',(0.000500614389251542,-0.0191830655857678,0.037873344175741));
#36392=CARTESIAN_POINT('',(0.00143175034843468,-0.0189696728656897,0.0380941477309837));
#36393=CARTESIAN_POINT('',(0.0014362479032175,-0.0189693191294249,0.0379255097828157));
#36394=CARTESIAN_POINT('',(0.00144920178766854,-0.01913531960882,0.0378970719744518));
#36395=CARTESIAN_POINT('',(0.00284238342400006,-0.0187921647474114,0.0381300899636321));
#36396=CARTESIAN_POINT('',(0.00284662846057186,-0.0187915244138856,0.0379612649815778));
#36397=CARTESIAN_POINT('',(0.0028721631719315,-0.0189560989677983,0.0379329784026332));
#36398=CARTESIAN_POINT('',(0.00331441870834582,-0.0187146954289997,0.0381421650442573));
#36399=CARTESIAN_POINT('',(0.00331857804575343,-0.0187139582770902,0.0379732853469086));
#36400=CARTESIAN_POINT('',(0.00334831904383978,-0.0188778892806443,0.0379450429468843));
#36401=CARTESIAN_POINT('',(0.00424454885795175,-0.0185259008247079,0.0381660293974286));
#36402=CARTESIAN_POINT('',(0.00424864072028103,-0.0185249631732459,0.0379971363307566));
#36403=CARTESIAN_POINT('',(0.00428652689934009,-0.0186872200107699,0.0379689040486078));
#36404=CARTESIAN_POINT('',(0.00470370079483309,-0.0184145889742131,0.0381778419035332));
#36405=CARTESIAN_POINT('',(0.00470768720968842,-0.0184135722921259,0.0380089916051811));
#36406=CARTESIAN_POINT('',(0.00474965416178299,-0.0185747665565142,0.0379807250413738));
#36407=CARTESIAN_POINT('',(0.00606380119694438,-0.0180310251530532,0.0382131547292891));
#36408=CARTESIAN_POINT('',(0.00606749675489961,-0.018029767989791,0.0380444706945485));
#36409=CARTESIAN_POINT('',(0.0061215042945471,-0.0181873072730242,0.0380160711436542));
#36410=CARTESIAN_POINT('',(0.00694748782462672,-0.0177094134570405,0.0382365440826416));
#36411=CARTESIAN_POINT('',(0.0069513148115175,-0.0177079163720193,0.038068014101374));
#36412=CARTESIAN_POINT('',(0.00701278761473244,-0.0178624923287709,0.0380394902056667));
#36413=CARTESIAN_POINT('',(0.00823823532605298,-0.0171275861325818,0.0382720683555505));
#36414=CARTESIAN_POINT('',(0.00824199786134128,-0.0171257761164743,0.0381035828034171));
#36415=CARTESIAN_POINT('',(0.00831467242736803,-0.0172751908127472,0.038075023547654));
#36416=CARTESIAN_POINT('',(0.0086626641886403,-0.0169170087108244,0.0382839795954378));
#36417=CARTESIAN_POINT('',(0.0086664417757708,-0.0169150732813902,0.0381154832438721));
#36418=CARTESIAN_POINT('',(0.00874277095704306,-0.0170626723128832,0.0380869325313221));
#36419=CARTESIAN_POINT('',(0.00949954853666518,-0.0164616375906773,0.0383080094950215));
#36420=CARTESIAN_POINT('',(0.00950323875888994,-0.0164595095632353,0.0381394377811394));
#36421=CARTESIAN_POINT('',(0.00958691185482858,-0.0166031712779041,0.0381109478454699));
#36422=CARTESIAN_POINT('',(0.00990843536764638,-0.0162186992949781,0.0383200270202185));
#36423=CARTESIAN_POINT('',(0.00991210717425925,-0.0162164537967256,0.0381513935373868));
#36424=CARTESIAN_POINT('',(0.00999935496721639,-0.0163580607416676,0.0381229531141535));
#36425=CARTESIAN_POINT('',(0.0110994261007969,-0.0154497874825496,0.0383559010620778));
#36426=CARTESIAN_POINT('',(0.0111031423256522,-0.0154471380416969,0.0381870634441405));
#36427=CARTESIAN_POINT('',(0.0112007117190244,-0.0155823067969157,0.0381587859658031));
#36428=CARTESIAN_POINT('',(0.0118494369587164,-0.0148821057065514,0.0383796746295091));
#36429=CARTESIAN_POINT('',(0.011852646263133,-0.0148795566452164,0.0382106555459431));
#36430=CARTESIAN_POINT('',(0.0119572588280899,-0.0150096152999654,0.0381825259246114));
#36431=CARTESIAN_POINT('',(0.0129092501586493,-0.0139489360514091,0.038415073154031));
#36432=CARTESIAN_POINT('',(0.0129122957065155,-0.0139461160896238,0.0382461342271903));
#36433=CARTESIAN_POINT('',(0.0130260382391751,-0.0140679459369744,0.0382179387953184));
#36434=CARTESIAN_POINT('',(0.0132516089108831,-0.0136242158973507,0.0384268476317155));
#36435=CARTESIAN_POINT('',(0.0132545427144061,-0.0136213651199016,0.0382579736292449));
#36436=CARTESIAN_POINT('',(0.0133712586534689,-0.0137402396292797,0.0382297260369069));
#36437=CARTESIAN_POINT('',(0.0139140780149237,-0.0129469235936279,0.0384504924275424));
#36438=CARTESIAN_POINT('',(0.0139168584048897,-0.01294393237065,0.0382817603825315));
#36439=CARTESIAN_POINT('',(0.0140392380233699,-0.0130567327058869,0.0382533985485152));
#36440=CARTESIAN_POINT('',(0.0142354224239416,-0.0125927827016563,0.0384624126901118));
#36441=CARTESIAN_POINT('',(0.0142381414406254,-0.012589711627674,0.0382937568838186));
#36442=CARTESIAN_POINT('',(0.014363241677094,-0.0126993490720532,0.0382653337823739));
#36443=CARTESIAN_POINT('',(0.0151522276287887,-0.0115026826837114,0.0384980076223509));
#36444=CARTESIAN_POINT('',(0.0151545874552716,-0.0114995531518966,0.0383295152258469));
#36445=CARTESIAN_POINT('',(0.0152876502554025,-0.0115993400969666,0.0383009622830993));
#36446=CARTESIAN_POINT('',(0.0157028445696647,-0.0107380131205138,0.0385215934366976));
#36447=CARTESIAN_POINT('',(0.0157053127628298,-0.0107343885637693,0.0383531321867574));
#36448=CARTESIAN_POINT('',(0.0158428716019425,-0.010827822373824,0.0383245525184931));
#36449=CARTESIAN_POINT('',(0.0166863994512137,-0.00913500556704324,0.0385690398252237));
#36450=CARTESIAN_POINT('',(0.0166885267815842,-0.00913114013625447,0.0384004187286762));
#36451=CARTESIAN_POINT('',(0.0168347853906698,-0.00921061383527548,0.0383719678507318));
#36452=CARTESIAN_POINT('',(0.0171193431567698,-0.00829667109200794,0.0385928971779095));
#36453=CARTESIAN_POINT('',(0.0171212465033512,-0.00829272483889006,0.0384240949560577));
#36454=CARTESIAN_POINT('',(0.0172714888685827,-0.00836491513506412,0.0383957899260171));
#36455=CARTESIAN_POINT('',(0.0176771319563529,-0.00698181001816414,0.0386288991507295));
#36456=CARTESIAN_POINT('',(0.0176786906208708,-0.00697786552822998,0.0384599999960005));
#36457=CARTESIAN_POINT('',(0.0178339126296295,-0.00703845721684935,0.0384317728072497));
#36458=CARTESIAN_POINT('',(0.0178464393626524,-0.00653667127314852,0.0386408395226));
#36459=CARTESIAN_POINT('',(0.0178478625413834,-0.00653278908310416,0.0384719535535284));
#36460=CARTESIAN_POINT('',(0.0180045668908952,-0.00658938096130684,0.0384437158153504));
#36461=CARTESIAN_POINT('',(0.0181494253443772,-0.00564108402055084,0.0386644913397127));
#36462=CARTESIAN_POINT('',(0.0181506465751278,-0.00563714975327069,0.038495697562868));
#36463=CARTESIAN_POINT('',(0.018309872103834,-0.00568584827677441,0.0384673853426935));
#36464=CARTESIAN_POINT('',(0.0182836395517567,-0.00518939017263809,0.0386762445560239));
#36465=CARTESIAN_POINT('',(0.0182847605137434,-0.00518544719602479,0.0385075191395397));
#36466=CARTESIAN_POINT('',(0.0184450696221258,-0.005230143102191,0.0384791520040357));
#36467=CARTESIAN_POINT('',(0.0186352161966197,-0.00382278691467086,0.0387114894144686));
#36468=CARTESIAN_POINT('',(0.0186359845944907,-0.00381897190788193,0.0385429418061745));
#36469=CARTESIAN_POINT('',(0.0187991701429938,-0.00385143102407525,0.0385144330338758));
#36470=CARTESIAN_POINT('',(0.0188017960362101,-0.0028964201027731,0.0387349811818274));
#36471=CARTESIAN_POINT('',(0.0188024454149778,-0.0028921752332426,0.0385665207905428));
#36472=CARTESIAN_POINT('',(0.018966882805175,-0.00291689698104377,0.0385379405990861));
#36473=CARTESIAN_POINT('',(0.0189479153503385,-0.00148347557315803,0.0387707536733621));
#36474=CARTESIAN_POINT('',(0.0189482467385373,-0.00147925369912812,0.0386022240958527));
#36475=CARTESIAN_POINT('',(0.0191139948493069,-0.0014915431171492,0.0385737003077644));
#36476=CARTESIAN_POINT('',(0.0189792661299307,-0.00100653752197626,0.038782814865168));
#36477=CARTESIAN_POINT('',(0.0189794916596513,-0.001002251562758,0.0386142366077066));
#36478=CARTESIAN_POINT('',(0.0191455543189113,-0.00101042246271182,0.0385857517789344));
#36479=CARTESIAN_POINT('',(0.0190058525312823,-5.68346111770116E-5,0.0388068420499248));
#36480=CARTESIAN_POINT('',(0.0190058674042672,-5.25318559422445E-5,0.0386381350600849));
#36481=CARTESIAN_POINT('',(0.0191722756290578,-5.23957056172181E-5,0.038609753788149));
#36482=CARTESIAN_POINT('',(0.0190012916831888,0.000415945346046065,0.0388188083349403));
#36483=CARTESIAN_POINT('',(0.0190011954646666,0.00042025103815367,0.0386500229389775));
#36484=CARTESIAN_POINT('',(0.019167642261252,0.000424526058990718,0.0386217047075898));
#36485=CARTESIAN_POINT('',(0.0189353110941103,0.00182821727683686,0.0388545731395467));
#36486=CARTESIAN_POINT('',(0.018934890195968,0.00183273174670508,0.0386855956068839));
#36487=CARTESIAN_POINT('',(0.019100944459924,0.00184915730125414,0.0386574305714316));
#36488=CARTESIAN_POINT('',(0.0188218749463008,0.00276167625899422,0.0388781470791831));
#36489=CARTESIAN_POINT('',(0.0188213246428188,0.00276552616071793,0.0387091476577289));
#36490=CARTESIAN_POINT('',(0.0189862822059325,0.00279074695963414,0.0386810023014141));
#36491=CARTESIAN_POINT('',(0.0185472934983701,0.00414974239546678,0.0389134831899818));
#36492=CARTESIAN_POINT('',(0.0185463978178042,0.00415373650031088,0.038744683372103));
#36493=CARTESIAN_POINT('',(0.0187087218937265,0.00419085004648558,0.0387163759892953));
#36494=CARTESIAN_POINT('',(0.0184382916390242,0.00461040202404379,0.0389252797588995));
#36495=CARTESIAN_POINT('',(0.0184373014075557,0.00461437039626621,0.0387565586044812));
#36496=CARTESIAN_POINT('',(0.018598559234186,0.00465549550858827,0.0387281879997201));
#36497=CARTESIAN_POINT('',(0.0181844048677269,0.00552755144667211,0.0389490404383303));
#36498=CARTESIAN_POINT('',(0.0181832126536465,0.00553146714312297,0.0387804504254259));
#36499=CARTESIAN_POINT('',(0.0183420680926315,0.00558057318884372,0.0387519746590418));
#36500=CARTESIAN_POINT('',(0.0180399541591308,0.00598194757027819,0.0389609521020994));
#36501=CARTESIAN_POINT('',(0.0180386500163758,0.00598588330045647,0.0387924150945185));
#36502=CARTESIAN_POINT('',(0.0181961788428216,0.00603889409903781,0.0387638967209641));
#36503=CARTESIAN_POINT('',(0.0175600527577911,0.00731704300465663,0.0389965132793485));
#36504=CARTESIAN_POINT('',(0.0175584774699178,0.00732081044190295,0.0388280482386248));
#36505=CARTESIAN_POINT('',(0.0177116499128679,0.00738553362907206,0.0387994730817159));
#36506=CARTESIAN_POINT('',(0.017176600931976,0.00817618649942297,0.0390201720001328));
#36507=CARTESIAN_POINT('',(0.0171746560250469,0.00818024084845669,0.0388516453823604));
#36508=CARTESIAN_POINT('',(0.0173246945182605,0.00825213319926071,0.0388231180125633));
#36509=CARTESIAN_POINT('',(0.0165075720298665,0.00941920787493285,0.0390558582625029));
#36510=CARTESIAN_POINT('',(0.0165054454097937,0.00942293852162265,0.0388871453891533));
#36511=CARTESIAN_POINT('',(0.0166496672349242,0.00950596673263848,0.0388587687948336));
#36512=CARTESIAN_POINT('',(0.0162688557302333,0.00982590126449492,0.0390677822215656));
#36513=CARTESIAN_POINT('',(0.0162666412000637,0.00982956491781396,0.0388989998022133));
#36514=CARTESIAN_POINT('',(0.0164088235359054,0.00991619979799271,0.0388706791571233));
#36515=CARTESIAN_POINT('',(0.0157594566755032,0.0106237247575267,0.0390916827747241));
#36516=CARTESIAN_POINT('',(0.0157570704482312,0.010627266788554,0.0389228038988642));
#36517=CARTESIAN_POINT('',(0.0158948546840466,0.0107209302791126,0.0388945605424311));
#36518=CARTESIAN_POINT('',(0.0154875468403251,0.0110164331272623,0.039103700532307));
#36519=CARTESIAN_POINT('',(0.0154851324209757,0.0110198284626436,0.038934798802496));
#36520=CARTESIAN_POINT('',(0.0156204878405909,0.0111170111446627,0.0389065739056364));
#36521=CARTESIAN_POINT('',(0.01463225995395,0.0121573267026454,0.0391394336004382));
#36522=CARTESIAN_POINT('',(0.0146296726940152,0.0121604286682179,0.0389706139625599));
#36523=CARTESIAN_POINT('',(0.0147573523537256,0.0122675988502235,0.0389423227946196));
#36524=CARTESIAN_POINT('',(0.0140116166276898,0.0128669651519896,0.0391628479121368));
#36525=CARTESIAN_POINT('',(0.014008934229898,0.0128699010213118,0.0389942080391084));
#36526=CARTESIAN_POINT('',(0.0141309339335042,0.0129831580760785,0.0389657727502402));
#36527=CARTESIAN_POINT('',(0.012672679814133,0.0141875783371347,0.0392099060817211));
#36528=CARTESIAN_POINT('',(0.0126696949858274,0.0141902322562065,0.0390414338041929));
#36529=CARTESIAN_POINT('',(0.0127797951853403,0.0143148573607752,0.0390128645733509));
#36530=CARTESIAN_POINT('',(0.0119543874113125,0.0147985541865073,0.0392335494260721));
#36531=CARTESIAN_POINT('',(0.0119509078822839,0.0148013492768455,0.0390650749354725));
#36532=CARTESIAN_POINT('',(0.012055068200747,0.014931008420279,0.0390365056751324));
#36533=CARTESIAN_POINT('',(0.0108011721063,0.0156384406904196,0.0392695930882427));
#36534=CARTESIAN_POINT('',(0.0107976455557038,0.0156408785488082,0.0391009499668969));
#36535=CARTESIAN_POINT('',(0.010891641938822,0.0157781079937479,0.0390725173883642));
#36536=CARTESIAN_POINT('',(0.0104050549928709,0.0159046738736348,0.0392816670826779));
#36537=CARTESIAN_POINT('',(0.0104014461052566,0.0159070323820953,0.0391129496189465));
#36538=CARTESIAN_POINT('',(0.0104920332148233,0.0160466424796337,0.0390845767324489));
#36539=CARTESIAN_POINT('',(0.00960060432550017,0.0164028112534571,0.0393056145314552));
#36540=CARTESIAN_POINT('',(0.00959688329125498,0.0164049915851909,0.0391367542902623));
#36541=CARTESIAN_POINT('',(0.00968049362552568,0.0165490736695186,0.0391084961636348));
#36542=CARTESIAN_POINT('',(0.00919077016220187,0.0166358376692505,0.0393175351290205));
#36543=CARTESIAN_POINT('',(0.00918704062898051,0.0166378968498416,0.0391486055828836));
#36544=CARTESIAN_POINT('',(0.00926704844523166,0.0167841022166925,0.0391204033728952));
#36545=CARTESIAN_POINT('',(0.00793881728687105,0.0172875846957858,0.0393531118455946));
#36546=CARTESIAN_POINT('',(0.00793487961528051,0.0172893992463166,0.0391840956119047));
#36547=CARTESIAN_POINT('',(0.00800402716637696,0.0174413142009149,0.039155961915177));
#36548=CARTESIAN_POINT('',(0.00707437008646464,0.017659234549578,0.0393765064409228));
#36549=CARTESIAN_POINT('',(0.00707080832974097,0.0176606790938871,0.039207641159205));
#36550=CARTESIAN_POINT('',(0.007131844103949,0.0178158234315231,0.0391793875957313));
#36551=CARTESIAN_POINT('',(0.005732249994112,0.0181208479176423,0.0394119261070158));
#36552=CARTESIAN_POINT('',(0.00572835454355227,0.0181220780387678,0.0392432790471558));
#36553=CARTESIAN_POINT('',(0.00577777163514192,0.0182809051014134,0.0392148490066115));
#36554=CARTESIAN_POINT('',(0.00527545652035367,0.0182591268759004,0.0394238350568987));
#36555=CARTESIAN_POINT('',(0.00527149473368085,0.0182602728773766,0.0392552533782693));
#36556=CARTESIAN_POINT('',(0.00531692029397464,0.0184202071183902,0.0392267708015014));
#36557=CARTESIAN_POINT('',(0.00435539353041513,0.018500181160291,0.0394476409160019));
#36558=CARTESIAN_POINT('',(0.00435136851956518,0.0185011277015551,0.0392791386244272));
#36559=CARTESIAN_POINT('',(0.00438871216218091,0.0186630486100609,0.0392505926666229));
#36560=CARTESIAN_POINT('',(0.00389346521987264,0.0186027756405381,0.039459504480206));
#36561=CARTESIAN_POINT('',(0.00388935165258131,0.0186036364179546,0.0392910186220323));
#36562=CARTESIAN_POINT('',(0.00392270794497542,0.0187664061473219,0.0392624593799105));
#36563=CARTESIAN_POINT('',(0.0025021362129001,0.0188581188397552,0.0394950907033245));
#36564=CARTESIAN_POINT('',(0.0024979024578147,0.0188586841465867,0.039326569989871));
#36565=CARTESIAN_POINT('',(0.00251913145143705,0.0190236684794769,0.0392980390079921));
#36566=CARTESIAN_POINT('',(0.00156722162533421,0.0189587090116307,0.0395188250839918));
#36567=CARTESIAN_POINT('',(0.00156273541928549,0.0189590661812377,0.0393501647798695));
#36568=CARTESIAN_POINT('',(0.0015760199744932,0.0191250631597236,0.0393217450128133));
#36569=CARTESIAN_POINT('',(0.000153819308255418,0.019005224212649,0.039554568327384));
#36570=CARTESIAN_POINT('',(0.000149530859344075,0.01900526053676,0.0393857282248346));
#36571=CARTESIAN_POINT('',(0.000150241301015367,0.0191718195442531,0.0393574537845495));
#36572=CARTESIAN_POINT('',(-0.000319160762607007,0.0190032637954438,0.0395665019919062));
#36573=CARTESIAN_POINT('',(-0.000323370020041294,0.019003192852083,0.0393976124045188));
#36574=CARTESIAN_POINT('',(-0.000326875348561001,0.0191697739060299,0.039369377919062));
#36575=CARTESIAN_POINT('',(-0.00126890586194998,0.018963538076665,0.0395903822535847));
#36576=CARTESIAN_POINT('',(-0.00127308020914811,0.0189632583539193,0.0394214973160597));
#36577=CARTESIAN_POINT('',(-0.00128490540974052,0.0191294501530534,0.0393932584593037));
#36578=CARTESIAN_POINT('',(-0.00174506512229052,0.0189256111751952,0.0396023189675094));
#36579=CARTESIAN_POINT('',(-0.00174915643471746,0.0189252355786291,0.0394334832095891));
#36580=CARTESIAN_POINT('',(-0.00176521655921334,0.0190910107260413,0.0394052049194109));
#36581=CARTESIAN_POINT('',(-0.00315527515090238,0.018760071462149,0.039637791882901));
#36582=CARTESIAN_POINT('',(-0.003159109299956,0.0187594121399547,0.0394691299482635));
#36583=CARTESIAN_POINT('',(-0.00318770175369042,0.0189234555223965,0.0394407127252026));
#36584=CARTESIAN_POINT('',(-0.00407912829785893,0.018580793512523,0.0396612080344229));
#36585=CARTESIAN_POINT('',(-0.00408316786564095,0.018579909525709,0.0394926925719882));
#36586=CARTESIAN_POINT('',(-0.00411956712144044,0.0187422127576033,0.039464156958556));
#36587=CARTESIAN_POINT('',(-0.00544090513770603,0.0182103774010545,0.0396966359311057));
#36588=CARTESIAN_POINT('',(-0.00544491365088278,0.0182091796481191,0.0395281488885336));
#36589=CARTESIAN_POINT('',(-0.00549317019086339,0.0183681706275683,0.0394995908528479));
#36590=CARTESIAN_POINT('',(-0.0058908137160072,0.0180699183671704,0.0397084917546821));
#36591=CARTESIAN_POINT('',(-0.00589485530925784,0.0180685997080032,0.0395399883854288));
#36592=CARTESIAN_POINT('',(-0.00594698956526464,0.0182263848992081,0.0395114433292663));
#36593=CARTESIAN_POINT('',(-0.00678246751915138,0.0177544859228465,0.0397323568648656));
#36594=CARTESIAN_POINT('',(-0.00678645328451132,0.0177529647917131,0.0395637699716895));
#36595=CARTESIAN_POINT('',(-0.00684640658568973,0.0179080488318765,0.0395352922314537));
#36596=CARTESIAN_POINT('',(-0.00722571835368339,0.017578833949069,0.0397444079220017));
#36597=CARTESIAN_POINT('',(-0.00722970204839152,0.0175771942536395,0.0395757558710103));
#36598=CARTESIAN_POINT('',(-0.00729352337765429,0.0177308137646229,0.0395473303724816));
#36599=CARTESIAN_POINT('',(-0.00853200419952799,0.0170032508445306,0.0397805349308342));
#36600=CARTESIAN_POINT('',(-0.0085360992930078,0.0170012150729036,0.039611674312779));
#36601=CARTESIAN_POINT('',(-0.00861120340273501,0.0171500754775071,0.0395834152712123));
#36602=CARTESIAN_POINT('',(-0.0093640660238232,0.0165589396761269,0.0398043541347681));
#36603=CARTESIAN_POINT('',(-0.00936760081192483,0.0165569485390271,0.0396353274950174));
#36604=CARTESIAN_POINT('',(-0.00945051414852193,0.016701814789159,0.0396072040025732));
#36605=CARTESIAN_POINT('',(-0.01095333582558,0.0155534128083901,0.0398514625261982));
#36606=CARTESIAN_POINT('',(-0.0109566123383997,0.0155510945355589,0.0396825712046406));
#36607=CARTESIAN_POINT('',(-0.0110533401052372,0.0156869529799877,0.0396543377658962));
#36608=CARTESIAN_POINT('',(-0.0117105392461648,0.0149921946210177,0.039874852741731));
#36609=CARTESIAN_POINT('',(-0.011713637850033,0.0149897904366676,0.0397061581247415));
#36610=CARTESIAN_POINT('',(-0.0118168992740911,0.0151204397263602,0.0396777669570562));
#36611=CARTESIAN_POINT('',(-0.0127884183122455,0.0140599436100801,0.0399104774481127));
#36612=CARTESIAN_POINT('',(-0.0127914607265617,0.0140571744085504,0.0397419455571428));
#36613=CARTESIAN_POINT('',(-0.0129038625355801,0.0141796081141066,0.0397134232557945));
#36614=CARTESIAN_POINT('',(-0.0131379114294796,0.0137338809283803,0.0399224413483593));
#36615=CARTESIAN_POINT('',(-0.0131409305574613,0.0137309932121728,0.0397539429397205));
#36616=CARTESIAN_POINT('',(-0.0132563078073279,0.013850572888493,0.0397253936890723));
#36617=CARTESIAN_POINT('',(-0.0138057031563641,0.0130624179401111,0.0399462274691676));
#36618=CARTESIAN_POINT('',(-0.0138085845594307,0.0130593726890895,0.0397777367289653));
#36619=CARTESIAN_POINT('',(-0.0139297708475482,0.0131730492921678,0.0397491816858674));
#36620=CARTESIAN_POINT('',(-0.0141255775468695,0.0127157202418076,0.0399581004650935));
#36621=CARTESIAN_POINT('',(-0.0141284240212117,0.0127125564928361,0.0397895871103025));
#36622=CARTESIAN_POINT('',(-0.0142523778617903,0.0128232511590351,0.0397610500977433));
#36623=CARTESIAN_POINT('',(-0.0150438981845955,0.0116433266987443,0.0399937332592782));
#36624=CARTESIAN_POINT('',(-0.0150466194918001,0.011639828119222,0.0398250918461492));
#36625=CARTESIAN_POINT('',(-0.0151785812924363,0.0117413244877355,0.0397966572050952));
#36626=CARTESIAN_POINT('',(-0.015601268190893,0.0108855078609694,0.0400175221674402));
#36627=CARTESIAN_POINT('',(-0.0156037502572203,0.0108819389745214,0.0398486971526389));
#36628=CARTESIAN_POINT('',(-0.0157408064102649,0.0109768426249763,0.0398204106081291));
#36629=CARTESIAN_POINT('',(-0.0163539519335297,0.00968357985430214,0.0400532444840827));
#36630=CARTESIAN_POINT('',(-0.0163561069607314,0.00967994124090683,0.0398843442193726));
#36631=CARTESIAN_POINT('',(-0.0164998281064669,0.00976425969374833,0.0398561178725525));
#36632=CARTESIAN_POINT('',(-0.0165915150789842,0.00927083072614016,0.0400651730542086));
#36633=CARTESIAN_POINT('',(-0.0165935289830433,0.0092672292824464,0.039896296072404));
#36634=CARTESIAN_POINT('',(-0.0167393345586793,0.00934782893475484,0.0398680510651776));
#36635=CARTESIAN_POINT('',(-0.0170350195453023,0.00842821357465935,0.0400889840246388));
#36636=CARTESIAN_POINT('',(-0.0170368417118387,0.0084245268980667,0.0399202084076463));
#36637=CARTESIAN_POINT('',(-0.0171863989694787,0.00849767210950886,0.039891881591703));
#36638=CARTESIAN_POINT('',(-0.0172396324978774,0.00800110402734881,0.0401007953333983));
#36639=CARTESIAN_POINT('',(-0.0172413601410088,0.00799738572201798,0.039932089458272));
#36640=CARTESIAN_POINT('',(-0.0173926212073374,0.0080667359571995,0.0399037066132332));
#36641=CARTESIAN_POINT('',(-0.0178034336420264,0.00670284475631644,0.0401361524066879));
#36642=CARTESIAN_POINT('',(-0.0178047945753691,0.00669919133529955,0.0399676203732049));
#36643=CARTESIAN_POINT('',(-0.0179608373997931,0.0067568816351323,0.0399390991282188));
#36644=CARTESIAN_POINT('',(-0.0181128517827389,0.00581485538526614,0.0401596376776761));
#36645=CARTESIAN_POINT('',(-0.0181141665497967,0.00581074175312345,0.0399911802605542));
#36646=CARTESIAN_POINT('',(-0.0182726660690083,0.00586101576834401,0.0399625976310416));
#36647=CARTESIAN_POINT('',(-0.0184777093830138,0.00444929676135907,0.040195251280918));
#36648=CARTESIAN_POINT('',(-0.0184787035275952,0.00444517229375046,0.0400267096747493));
#36649=CARTESIAN_POINT('',(-0.0186404590020018,0.00448342268040512,0.0399981955538656));
#36650=CARTESIAN_POINT('',(-0.0185827164300928,0.00398849194161903,0.0402071825625149));
#36651=CARTESIAN_POINT('',(-0.0185836162437446,0.00398429085242931,0.0400385885567563));
#36652=CARTESIAN_POINT('',(-0.0187463269246786,0.00401856738028491,0.040010116389651));
#36653=CARTESIAN_POINT('',(-0.0187587324938683,0.00305538428239273,0.0402312024082703));
#36654=CARTESIAN_POINT('',(-0.0187594268054271,0.0030511343055048,0.0400624751713173));
#36655=CARTESIAN_POINT('',(-0.0189237939209322,0.00307726697975156,0.0400341101664153));
#36656=CARTESIAN_POINT('',(-0.0188296379468907,0.00258246669485135,0.0402433059287324));
#36657=CARTESIAN_POINT('',(-0.0188302208997272,0.00257820196063475,0.0400744988885604));
#36658=CARTESIAN_POINT('',(-0.0189952883801537,0.00260020132984729,0.0400461980710632));
#36659=CARTESIAN_POINT('',(-0.018987584222582,0.00117014663797905,0.0402792453812985));
#36660=CARTESIAN_POINT('',(-0.0189878766130811,0.00116563546292821,0.0401102538110408));
#36661=CARTESIAN_POINT('',(-0.0191544678476417,0.00117549997084161,0.0400821000667122));
#36662=CARTESIAN_POINT('',(-0.019021886828312,0.000229388592566755,0.04030281238303));
#36663=CARTESIAN_POINT('',(-0.0190219485422196,0.000225513787905416,0.040133827629379));
#36664=CARTESIAN_POINT('',(-0.0191888011910571,0.000226509022047831,0.0401056704327208));
#36665=CARTESIAN_POINT('',(-0.0189515281684091,-0.00165056890722806,0.0403497808792148));
#36666=CARTESIAN_POINT('',(-0.0189511778767747,-0.0016544084517273,0.0401810645284669));
#36667=CARTESIAN_POINT('',(-0.0191170355267067,-0.00166987725288971,0.0401526910770812));
#36668=CARTESIAN_POINT('',(-0.0188464963096979,-0.0025917854637227,0.0403733212216877));
#36669=CARTESIAN_POINT('',(-0.0188459456773645,-0.00259582874536051,0.0402047736177609));
#36670=CARTESIAN_POINT('',(-0.0190106563679482,-0.00261928870902019,0.0401762639310132));
#36671=CARTESIAN_POINT('',(-0.0184926679060761,-0.00446419183693985,0.0404211076161054));
#36672=CARTESIAN_POINT('',(-0.0184917002032655,-0.00446818357577394,0.0402526399957149));
#36673=CARTESIAN_POINT('',(-0.0186531564962856,-0.0045079905629465,0.0402240668619258));
#36674=CARTESIAN_POINT('',(-0.0182479002120906,-0.00537572886801895,0.0404448565103214));
#36675=CARTESIAN_POINT('',(-0.0182466139791819,-0.00538004586951678,0.0402763139845434));
#36676=CARTESIAN_POINT('',(-0.018406104300253,-0.00542747010521316,0.0402477993929647));
#36677=CARTESIAN_POINT('',(-0.0176278853553927,-0.00715136217164255,0.0404924090082616));
#36678=CARTESIAN_POINT('',(-0.0176262006455918,-0.00715555313748112,0.040323620177768));
#36679=CARTESIAN_POINT('',(-0.0177804667049412,-0.00721858680345464,0.0402953035664709));
#36680=CARTESIAN_POINT('',(-0.0172526295359134,-0.00801545626095273,0.0405161760389477));
#36681=CARTESIAN_POINT('',(-0.0172509307221984,-0.00801912986087298,0.040347239024586));
#36682=CARTESIAN_POINT('',(-0.0174018482893674,-0.00809020306586266,0.040319043275123));
#36683=CARTESIAN_POINT('',(-0.0165891310234162,-0.00927501607177101,0.0405518309761127));
#36684=CARTESIAN_POINT('',(-0.0165871113566919,-0.00927862586719968,0.0403830003753058));
#36685=CARTESIAN_POINT('',(-0.016732118837969,-0.00936054912549886,0.0403547177731007));
#36686=CARTESIAN_POINT('',(-0.0163504407096611,-0.0096895664096134,0.0405637668909742));
#36687=CARTESIAN_POINT('',(-0.0163483530307484,-0.00969309279106215,0.0403950016662479));
#36688=CARTESIAN_POINT('',(-0.0164911668339191,-0.00977862891273121,0.040366666560219));
#36689=CARTESIAN_POINT('',(-0.0158470220953076,-0.0104926878976402,0.0405874381582746));
#36690=CARTESIAN_POINT('',(-0.0158447595959533,-0.010496101570109,0.04041879922213));
#36691=CARTESIAN_POINT('',(-0.0159830116902603,-0.01058857535944,0.0403903626650279));
#36692=CARTESIAN_POINT('',(-0.0155815030828519,-0.0108829408412664,0.0405992200571002));
#36693=CARTESIAN_POINT('',(-0.0155791404639051,-0.0108863256057379,0.0404306420263519));
#36694=CARTESIAN_POINT('',(-0.0157150102784006,-0.0109821387006477,0.0404021565358583));
#36695=CARTESIAN_POINT('',(-0.0147443380000451,-0.0120204432381726,0.0406345751477657));
#36696=CARTESIAN_POINT('',(-0.0147417946425176,-0.0120235500482091,0.040466107316148));
#36697=CARTESIAN_POINT('',(-0.014870115139696,-0.0121293123008178,0.0404375344932468));
#36698=CARTESIAN_POINT('',(-0.0141323054150094,-0.012734617153313,0.0406581742442809));
#36699=CARTESIAN_POINT('',(-0.0141292982380388,-0.0127379352802263,0.0404896901080622));
#36700=CARTESIAN_POINT('',(-0.0142525651721741,-0.0128496009415859,0.0404611285718946));
#36701=CARTESIAN_POINT('',(-0.0127993117038726,-0.0140737397407963,0.0407059276861236));
#36702=CARTESIAN_POINT('',(-0.012795989406329,-0.0140767800209882,0.0405372130140451));
#36703=CARTESIAN_POINT('',(-0.0129077330328863,-0.0142002990080325,0.0405088370003867));
#36704=CARTESIAN_POINT('',(-0.0120743866383509,-0.0147009483119556,0.0407301934339938));
#36705=CARTESIAN_POINT('',(-0.0120710300120229,-0.0147036972494881,0.0405612702667684));
#36706=CARTESIAN_POINT('',(-0.0121764415327295,-0.0148329955623863,0.0405330628488529));
#36707=CARTESIAN_POINT('',(-0.0105423258825493,-0.0158356578312777,0.0407782066571403));
#36708=CARTESIAN_POINT('',(-0.0105387562032422,-0.0158380387566235,0.0406091983341337));
#36709=CARTESIAN_POINT('',(-0.0106307531401576,-0.0159773049789665,0.040581058297319));
#36710=CARTESIAN_POINT('',(-0.00973264971430907,-0.016345206458774,0.0408019714360824));
#36711=CARTESIAN_POINT('',(-0.00972934845143041,-0.0163471907527672,0.0406331359711917));
#36712=CARTESIAN_POINT('',(-0.0098137431818835,-0.0164909303385969,0.0406048583516335));
#36713=CARTESIAN_POINT('',(-0.00806537401592001,-0.0172290448552643,0.040849071665102));
#36714=CARTESIAN_POINT('',(-0.00806187747714099,-0.0172306642979756,0.0406805112314068));
#36715=CARTESIAN_POINT('',(-0.00813148945943629,-0.0173818031815893,0.0406520128667242));
#36716=CARTESIAN_POINT('',(-0.00720410797528281,-0.0176065010020934,0.0408725336732333));
#36717=CARTESIAN_POINT('',(-0.00720015555035734,-0.0176081146295931,0.0407040676752542));
#36718=CARTESIAN_POINT('',(-0.00726254823193961,-0.017762253651073,0.0406754920583924));
#36719=CARTESIAN_POINT('',(-0.00587093155877073,-0.0180763429638379,0.0409081137712902));
#36720=CARTESIAN_POINT('',(-0.00586691205994924,-0.0180776491619511,0.0407395938948666));
#36721=CARTESIAN_POINT('',(-0.0059175910359496,-0.0182359248774687,0.0407110623000412));
#36722=CARTESIAN_POINT('',(-0.00541963181038933,-0.018216834715786,0.0409200341480749));
#36723=CARTESIAN_POINT('',(-0.00541552867837081,-0.0182180537864837,0.0407514716238395));
#36724=CARTESIAN_POINT('',(-0.00546231699354845,-0.0183775787376718,0.0407229741499068));
#36725=CARTESIAN_POINT('',(-0.00450289334993954,-0.0184648159346774,0.0409440335352421));
#36726=CARTESIAN_POINT('',(-0.00449872590875717,-0.0184658340544464,0.0407753565497765));
#36727=CARTESIAN_POINT('',(-0.00453751882102838,-0.0186276217911276,0.0407469511301288));
#36728=CARTESIAN_POINT('',(-0.00403695754679052,-0.0185722191308532,0.0409561242729045));
#36729=CARTESIAN_POINT('',(-0.00403276579261126,-0.0185731285420499,0.0407873765694338));
#36730=CARTESIAN_POINT('',(-0.00406749283074953,-0.0187359238531794,0.0407590279987012));
#36731=CARTESIAN_POINT('',(-0.00264132417527466,-0.0188393419555243,0.0409920272199963));
#36732=CARTESIAN_POINT('',(-0.00263689297781954,-0.0188399757678068,0.0408231190853848));
#36733=CARTESIAN_POINT('',(-0.00265961278377104,-0.0190052087860372,0.0407948982614302));
#36734=CARTESIAN_POINT('',(-0.00170611182026073,-0.0189466097837117,0.0410155716589265));
#36735=CARTESIAN_POINT('',(-0.00170222908050555,-0.0189469732330682,0.0408466877375895));
#36736=CARTESIAN_POINT('',(-0.00171619674648011,-0.0191131286454142,0.0408184492137106));
#36737=CARTESIAN_POINT('',(0.000173676291005686,-0.0190224781872767,0.0410625631663291));
#36738=CARTESIAN_POINT('',(0.000177561804452529,-0.0190224283900372,0.0408939239429425));
#36739=CARTESIAN_POINT('',(0.000180075422117499,-0.0191888972842088,0.0408654885305162));
#36740=CARTESIAN_POINT('',(0.00112054509379683,-0.0189908367634547,0.041086146524359));
#36741=CARTESIAN_POINT('',(0.00112470330846933,-0.0189905928322111,0.0409176462158715));
#36742=CARTESIAN_POINT('',(0.00113522074412725,-0.0191565845251325,0.0408890983625158));
#36743=CARTESIAN_POINT('',(0.00301448963456351,-0.0187835128377661,0.041134005321298));
#36744=CARTESIAN_POINT('',(0.00301863139178279,-0.0187828482042093,0.0409655173243587));
#36745=CARTESIAN_POINT('',(0.00304570274636773,-0.0189469427742119,0.0409369603164412));
#36746=CARTESIAN_POINT('',(0.00394221166531097,-0.0186103000822643,0.0411577955127677));
#36747=CARTESIAN_POINT('',(0.0039466673760474,-0.0186093396509136,0.0409891964228946));
#36748=CARTESIAN_POINT('',(0.00398152970205259,-0.0187721087890722,0.0409607271352016));
#36749=CARTESIAN_POINT('',(0.00576061524732153,-0.0181300748464635,0.0412053975508442));
#36750=CARTESIAN_POINT('',(0.00576497305527062,-0.0181287075485317,0.0410365127368558));
#36751=CARTESIAN_POINT('',(0.00581582182420553,-0.0182875225378765,0.041008273159893));
#36752=CARTESIAN_POINT('',(0.00665129567942447,-0.0178230540864072,0.0412291638059619));
#36753=CARTESIAN_POINT('',(0.00665505784648776,-0.0178216596144055,0.0410601325402539));
#36754=CARTESIAN_POINT('',(0.00671426399796193,-0.0179777285045373,0.0410320128311421));
#36755=CARTESIAN_POINT('',(0.00795874306948506,-0.0172593063750968,0.0412648016528986));
#36756=CARTESIAN_POINT('',(0.0079624897360314,-0.01725757706242,0.0410959001265478));
#36757=CARTESIAN_POINT('',(0.00803294542961736,-0.0174085796363617,0.0410676745710227));
#36758=CARTESIAN_POINT('',(0.00839055002517237,-0.0170535400231114,0.0412767285079113));
#36759=CARTESIAN_POINT('',(0.00839421742130898,-0.0170517379264982,0.0411079006699725));
#36760=CARTESIAN_POINT('',(0.00846844394164472,-0.0172008232970993,0.0410796158868639));
#36761=CARTESIAN_POINT('',(0.0092302457670169,-0.0166140639256399,0.0413003785807796));
#36762=CARTESIAN_POINT('',(0.00923381364818658,-0.0166120792976908,0.0411316946468232));
#36763=CARTESIAN_POINT('',(0.00931530390538305,-0.0167571365359391,0.0411032941901137));
#36764=CARTESIAN_POINT('',(0.00963990932261663,-0.0163796754406052,0.0413121493670696));
#36765=CARTESIAN_POINT('',(0.0096434555062509,-0.0163775901268873,0.0411435356216829));
#36766=CARTESIAN_POINT('',(0.00972845586542258,-0.01652052075835,0.0411150787592204));
#36767=CARTESIAN_POINT('',(0.0108389410363852,-0.0156334204306386,0.0413474703331632));
#36768=CARTESIAN_POINT('',(0.0108421950119882,-0.0156311517720273,0.041178994654508));
#36769=CARTESIAN_POINT('',(0.0109377134474799,-0.0157672818803707,0.0411504282304712));
#36770=CARTESIAN_POINT('',(0.0115985132592406,-0.0150786995332378,0.0413710456213849));
#36771=CARTESIAN_POINT('',(0.0116020174110474,-0.0150759907838975,0.0412025738370888));
#36772=CARTESIAN_POINT('',(0.0117037965647246,-0.0152075166331746,0.0411740025318393));
#36773=CARTESIAN_POINT('',(0.013037245328802,-0.0138536249290601,0.0414187558668103));
#36774=CARTESIAN_POINT('',(0.0130404966051281,-0.0138505813276262,0.0412500917664286));
#36775=CARTESIAN_POINT('',(0.0131549586138197,-0.0139715066661794,0.0412216752600993));
#36776=CARTESIAN_POINT('',(0.0137193186319365,-0.0131784541631398,0.0414430267121299));
#36777=CARTESIAN_POINT('',(0.0137222941911337,-0.0131753500627701,0.0412741734181582));
#36778=CARTESIAN_POINT('',(0.0138429835311531,-0.0132903920070307,0.0412459098280563));
#36779=CARTESIAN_POINT('',(0.0149581951487915,-0.0117534571826866,0.0414905424104802));
#36780=CARTESIAN_POINT('',(0.0149608243882024,-0.011750114412885,0.0413216314071093));
#36781=CARTESIAN_POINT('',(0.0150923642333444,-0.0118526683603501,0.0412934130886694));
#36782=CARTESIAN_POINT('',(0.015520688566203,-0.0109997943715279,0.0415139101617592));
#36783=CARTESIAN_POINT('',(0.0155229576784727,-0.0109966158267174,0.0413451631485277));
#36784=CARTESIAN_POINT('',(0.0156594313125402,-0.0110921438850482,0.0413168142304098));
#36785=CARTESIAN_POINT('',(0.0162795889764332,-0.00980799649289466,0.0415492121914758));
#36786=CARTESIAN_POINT('',(0.0162817062626187,-0.00980447906514115,0.0413806424581893));
#36787=CARTESIAN_POINT('',(0.0164245046421128,-0.00988960817174467,0.0413521504341661));
#36788=CARTESIAN_POINT('',(0.0165183582002229,-0.00940047153184422,0.0415610186696038));
#36789=CARTESIAN_POINT('',(0.0165204138835871,-0.00939686076164193,0.0413924953238669));
#36790=CARTESIAN_POINT('',(0.0166652153599872,-0.00947842675338205,0.0413639660176923));
#36791=CARTESIAN_POINT('',(0.0169668815467093,-0.00856445872380873,0.04158481274074));
#36792=CARTESIAN_POINT('',(0.016968759366247,-0.00856073776940504,0.041416327221764));
#36793=CARTESIAN_POINT('',(0.0171174145640933,-0.00863495449719448,0.0413877679181777));
#36794=CARTESIAN_POINT('',(0.017177065864082,-0.00813468948262829,0.0415968345520146));
#36795=CARTESIAN_POINT('',(0.0171788787931287,-0.00813085947155214,0.0414283427704703));
#36796=CARTESIAN_POINT('',(0.0173293372690474,-0.00820137076331004,0.0413997883749501));
#36797=CARTESIAN_POINT('',(0.0177535601601371,-0.00683448318101424,0.0416326921596994));
#36798=CARTESIAN_POINT('',(0.0177551425550477,-0.00683039655157697,0.0414641029034488));
#36799=CARTESIAN_POINT('',(0.0179106526810362,-0.00688967026267464,0.0414356266030977));
#36800=CARTESIAN_POINT('',(0.018069656200551,-0.00594744061890342,0.0416565058932169));
#36801=CARTESIAN_POINT('',(0.018071053086069,-0.00594315201602428,0.041487737925076));
#36802=CARTESIAN_POINT('',(0.0182294850460007,-0.00599484249099837,0.0414594047964829));
#36803=CARTESIAN_POINT('',(0.0185686762479634,-0.00413385867196868,0.0417040557893634));
#36804=CARTESIAN_POINT('',(0.018569665428116,-0.0041294751717134,0.0415350525030694));
#36805=CARTESIAN_POINT('',(0.018732662999263,-0.00416532793544681,0.0415069082292052));
#36806=CARTESIAN_POINT('',(0.0187516269698394,-0.0032072138444847,0.041727668157059));
#36807=CARTESIAN_POINT('',(0.0187522925110488,-0.00320341907381266,0.0415587004547988));
#36808=CARTESIAN_POINT('',(0.0189169160347779,-0.00323052407359695,0.0415305295422462));
#36809=CARTESIAN_POINT('',(0.0189785497013675,-0.00131315874630033,0.041775282469228));
#36810=CARTESIAN_POINT('',(0.0189787976176584,-0.00130933038624944,0.0416065960986041));
#36811=CARTESIAN_POINT('',(0.0191450183683159,-0.00131978865421991,0.0415781986729045));
#36812=CARTESIAN_POINT('',(0.0190196699561884,-0.000369682902736731,0.041798768663557));
#36813=CARTESIAN_POINT('',(0.0190197536794715,-0.000365571149283191,0.0416302401562733));
#36814=CARTESIAN_POINT('',(0.0191860834814799,-0.00036803283829089,0.0416017150620279));
#36815=CARTESIAN_POINT('',(0.0189632035263676,0.00151043791943559,0.0418459668701129));
#36816=CARTESIAN_POINT('',(0.0189628723964422,0.00151456480353777,0.0416774933135412));
#36817=CARTESIAN_POINT('',(0.0191285756981165,0.00152854275765588,0.0416489248534374));
#36818=CARTESIAN_POINT('',(0.0188656035494357,0.00244708229619764,0.041869676770902));
#36819=CARTESIAN_POINT('',(0.0188650082956082,0.00245155860199098,0.0417011164879532));
#36820=CARTESIAN_POINT('',(0.019029988696039,0.00247337433558962,0.0416726161446262));
#36821=CARTESIAN_POINT('',(0.0186125495933428,0.00384679085700881,0.0419056432466697));
#36822=CARTESIAN_POINT('',(0.0186116814547299,0.00385100058683171,0.0417368885715677));
#36823=CARTESIAN_POINT('',(0.0187745695464339,0.00388531336935315,0.0417085455414632));
#36824=CARTESIAN_POINT('',(0.0185098333503103,0.00431405271833229,0.0419177363955599));
#36825=CARTESIAN_POINT('',(0.0185088638003719,0.0043182070784044,0.0417489139784957));
#36826=CARTESIAN_POINT('',(0.0186709077889593,0.00435665613252931,0.0417206255091514));
#36827=CARTESIAN_POINT('',(0.0182715157482693,0.00523227424487254,0.041941661341413));
#36828=CARTESIAN_POINT('',(0.0182703464161454,0.00523636077672844,0.041772765548564));
#36829=CARTESIAN_POINT('',(0.0184303499014007,0.00528286586327708,0.0417445357014452));
#36830=CARTESIAN_POINT('',(0.0181357838983419,0.00568464048515436,0.0419535140553254));
#36831=CARTESIAN_POINT('',(0.0181345455695604,0.00568859447658796,0.0417846212593873));
#36832=CARTESIAN_POINT('',(0.0182933099783667,0.00573914511459434,0.0417563890549324));
#36833=CARTESIAN_POINT('',(0.0176799226482771,0.00702193102801493,0.0419888744003936));
#36834=CARTESIAN_POINT('',(0.0176784448562162,0.0070256238076518,0.0418201020793719));
#36835=CARTESIAN_POINT('',(0.0178329826032857,0.00708796730728556,0.0417917731207448));
#36836=CARTESIAN_POINT('',(0.0173113916908864,0.00788715324152287,0.0420122387595618));
#36837=CARTESIAN_POINT('',(0.0173097335223211,0.00789081251687946,0.0418436408609179));
#36838=CARTESIAN_POINT('',(0.017460819243278,0.00796059517179978,0.0418151717394463));
#36839=CARTESIAN_POINT('',(0.0164441541540594,0.00956458376972509,0.0420595310619518));
#36840=CARTESIAN_POINT('',(0.0164421174582832,0.0095680713322191,0.0418910660817133));
#36841=CARTESIAN_POINT('',(0.0165854185710355,0.00965242605887456,0.0418624909390898));
#36842=CARTESIAN_POINT('',(0.0159408649555386,0.0103817820325783,0.0420836316696311));
#36843=CARTESIAN_POINT('',(0.0159383978648997,0.010385544968291,0.041915133818142));
#36844=CARTESIAN_POINT('',(0.0160775560756277,0.0104766751733535,0.0418865832516409));
#36845=CARTESIAN_POINT('',(0.0148323250115084,0.0119119565334862,0.0421314054120078));
#36846=CARTESIAN_POINT('',(0.0148295044085068,0.0119154922548428,0.0419626612680497));
#36847=CARTESIAN_POINT('',(0.0149591363198844,0.0120201360514607,0.0419343088550291));
#36848=CARTESIAN_POINT('',(0.0142253115705693,0.0126304014464608,0.0421552128021273));
#36849=CARTESIAN_POINT('',(0.0142224595723812,0.012633607676376,0.0419862640682912));
#36850=CARTESIAN_POINT('',(0.0143467869578076,0.0127448697856584,0.0419580774261687));
#36851=CARTESIAN_POINT('',(0.0132364774583089,0.0136388158206757,0.0421907471038048));
#36852=CARTESIAN_POINT('',(0.0132334576479525,0.0136417465358339,0.0420217625471197));
#36853=CARTESIAN_POINT('',(0.0133490796759129,0.0137618674964216,0.041993603964865));
#36854=CARTESIAN_POINT('',(0.0128937599156229,0.01396336454063,0.0422025508615589));
#36855=CARTESIAN_POINT('',(0.0128907415118545,0.0139661539971817,0.0420336077348191));
#36856=CARTESIAN_POINT('',(0.013003246381497,0.0140891303563364,0.0420054159154212));
#36857=CARTESIAN_POINT('',(0.0121815880954904,0.0145888143976149,0.0422262280147507));
#36858=CARTESIAN_POINT('',(0.0121784421451099,0.0145914386973753,0.0420574090145197));
#36859=CARTESIAN_POINT('',(0.0122845861716777,0.0147197644261911,0.0420291170568967));
#36860=CARTESIAN_POINT('',(0.0118105913145593,0.0148907736728587,0.0422381485332703));
#36861=CARTESIAN_POINT('',(0.0118073893680565,0.0148933158527189,0.0420694090337606));
#36862=CARTESIAN_POINT('',(0.0119102049265592,0.0150242021930805,0.0420410531744612));
#36863=CARTESIAN_POINT('',(0.0106734218716814,0.0157473457018157,0.0422736889611043));
#36864=CARTESIAN_POINT('',(0.0106702181203719,0.0157494984225377,0.0421051454901133));
#36865=CARTESIAN_POINT('',(0.01076271558934,0.0158877999445305,0.0420766335422122));
#36866=CARTESIAN_POINT('',(0.00988050851272395,0.0162560718816535,0.0422972091975336));
#36867=CARTESIAN_POINT('',(0.00987683663777725,0.0162582984438685,0.0421287476323781));
#36868=CARTESIAN_POINT('',(0.00996268647807769,0.0164007066453042,0.0421001684059327));
#36869=CARTESIAN_POINT('',(0.00822699946699953,0.017152282683698,0.04234457338802));
#36870=CARTESIAN_POINT('',(0.00822310342235589,0.0171541579220479,0.0421760222602139));
#36871=CARTESIAN_POINT('',(0.00829450940136363,0.0173044330294566,0.0421475155211143));
#36872=CARTESIAN_POINT('',(0.00736640822147979,0.0175397753961563,0.0423684146679046));
#36873=CARTESIAN_POINT('',(0.00736227559279473,0.0175414972662327,0.0421997056878268));
#36874=CARTESIAN_POINT('',(0.00742635462325823,0.0176952661658757,0.0421713251998001));
#36875=CARTESIAN_POINT('',(0.00557485437135022,0.0181886967584633,0.0424165432900864));
#36876=CARTESIAN_POINT('',(0.00557059305018462,0.0181900151580173,0.0422476259115998));
#36877=CARTESIAN_POINT('',(0.00561903875309368,0.0183496257535651,0.0422194125176644));
#36878=CARTESIAN_POINT('',(0.00466249418556595,0.0184430462980749,0.0424402033696721));
#36879=CARTESIAN_POINT('',(0.00465872401835851,0.0184440139348268,0.0422713359950257));
#36880=CARTESIAN_POINT('',(0.00469862095603388,0.018605891838371,0.0422430841271073));
#36881=CARTESIAN_POINT('',(0.00281802077453407,0.0188133879909405,0.0424871885748908));
#36882=CARTESIAN_POINT('',(0.00281417986827133,0.0188139486691576,0.042318570161192));
#36883=CARTESIAN_POINT('',(0.00283785041442192,0.0189787211855483,0.0422901180916585));
#36884=CARTESIAN_POINT('',(0.0018839080918573,0.0189300934702549,0.0425106335656295));
#36885=CARTESIAN_POINT('',(0.00187973838254741,0.0189305086999314,0.0423421439355997));
#36886=CARTESIAN_POINT('',(0.00189551287781105,0.0190960706762482,0.0423135874532213));
#36887=CARTESIAN_POINT('',(0.000464554162843612,0.0190002256974114,0.042546347882846));
#36888=CARTESIAN_POINT('',(0.000460353791048119,0.0190003286426425,0.0423778524092138));
#36889=CARTESIAN_POINT('',(0.000463706370908465,0.0191664584001732,0.0423493011875901));
#36890=CARTESIAN_POINT('',(-1.3603547443907E-5,0.0190059266909682,0.0425583908750204));
#36891=CARTESIAN_POINT('',(-1.78713899531079E-5,0.0190059222927238,0.0423898667183118));
#36892=CARTESIAN_POINT('',(-1.86409425035557E-5,0.0191721206572552,0.0423613383876707));
#36893=CARTESIAN_POINT('',(-0.000962888698749424,0.0189815246962087,0.0425823743588719));
#36894=CARTESIAN_POINT('',(-0.000967165032777534,0.0189813094341095,0.0424137476132222));
#36895=CARTESIAN_POINT('',(-0.000976240535668051,0.0191473772967885,0.0423853018819463));
#36896=CARTESIAN_POINT('',(-0.00143457126590083,0.0189516225437873,0.0425943284623379));
#36897=CARTESIAN_POINT('',(-0.0014388688977218,0.0189512951800986,0.0424256301917518));
#36898=CARTESIAN_POINT('',(-0.00145205322852197,0.0191171736530932,0.0423972418708909));
#36899=CARTESIAN_POINT('',(-0.00284094099793105,0.0188100244891607,0.0426301040963971));
#36900=CARTESIAN_POINT('',(-0.00284545979462405,0.0188093587371052,0.0424611973850735));
#36901=CARTESIAN_POINT('',(-0.0028707299272499,0.0189742158760984,0.042432975391739));
#36902=CARTESIAN_POINT('',(-0.00376699808139046,0.0186467172316367,0.0426537986907363));
#36903=CARTESIAN_POINT('',(-0.00377090364480976,0.01864593864656,0.0424847683690623));
#36904=CARTESIAN_POINT('',(-0.00380486530349046,0.0188093633942862,0.0424566479060653));
#36905=CARTESIAN_POINT('',(-0.00513872791989791,0.0182979796666385,0.0426892045843495));
#36906=CARTESIAN_POINT('',(-0.00514269239735289,0.0182968646407614,0.0425203216200328));
#36907=CARTESIAN_POINT('',(-0.00518846589550756,0.0184570621158076,0.0424920811195789));
#36908=CARTESIAN_POINT('',(-0.00559306625344521,0.0181643680587182,0.0427010104062051));
#36909=CARTESIAN_POINT('',(-0.00559697087728178,0.0181631679712986,0.0425322025701378));
#36910=CARTESIAN_POINT('',(-0.00564672406313777,0.0183220802758641,0.0425039016870662));
#36911=CARTESIAN_POINT('',(-0.0064957694573478,0.0178614567223671,0.04272477133892));
#36912=CARTESIAN_POINT('',(-0.00649960558446819,0.0178600593602805,0.042556107270354));
#36913=CARTESIAN_POINT('',(-0.00655720284798014,0.0180161278563503,0.0425276908777702));
#36914=CARTESIAN_POINT('',(-0.00694126016116529,0.0176930038061895,0.0427366525222747));
#36915=CARTESIAN_POINT('',(-0.00694509541752452,0.0176915006586277,0.0425680564301373));
#36916=CARTESIAN_POINT('',(-0.00700652501390227,0.0178460130912245,0.0425395854091972));
#36917=CARTESIAN_POINT('',(-0.00824820177693959,0.0171423765181543,0.0427721357638053));
#36918=CARTESIAN_POINT('',(-0.008251790548277,0.0171406392387208,0.0426036659013395));
#36919=CARTESIAN_POINT('',(-0.00832471646847662,0.0172900888841845,0.0425750947903131));
#36920=CARTESIAN_POINT('',(-0.00908546781664353,0.0167134730961815,0.0427957318040787));
#36921=CARTESIAN_POINT('',(-0.00908936767614809,0.0167113403149665,0.0426272517131758));
#36922=CARTESIAN_POINT('',(-0.00916921216002814,0.0168572372731341,0.0425986870535596));
#36923=CARTESIAN_POINT('',(-0.0102909999685144,0.0159786356346231,0.0428313901050363));
#36924=CARTESIAN_POINT('',(-0.0102945991898559,0.0159763194692739,0.0426627520459007));
#36925=CARTESIAN_POINT('',(-0.0103852063330003,0.0161158016210226,0.0426343153725058));
#36926=CARTESIAN_POINT('',(-0.010684414992981,0.0157183797799352,0.0428433157318564));
#36927=CARTESIAN_POINT('',(-0.0106879657483226,0.0157159640201062,0.0426746099673093));
#36928=CARTESIAN_POINT('',(-0.0107820427352414,0.0158532295056831,0.0426462276658231));
#36929=CARTESIAN_POINT('',(-0.0114540765240435,0.0151666844639779,0.0428672547991974));
#36930=CARTESIAN_POINT('',(-0.0114575030590412,0.0151640988461154,0.0426984283455806));
#36931=CARTESIAN_POINT('',(-0.0115583793013117,0.0152966179800366,0.0426701429484309));
#36932=CARTESIAN_POINT('',(-0.0118318566377774,0.0148738979658878,0.0428793194454723));
#36933=CARTESIAN_POINT('',(-0.0118351611856566,0.0148712686395132,0.0427104387051855));
#36934=CARTESIAN_POINT('',(-0.0119394263670495,0.0150012189785698,0.0426821971437567));
#36935=CARTESIAN_POINT('',(-0.0129246431482226,0.0139590933902365,0.0429151506839148));
#36936=CARTESIAN_POINT('',(-0.0129277296762079,0.013956235532516,0.0427462529203825));
#36937=CARTESIAN_POINT('',(-0.0130415327640104,0.0140781574671,0.042718023992381));
#36938=CARTESIAN_POINT('',(-0.0135998275021078,0.0133014626056276,0.042938562210487));
#36939=CARTESIAN_POINT('',(-0.013602575516219,0.0132986712873312,0.0427698376504481));
#36940=CARTESIAN_POINT('',(-0.0137223200965974,0.0134144441308818,0.0427414706275737));
#36941=CARTESIAN_POINT('',(-0.0148467549202409,0.0118936152566955,0.0429855619714583));
#36942=CARTESIAN_POINT('',(-0.0148491996917421,0.011890543812061,0.0428170568736124));
#36943=CARTESIAN_POINT('',(-0.0149796173886599,0.0119937802269414,0.0427885140212086));
#36944=CARTESIAN_POINT('',(-0.0154185009886721,0.0111434013612562,0.043009149593558));
#36945=CARTESIAN_POINT('',(-0.0154210574184647,0.0111398501006241,0.0428406940622408));
#36946=CARTESIAN_POINT('',(-0.0155561398607172,0.0112368259946476,0.0428121097777485));
#36947=CARTESIAN_POINT('',(-0.0161957093387957,0.00994612440462015,0.04304515280486));
#36948=CARTESIAN_POINT('',(-0.0161979399841593,0.00994249463749885,0.0428765797355238));
#36949=CARTESIAN_POINT('',(-0.0163399589840616,0.0100289293449728,0.0428480908890324));
#36950=CARTESIAN_POINT('',(-0.0164400593245126,0.00953667116451164,0.0430572012611153));
#36951=CARTESIAN_POINT('',(-0.0164422174803105,0.00953294684637346,0.042888565959774));
#36952=CARTESIAN_POINT('',(-0.0165864061706359,0.00961586280349823,0.0428601269980955));
#36953=CARTESIAN_POINT('',(-0.016894147383795,0.00870697603465936,0.0430811362951355));
#36954=CARTESIAN_POINT('',(-0.0168961245689515,0.0087031443145647,0.0429123604322927));
#36955=CARTESIAN_POINT('',(-0.0170443990829768,0.00877885858332786,0.042884034500655));
#36956=CARTESIAN_POINT('',(-0.0171048065348784,0.00828534182490399,0.0430930647472596));
#36957=CARTESIAN_POINT('',(-0.0171066764884509,0.00828147746536018,0.0429242109612949));
#36958=CARTESIAN_POINT('',(-0.0172568737159689,0.00835351582487844,0.0428959477698145));
#36959=CARTESIAN_POINT('',(-0.017688402759418,0.00700039933326027,0.043128724510894));
#36960=CARTESIAN_POINT('',(-0.0176900583888289,0.0069962481391462,0.0429597124205211));
#36961=CARTESIAN_POINT('',(-0.0178454143940276,0.00705725387080521,0.042931575254563));
#36962=CARTESIAN_POINT('',(-0.0180132271233088,0.00611715943804409,0.0431522198964858));
#36963=CARTESIAN_POINT('',(-0.0180144803111107,0.00611351968480371,0.0429832705912268));
#36964=CARTESIAN_POINT('',(-0.0181727669051138,0.0061661772908184,0.0429550848131308));
#36965=CARTESIAN_POINT('',(-0.0184023284969058,0.00475166324970116,0.0431876550859494));
#36966=CARTESIAN_POINT('',(-0.0184033474459008,0.00474770852564244,0.043018925065945));
#36967=CARTESIAN_POINT('',(-0.018564689450059,0.00478855747754072,0.0429905616050906));
#36968=CARTESIAN_POINT('',(-0.018515972453872,0.0042877361244035,0.0431995615620718));
#36969=CARTESIAN_POINT('',(-0.0185168995642598,0.00428374021123731,0.0430309075356459));
#36970=CARTESIAN_POINT('',(-0.0186791254983124,0.00432051716027729,0.0430024830057629));
#36971=CARTESIAN_POINT('',(-0.0187072033441742,0.00335655478501059,0.0432233179844061));
#36972=CARTESIAN_POINT('',(-0.0187079274872983,0.00335251021259686,0.0430547756581805));
#36973=CARTESIAN_POINT('',(-0.0188716668817317,0.00338110383995676,0.0430262617061117));
#36974=CARTESIAN_POINT('',(-0.0187848419957819,0.00288997040124032,0.0432351521775762));
#36975=CARTESIAN_POINT('',(-0.0187854765891899,0.00288584828394335,0.0430666473531019));
#36976=CARTESIAN_POINT('',(-0.0189498247619837,0.00291040610459593,0.0430381032284253));
#36977=CARTESIAN_POINT('',(-0.0189651462740219,0.00148731224398622,0.0432706566150148));
#36978=CARTESIAN_POINT('',(-0.0189654708666694,0.00148315793899136,0.0431021765175295));
#36979=CARTESIAN_POINT('',(-0.019131318753891,0.00149540950004909,0.0430736132395977));
#36980=CARTESIAN_POINT('',(-0.0190154832834067,0.000548349506278168,0.0432943453252847));
#36981=CARTESIAN_POINT('',(-0.0190155990614365,0.000543835601436554,0.0431257663874186));
#36982=CARTESIAN_POINT('',(-0.0191819768803391,0.000548218567437135,0.0430972810643009));
#36983=CARTESIAN_POINT('',(-0.0189861153355352,-0.000865879544968052,0.0433301138001482));
#36984=CARTESIAN_POINT('',(-0.018985921377837,-0.000870172708024659,0.0431613409049158));
#36985=CARTESIAN_POINT('',(-0.0191522017187679,-0.000878390970992399,0.0431330125099441));
#36986=CARTESIAN_POINT('',(-0.018958776420447,-0.00133825739454921,0.0433420716187868));
#36987=CARTESIAN_POINT('',(-0.018958475476988,-0.00134250478669942,0.0431732337615662));
#36988=CARTESIAN_POINT('',(-0.0191245742056541,-0.00135490145970564,0.0431449577125661));
#36989=CARTESIAN_POINT('',(-0.0188680924290746,-0.00228499984736558,0.0433660434476357));
#36990=CARTESIAN_POINT('',(-0.018867583315166,-0.00228920930196638,0.0431971440969443));
#36991=CARTESIAN_POINT('',(-0.0190329223973134,-0.00230990336534812,0.0431689170616229));
#36992=CARTESIAN_POINT('',(-0.018804704452073,-0.00275806485483265,0.0433780088934093));
#36993=CARTESIAN_POINT('',(-0.0188041057185145,-0.00276215519583305,0.0432091237363117));
#36994=CARTESIAN_POINT('',(-0.0189688397708669,-0.00278708086793507,0.043180885340923));
#36995=CARTESIAN_POINT('',(-0.0185638443092955,-0.00415680280424106,0.0434135137709053));
#36996=CARTESIAN_POINT('',(-0.0185629695552276,-0.0041606564775658,0.0432447642656287));
#36997=CARTESIAN_POINT('',(-0.0187253545087216,-0.00419796417403942,0.0432164170789741));
#36998=CARTESIAN_POINT('',(-0.0183353368812342,-0.00506959719009099,0.0434368961714605));
#36999=CARTESIAN_POINT('',(-0.0183342669764093,-0.00507349342334267,0.0432683174256558));
#37000=CARTESIAN_POINT('',(-0.0184944243935023,-0.00511864724285449,0.0432398328593739));
#37001=CARTESIAN_POINT('',(-0.0178923697591036,-0.00640971551303542,0.0434722602728136));
#37002=CARTESIAN_POINT('',(-0.0178909687343637,-0.00641362442053553,0.043303769684843));
#37003=CARTESIAN_POINT('',(-0.018047139167788,-0.00647035981594991,0.0432752143871632));
#37004=CARTESIAN_POINT('',(-0.0177279437193191,-0.00685155606459969,0.043484092904052));
#37005=CARTESIAN_POINT('',(-0.0177264219885323,-0.00685549210929144,0.0433156079658385));
#37006=CARTESIAN_POINT('',(-0.0178811548515406,-0.00691602627884074,0.0432870480313056));
#37007=CARTESIAN_POINT('',(-0.0173649907948434,-0.00772534165695619,0.0435079218054287));
#37008=CARTESIAN_POINT('',(-0.0173632699341338,-0.00772921190972498,0.0433393911381997));
#37009=CARTESIAN_POINT('',(-0.0175148451097775,-0.00779739418046767,0.0433108682260294));
#37010=CARTESIAN_POINT('',(-0.017165602484246,-0.00815893710550448,0.0435199651766935));
#37011=CARTESIAN_POINT('',(-0.0171637581683695,-0.00816281321507147,0.043351385511468));
#37012=CARTESIAN_POINT('',(-0.0173136504702881,-0.00823476080683952,0.0433229018136475));
#37013=CARTESIAN_POINT('',(-0.0165210940987345,-0.009431760341298,0.043556046947235));
#37014=CARTESIAN_POINT('',(-0.0165188567241586,-0.00943571101744704,0.0433872789874135));
#37015=CARTESIAN_POINT('',(-0.0166633643727174,-0.00951867007146015,0.0433589456373712));
#37016=CARTESIAN_POINT('',(-0.0160329494926047,-0.0102385897110408,0.0435799136272656));
#37017=CARTESIAN_POINT('',(-0.0160306646401609,-0.0102421644523927,0.0434109413536699));
#37018=CARTESIAN_POINT('',(-0.0161709217927998,-0.0103325643479168,0.0433827738611434));
#37019=CARTESIAN_POINT('',(-0.0149436602822656,-0.0117716271632975,0.0436271814331457));
#37020=CARTESIAN_POINT('',(-0.0149410707316043,-0.0117749125269769,0.043458203402268));
#37021=CARTESIAN_POINT('',(-0.0150717262175193,-0.0118787143429182,0.0434300391083153));
#37022=CARTESIAN_POINT('',(-0.0143425139356339,-0.0124978339573583,0.0436505840409847));
#37023=CARTESIAN_POINT('',(-0.0143399871796448,-0.0125007572524888,0.0434817939080769));
#37024=CARTESIAN_POINT('',(-0.0144649508075557,-0.0126109912636555,0.0434534797499));
#37025=CARTESIAN_POINT('',(-0.013353254765621,-0.0135246618097943,0.043686185188991));
#37026=CARTESIAN_POINT('',(-0.0133503403783537,-0.0135275366571819,0.0435175966304388));
#37027=CARTESIAN_POINT('',(-0.0134666009456983,-0.013646403549451,0.0434891196980371));
#37028=CARTESIAN_POINT('',(-0.0130091106488293,-0.013855939438497,0.0436981192445647));
#37029=CARTESIAN_POINT('',(-0.0130060880561487,-0.0138587784869067,0.0435295834038134));
#37030=CARTESIAN_POINT('',(-0.0131193165195436,-0.0139804517481268,0.0435010640960348));
#37031=CARTESIAN_POINT('',(-0.0123030784965075,-0.014486486016476,0.0437218476773994));
#37032=CARTESIAN_POINT('',(-0.0122999076233398,-0.0144891782747915,0.0435533603286156));
#37033=CARTESIAN_POINT('',(-0.0124068999056232,-0.0146162992716977,0.0435248024699253));
#37034=CARTESIAN_POINT('',(-0.011939825755397,-0.0147872234611433,0.0437336919390996));
#37035=CARTESIAN_POINT('',(-0.0119365362629715,-0.0147898787470809,0.0435652034709374));
#37036=CARTESIAN_POINT('',(-0.0120403900735433,-0.0149195795744518,0.0435366464007867));
#37037=CARTESIAN_POINT('',(-0.0108198925979776,-0.0156465840107142,0.0437692594703814));
#37038=CARTESIAN_POINT('',(-0.0108163199250364,-0.0156490630775139,0.0436006916153784));
#37039=CARTESIAN_POINT('',(-0.0109104810471308,-0.0157862543759804,0.0435721982202406));
#37040=CARTESIAN_POINT('',(-0.0100332035243057,-0.0161625907830607,0.0437930330870528));
#37041=CARTESIAN_POINT('',(-0.0100294118999466,-0.0161649308481875,0.0436243007810868));
#37042=CARTESIAN_POINT('',(-0.0101168709807266,-0.0163067379621374,0.0435959391586223));
#37043=CARTESIAN_POINT('',(-0.00879216804478874,-0.0168499676414349,0.0438288524583594));
#37044=CARTESIAN_POINT('',(-0.00878838298714177,-0.0168519440507585,0.0436599726789626));
#37045=CARTESIAN_POINT('',(-0.00886488046311359,-0.016999950121302,0.0436317300461986));
#37046=CARTESIAN_POINT('',(-0.00836678386397909,-0.0170652673611714,0.0438408466943254));
#37047=CARTESIAN_POINT('',(-0.00836304432866484,-0.0170671014593458,0.0436719450370716));
#37048=CARTESIAN_POINT('',(-0.00843573579653323,-0.0172170398082215,0.0436437200774922));
#37049=CARTESIAN_POINT('',(-0.0075020610771226,-0.017462688851661,0.0438646944908298));
#37050=CARTESIAN_POINT('',(-0.00749825266116855,-0.0174643237639204,0.0436958505787912));
#37051=CARTESIAN_POINT('',(-0.00756332366407398,-0.0176176520556874,0.0436675786878873));
#37052=CARTESIAN_POINT('',(-0.00706477335026738,-0.0176440200780838,0.0438765091448451));
#37053=CARTESIAN_POINT('',(-0.00706096804890941,-0.0176455456634563,0.0437077276210945));
#37054=CARTESIAN_POINT('',(-0.00712213400549059,-0.0178003908836544,0.0436794056320971));
#37055=CARTESIAN_POINT('',(-0.00573852163197963,-0.0181372334578677,0.0439118465916292));
#37056=CARTESIAN_POINT('',(-0.00573481921426324,-0.0181383895346569,0.043743248215973));
#37057=CARTESIAN_POINT('',(-0.00578406965445588,-0.0182973783030603,0.0437147801112202));
#37058=CARTESIAN_POINT('',(-0.00483524655341389,-0.0183986073071731,0.0439352782854798));
#37059=CARTESIAN_POINT('',(-0.00483116852585073,-0.018399678078592,0.0437667982660677));
#37060=CARTESIAN_POINT('',(-0.00487278496604438,-0.0185606870996588,0.0437382340115492));
#37061=CARTESIAN_POINT('',(-0.00345175988030525,-0.018689768424132,0.0439708278229095));
#37062=CARTESIAN_POINT('',(-0.00344762002299385,-0.0186905334044925,0.0438023259722786));
#37063=CARTESIAN_POINT('',(-0.00347710746122709,-0.0188540666261451,0.0437737798863077));
#37064=CARTESIAN_POINT('',(-0.00298581589560767,-0.0187699373373264,0.0439827406953793));
#37065=CARTESIAN_POINT('',(-0.0029815945202669,-0.0187706073743282,0.0438142055341818));
#37066=CARTESIAN_POINT('',(-0.00300706790601135,-0.0189348569344595,0.0437856860537803));
#37067=CARTESIAN_POINT('',(-0.00204413509094533,-0.0188956914649766,0.0440067439405659));
#37068=CARTESIAN_POINT('',(-0.0020398726024733,-0.0188961543529943,0.0438380990315092));
#37069=CARTESIAN_POINT('',(-0.00205712019075991,-0.0190615944017183,0.043809667889534));
#37070=CARTESIAN_POINT('',(-0.00156830996680276,-0.0189410826500961,0.0440188361973977));
#37071=CARTESIAN_POINT('',(-0.00156401312848831,-0.0189414363423515,0.0438501166546982));
#37072=CARTESIAN_POINT('',(-0.00157712255868106,-0.0191073458819795,0.0438217454397834));
#37073=CARTESIAN_POINT('',(-0.000150154974504012,-0.0190229936109595,0.0440547882027781));
#37074=CARTESIAN_POINT('',(-0.000145588323455347,-0.0190230462400798,0.0438858608428633));
#37075=CARTESIAN_POINT('',(-0.000146539257022446,-0.0191898518619688,0.0438576554283318));
#37076=CARTESIAN_POINT('',(0.000790936627636269,-0.019006824755411,0.0440784751545746));
#37077=CARTESIAN_POINT('',(0.00079488815217747,-0.0190066717643781,0.0439094489159697));
#37078=CARTESIAN_POINT('',(0.000802778280913555,-0.0191733936965734,0.0438813251670424));
#37079=CARTESIAN_POINT('',(0.00219618132025848,-0.018878507081242,0.0441137553179732));
#37080=CARTESIAN_POINT('',(0.00220026426151477,-0.0188780303767659,0.0439448926290359));
#37081=CARTESIAN_POINT('',(0.00222026970006894,-0.0190434097462471,0.0439166358100154));
#37082=CARTESIAN_POINT('',(0.00266352565200299,-0.0188183179147578,0.044125500051272));
#37083=CARTESIAN_POINT('',(0.00266757183132161,-0.0188177472930563,0.0439567138470368));
#37084=CARTESIAN_POINT('',(0.00269168007756433,-0.0189824858408622,0.0439283955500007));
#37085=CARTESIAN_POINT('',(0.00359603759486174,-0.0186625821272436,0.0441490943401665));
#37086=CARTESIAN_POINT('',(0.00360004882176565,-0.0186618071442378,0.0439804491106465));
#37087=CARTESIAN_POINT('',(0.00363229267182523,-0.0188249870752841,0.0439520176016581));
#37088=CARTESIAN_POINT('',(0.00406249693166183,-0.018566712268401,0.0441609772952625));
#37089=CARTESIAN_POINT('',(0.00406652662148846,-0.0185658318754706,0.0439923969852757));
#37090=CARTESIAN_POINT('',(0.00410279819761283,-0.0187280858111682,0.0439639133116328));
#37091=CARTESIAN_POINT('',(0.0054497458441839,-0.0182265469396486,0.0441967294346886));
#37092=CARTESIAN_POINT('',(0.00545358262028542,-0.0182253907484344,0.0440282635270871));
#37093=CARTESIAN_POINT('',(0.00550208037506834,-0.0183844526912413,0.043999689222396));
#37094=CARTESIAN_POINT('',(0.0063465881321194,-0.0179333509087761,0.0442204124173489));
#37095=CARTESIAN_POINT('',(0.00635078959146271,-0.0179318513293681,0.044051922194549));
#37096=CARTESIAN_POINT('',(0.00640671032868024,-0.0180884976215383,0.0440233656430663));
#37097=CARTESIAN_POINT('',(0.00808635138350872,-0.0172190353109135,0.0442679269748748));
#37098=CARTESIAN_POINT('',(0.00809041392297931,-0.017217141719978,0.0440992201967355));
#37099=CARTESIAN_POINT('',(0.00816162287321362,-0.0173677050659826,0.0440708378489379));
#37100=CARTESIAN_POINT('',(0.00892927000815383,-0.0167979099162225,0.0442917541796707));
#37101=CARTESIAN_POINT('',(0.00893299016981508,-0.0167959318351288,0.0441228595101268));
#37102=CARTESIAN_POINT('',(0.00901191021205074,-0.0169428561738456,0.0440946294830747));
#37103=CARTESIAN_POINT('',(0.0101520063527029,-0.0160674259644378,0.0443275330439986));
#37104=CARTESIAN_POINT('',(0.0101555419580498,-0.0160651915313776,0.0441586481003933));
#37105=CARTESIAN_POINT('',(0.0102451320892497,-0.0162056661571703,0.0441304092466795));
#37106=CARTESIAN_POINT('',(0.0105530248471654,-0.0158068996913036,0.044339482773545));
#37107=CARTESIAN_POINT('',(0.0105564418813125,-0.0158046204070512,0.0441706477123562));
#37108=CARTESIAN_POINT('',(0.0106495601594412,-0.0159427075570703,0.0441423688593859));
#37109=CARTESIAN_POINT('',(0.0113276393296575,-0.0152613563778918,0.0443631513426043));
#37110=CARTESIAN_POINT('',(0.0113309294112503,-0.0152589120313818,0.0441944369148397));
#37111=CARTESIAN_POINT('',(0.0114307338273626,-0.0153920774500531,0.0441660609369003));
#37112=CARTESIAN_POINT('',(0.0117029764469784,-0.0149753766232204,0.0443749201640164));
#37113=CARTESIAN_POINT('',(0.0117062142264097,-0.014972848377937,0.044206274963219));
#37114=CARTESIAN_POINT('',(0.0118092359999567,-0.0151034343162899,0.0441778433696202));
#37115=CARTESIAN_POINT('',(0.0127937553720812,-0.0140785679095087,0.0444102184577515));
#37116=CARTESIAN_POINT('',(0.0127966613896774,-0.0140759112274443,0.0442417266093446));
#37117=CARTESIAN_POINT('',(0.0129092222992875,-0.0141983513220654,0.0442131731350139));
#37118=CARTESIAN_POINT('',(0.0134741569144895,-0.0134290820888552,0.0444337558421312));
#37119=CARTESIAN_POINT('',(0.0134772527320605,-0.0134259630804598,0.0442653011928489));
#37120=CARTESIAN_POINT('',(0.0135953916495663,-0.0135429841222457,0.0442367161687069));
#37121=CARTESIAN_POINT('',(0.0144237533789395,-0.0123765353003134,0.0444695263456117));
#37122=CARTESIAN_POINT('',(0.0144265326456636,-0.0123732984504774,0.0443009422857109));
#37123=CARTESIAN_POINT('',(0.0145531437809366,-0.0124810665665217,0.044272462273439));
#37124=CARTESIAN_POINT('',(0.014728973698961,-0.0120118394212612,0.0444815468308796));
#37125=CARTESIAN_POINT('',(0.0147316951565146,-0.0120084990933084,0.0443128975475059));
#37126=CARTESIAN_POINT('',(0.014861002078107,-0.0121131453026525,0.0442844698258981));
#37127=CARTESIAN_POINT('',(0.0153124435690708,-0.0112585978012749,0.0445056611452321));
#37128=CARTESIAN_POINT('',(0.0153150013476016,-0.0112551227366345,0.0443368677121805));
#37129=CARTESIAN_POINT('',(0.0154495190689251,-0.0113532550497856,0.0443085558935153));
#37130=CARTESIAN_POINT('',(0.0155882444401666,-0.0108733330355269,0.044517651274913));
#37131=CARTESIAN_POINT('',(0.015590696367927,-0.0108698150645401,0.0443487801060638));
#37132=CARTESIAN_POINT('',(0.0157277077512303,-0.0109645953864914,0.0443205309058317));
#37133=CARTESIAN_POINT('',(0.0163691710964169,-0.00969232591939088,0.0445534115306125));
#37134=CARTESIAN_POINT('',(0.0163714464651926,-0.0096885044715376,0.0443843937751832));
#37135=CARTESIAN_POINT('',(0.0165153057183266,-0.00977314734794248,0.0443562611772637));
#37136=CARTESIAN_POINT('',(0.0168280705761621,-0.0088715031155409,0.0445768634194298));
#37137=CARTESIAN_POINT('',(0.0168298773963543,-0.00886811101355751,0.0444079315425907));
#37138=CARTESIAN_POINT('',(0.0169779056880622,-0.00894497234046972,0.0443797317026779));
#37139=CARTESIAN_POINT('',(0.0174243664825587,-0.00759034481382917,0.0446121254669567));
#37140=CARTESIAN_POINT('',(0.0174259949050814,-0.00758660128298118,0.0444434164716655));
#37141=CARTESIAN_POINT('',(0.0175788687236481,-0.0076523374825775,0.0444150361200228));
#37142=CARTESIAN_POINT('',(0.0176077269712503,-0.00715493768044318,0.044623902971559));
#37143=CARTESIAN_POINT('',(0.0176092735419983,-0.00715113617066766,0.0444552686054724));
#37144=CARTESIAN_POINT('',(0.0177636450242175,-0.00721303680883226,0.0444268282888931));
#37145=CARTESIAN_POINT('',(0.0179429471430136,-0.00626704317267242,0.0446476246433377));
#37146=CARTESIAN_POINT('',(0.0179443015041592,-0.00626316109002529,0.0444790985861339));
#37147=CARTESIAN_POINT('',(0.0181014572970104,-0.00631723472224765,0.0444505715980682));
#37148=CARTESIAN_POINT('',(0.0180949724965274,-0.00581348313029633,0.0446595961907196));
#37149=CARTESIAN_POINT('',(0.0180962497503941,-0.00580950869140011,0.0444911054619768));
#37150=CARTESIAN_POINT('',(0.0182546606191797,-0.00585965097994928,0.0444625500480985));
#37151=CARTESIAN_POINT('',(0.0184959816576352,-0.00444939608775399,0.0446953019660419));
#37152=CARTESIAN_POINT('',(0.018496958849312,-0.00444533144179018,0.0445268281214257));
#37153=CARTESIAN_POINT('',(0.0186588124479543,-0.00448350568352277,0.0444982597993328));
#37154=CARTESIAN_POINT('',(0.0186931222678959,-0.00352871098495351,0.0447190290468711));
#37155=CARTESIAN_POINT('',(0.0186939437072589,-0.00352428564961369,0.0445504499253981));
#37156=CARTESIAN_POINT('',(0.0188575680062124,-0.00355473555155383,0.0445219648388717));
#37157=CARTESIAN_POINT('',(0.0189502365720984,-0.00166527931571346,0.0447665822341533));
#37158=CARTESIAN_POINT('',(0.018950644510258,-0.00166079385680507,0.0445977639216191));
#37159=CARTESIAN_POINT('',(0.019116722434608,-0.00167496209543366,0.0445694709399891));
#37160=CARTESIAN_POINT('',(0.0190102135009348,-0.000721603842810055,0.0447903421458515));
#37161=CARTESIAN_POINT('',(0.0190103745399458,-0.000717601730914487,0.0446214564980412));
#37162=CARTESIAN_POINT('',(0.0191770421900481,-0.000723030408788185,0.044593219240517));
#37163=CARTESIAN_POINT('',(0.018986960795852,0.0011850102083368,0.0448380670765952));
#37164=CARTESIAN_POINT('',(0.0189867025259235,0.00118898747267436,0.0446693435332347));
#37165=CARTESIAN_POINT('',(0.019152908993654,0.00120026015000668,0.0446409755342579));
#37166=CARTESIAN_POINT('',(0.0189041423152777,0.00212551926781839,0.0448615838243566));
#37167=CARTESIAN_POINT('',(0.0189036821317303,0.00212963503647161,0.0446929831128389));
#37168=CARTESIAN_POINT('',(0.0190689879037131,0.00214897360311979,0.0446645159522766));
#37169=CARTESIAN_POINT('',(0.0186018416989233,0.00398194854842917,0.0449088004107678));
#37170=CARTESIAN_POINT('',(0.0186009686985388,0.00398601997834442,0.0447402351269411));
#37171=CARTESIAN_POINT('',(0.0187635204626675,0.00402158525230051,0.0447117401013397));
#37172=CARTESIAN_POINT('',(0.018382348236366,0.00489786678679497,0.0449324980666317));
#37173=CARTESIAN_POINT('',(0.0183811758465752,0.00490221341614218,0.0447638576997983));
#37174=CARTESIAN_POINT('',(0.0185419608917838,0.00494549245887479,0.0447354216516968));
#37175=CARTESIAN_POINT('',(0.0179479062185708,0.00625280887325386,0.0449684687154362));
#37176=CARTESIAN_POINT('',(0.0179464943902665,0.0062568668598083,0.0447996428701011));
#37177=CARTESIAN_POINT('',(0.0181035577501198,0.00631225917213096,0.0447713570828861));
#37178=CARTESIAN_POINT('',(0.0177848319526543,0.00670258003035173,0.0449805623302665));
#37179=CARTESIAN_POINT('',(0.0177833220738104,0.0067065823745434,0.044811669837172));
#37180=CARTESIAN_POINT('',(0.0179390092271524,0.00676595516139307,0.0447834377416771));
#37181=CARTESIAN_POINT('',(0.0174283660129482,0.00758135111745522,0.0450045007790738));
#37182=CARTESIAN_POINT('',(0.0174266647478471,0.00758526492612676,0.044835520321406));
#37183=CARTESIAN_POINT('',(0.0175792882272123,0.00765236524299947,0.0448073587601778));
#37184=CARTESIAN_POINT('',(0.0172345799272952,0.00801192762887884,0.0450163802018326));
#37185=CARTESIAN_POINT('',(0.0172328260256429,0.00801570218315257,0.0448473807885217));
#37186=CARTESIAN_POINT('',(0.0173837160900334,0.00808665880559119,0.044819234475737));
#37187=CARTESIAN_POINT('',(0.0166075233603181,0.00927777377603944,0.0450517759664179));
#37188=CARTESIAN_POINT('',(0.0166055475967738,0.00928129451252952,0.0448828660892816));
#37189=CARTESIAN_POINT('',(0.0167507482423559,0.00936337902246387,0.0448546477246791));
#37190=CARTESIAN_POINT('',(0.0161288042341429,0.0100872971570167,0.045075201634086));
#37191=CARTESIAN_POINT('',(0.0161265818413747,0.0100908515680599,0.044906415077906));
#37192=CARTESIAN_POINT('',(0.0162675033284656,0.0101798132291225,0.0448780970874073));
#37193=CARTESIAN_POINT('',(0.0150489933465771,0.011636996571794,0.0451226650624829));
#37194=CARTESIAN_POINT('',(0.0150464140875462,0.0116403332888076,0.044953877202022));
#37195=CARTESIAN_POINT('',(0.0151778180517796,0.0117428355520045,0.0449255608731273));
#37196=CARTESIAN_POINT('',(0.0144429210201034,0.0123812019000766,0.0451468654392096));
#37197=CARTESIAN_POINT('',(0.0144400888394576,0.0123844959594197,0.0449779557783555));
#37198=CARTESIAN_POINT('',(0.0145663435705823,0.0124935061387918,0.0449497372028042));
#37199=CARTESIAN_POINT('',(0.0134685515906739,0.01340974086514,0.0451825562446273));
#37200=CARTESIAN_POINT('',(0.0134655641188587,0.0134127421838492,0.0450135709211634));
#37201=CARTESIAN_POINT('',(0.0135832408374368,0.0135308531692142,0.044985413154267));
#37202=CARTESIAN_POINT('',(0.0131321446070276,0.0137392811386444,0.0451945442673237));
#37203=CARTESIAN_POINT('',(0.0131256289439562,0.0137453916307771,0.0450257518235694));
#37204=CARTESIAN_POINT('',(0.0132431889465559,0.0138637230531154,0.0449973950606197));
#37205=CARTESIAN_POINT('',(0.0124364953824679,0.0143720092815323,0.0452251638180739));
#37206=CARTESIAN_POINT('',(0.0124288742620619,0.0143787537513585,0.0450495329495826));
#37207=CARTESIAN_POINT('',(0.0125454954734933,0.014508430361355,0.045026887812166));
#37208=CARTESIAN_POINT('',(0.0120772417837534,0.0146752127027321,0.0452428101759807));
#37209=CARTESIAN_POINT('',(0.0120638269525999,0.0146858875331522,0.0450611716033226));
#37210=CARTESIAN_POINT('',(0.0121871631803304,0.0148195625152073,0.0450435765026652));
#37211=CARTESIAN_POINT('',(0.0117064311150657,0.0149652754918919,0.0452574848572202));
#37212=CARTESIAN_POINT('',(0.0117017888431181,0.0149689068608435,0.0450664117380016));
#37213=CARTESIAN_POINT('',(0.0118192405672073,0.0151194868273913,0.045057783841377));
#37214=CARTESIAN_POINT('',(0.0135722303973856,0.013533541237196,0.0359858240518714));
#37215=CARTESIAN_POINT('',(0.013571622451412,0.0135341506939564,0.0359858446287144));
#37216=CARTESIAN_POINT('',(0.0135710144649558,0.0135347601152105,0.0359858652089559));
#37217=CARTESIAN_POINT('',(0.0135704064380024,0.0135353695009377,0.0359858857925812));
#37218=CARTESIAN_POINT('',(0.013570381808041,0.0135353510208532,0.0359857053491133));
#37219=CARTESIAN_POINT('',(0.0135722054159049,0.0135335224965762,0.0359856410406521));
#37220=CARTESIAN_POINT('',(0.0135704064380024,0.0135353695009377,0.0359858857925812));
#37221=CARTESIAN_POINT('',(0.0129036548070887,0.0142025964264844,0.0360085613545014));
#37222=CARTESIAN_POINT('',(0.0114611542483502,0.015448287166601,0.0360565775520735));
#37223=CARTESIAN_POINT('',(0.00909268102828358,0.0169514288058979,0.0361261820467452));
#37224=CARTESIAN_POINT('',(0.00647950090834531,0.0181120230886494,0.0361973328999772));
#37225=CARTESIAN_POINT('',(0.00287123768415439,0.0191126352245148,0.0362904101950139));
#37226=CARTESIAN_POINT('',(-0.000949677653458001,0.0193040117092425,0.036383990993209));
#37227=CARTESIAN_POINT('',(-0.00465102395568895,0.0186649672159626,0.0364775817539468));
#37228=CARTESIAN_POINT('',(-0.00735877861404485,0.0177724795978704,0.0365488480499061));
#37229=CARTESIAN_POINT('',(-0.00986237510046936,0.0165149149662214,0.0366178923756543));
#37230=CARTESIAN_POINT('',(-0.0122031927539453,0.0148689465492879,0.0366889731522299));
#37231=CARTESIAN_POINT('',(-0.0142334523316336,0.0129392989422766,0.036759211703248));
#37232=CARTESIAN_POINT('',(-0.0165756388821674,0.00994417572451643,0.0368531214084936));
#37233=CARTESIAN_POINT('',(-0.0181924746613863,0.00652957200048769,0.0369463139710774));
#37234=CARTESIAN_POINT('',(-0.0190261366639813,0.00283095697289045,0.037040783606513));
#37235=CARTESIAN_POINT('',(-0.0192356036156563,3.10245497638384E-5,0.0371099791765328));
#37236=CARTESIAN_POINT('',(-0.0190276609287275,-0.00281986751540245,0.0371812491961335));
#37237=CARTESIAN_POINT('',(-0.0184175486612505,-0.00555180159649675,0.0372512868433642));
#37238=CARTESIAN_POINT('',(-0.0173909007355282,-0.00821999643371724,0.0373217709207786));
#37239=CARTESIAN_POINT('',(-0.0155472357929439,-0.0114804485039055,0.0374146763836055));
#37240=CARTESIAN_POINT('',(-0.0129812711275626,-0.0143196448224917,0.0375095754402841));
#37241=CARTESIAN_POINT('',(-0.00991561226323179,-0.0164827729265894,0.0376021168106601));
#37242=CARTESIAN_POINT('',(-0.00736738918219378,-0.0177687876227372,0.0376735234568528));
#37243=CARTESIAN_POINT('',(-0.00470947524897598,-0.0186507963509578,0.0377433369936091));
#37244=CARTESIAN_POINT('',(-0.00189108857945936,-0.0191423871997642,0.0378138213830228));
#37245=CARTESIAN_POINT('',(0.000910715726981787,-0.0192135649995635,0.0378834946810402));
#37246=CARTESIAN_POINT('',(0.00468277998063177,-0.018754393673424,0.0379785967435593));
#37247=CARTESIAN_POINT('',(0.00823984871720905,-0.0174842256403166,0.038070608869898));
#37248=CARTESIAN_POINT('',(0.0114487135063291,-0.0154576187460385,0.0381657497589623));
#37249=CARTESIAN_POINT('',(0.0135750376321758,-0.0136288998762221,0.0382353373342439));
#37250=CARTESIAN_POINT('',(0.0154455607200755,-0.0114643757136311,0.0383058925721234));
#37251=CARTESIAN_POINT('',(0.0169460544911987,-0.00910137325776664,0.0383756965966336));
#37252=CARTESIAN_POINT('',(0.0181079837303313,-0.0064910253901214,0.0384470673278848));
#37253=CARTESIAN_POINT('',(0.0191108011877866,-0.00287969512756302,0.0385393341131735));
#37254=CARTESIAN_POINT('',(0.0193047752323962,0.000942482875310808,0.0386346426198504));
#37255=CARTESIAN_POINT('',(0.0186685396227,0.00463742868741877,0.0387273673272984));
#37256=CARTESIAN_POINT('',(0.0177752289363512,0.00735055566752598,0.0387979645948326));
#37257=CARTESIAN_POINT('',(0.0165206086502515,0.00985311295239786,0.0388679691965797));
#37258=CARTESIAN_POINT('',(0.0148766674473921,0.0121949490591136,0.0389391342272032));
#37259=CARTESIAN_POINT('',(0.01294505238683,0.0142268795201651,0.0390082266480041));
#37260=CARTESIAN_POINT('',(0.0099567045497623,0.0165679247808239,0.0391030670710161));
#37261=CARTESIAN_POINT('',(0.0065426543257601,0.0181884803449958,0.0391960410642187));
#37262=CARTESIAN_POINT('',(0.00283903174349127,0.0190242081903609,0.0392900399397408));
#37263=CARTESIAN_POINT('',(4.38490655596054E-5,0.0192361688814356,0.0393602697848384));
#37264=CARTESIAN_POINT('',(-0.00281004131304883,0.0190293691514629,0.0394310992984519));
#37265=CARTESIAN_POINT('',(-0.00554232062030348,0.018419201885183,0.0395002744159604));
#37266=CARTESIAN_POINT('',(-0.00820898556038362,0.0173965778160439,0.0395717411832897));
#37267=CARTESIAN_POINT('',(-0.0114742864751092,0.0155529990072777,0.0396650713268737));
#37268=CARTESIAN_POINT('',(-0.0143131630885914,0.0129864061291896,0.0397586567093767));
#37269=CARTESIAN_POINT('',(-0.0164770616490012,0.0099268333205899,0.0398525410597318));
#37270=CARTESIAN_POINT('',(-0.0177649442009733,0.00737585987507787,0.039923028622799));
#37271=CARTESIAN_POINT('',(-0.0186472732982126,0.00471948953200742,0.0399924153858999));
#37272=CARTESIAN_POINT('',(-0.0191420687654524,0.00190205791917451,0.0400641061633313));
#37273=CARTESIAN_POINT('',(-0.0192142413096121,-0.000901990499639644,0.0401336489952851));
#37274=CARTESIAN_POINT('',(-0.0187562485469653,-0.00466875352929895,0.0402272503848521));
#37275=CARTESIAN_POINT('',(-0.0174917918871846,-0.00822819321455465,0.0403213139141897));
#37276=CARTESIAN_POINT('',(-0.0154621346436875,-0.0114408475718349,0.0404149417726169));
#37277=CARTESIAN_POINT('',(-0.0130282697127285,-0.0142774028557637,0.0405080405422995));
#37278=CARTESIAN_POINT('',(-0.00991772725739437,-0.0165898472986663,0.0406038619665578));
#37279=CARTESIAN_POINT('',(-0.00650157038579237,-0.0181024042748644,0.0406960707748711));
#37280=CARTESIAN_POINT('',(-0.00283785189841008,-0.0191212759720652,0.0407913351761265));
#37281=CARTESIAN_POINT('',(0.000937913129849199,-0.0193054515594452,0.0408836654044101));
#37282=CARTESIAN_POINT('',(0.00467025910808451,-0.0186595712437484,0.040978151102671));
#37283=CARTESIAN_POINT('',(0.00733820999792568,-0.0177819060626436,0.0410483768661127));
#37284=CARTESIAN_POINT('',(0.00989155145181529,-0.0164970073708586,0.0411187932842743));
#37285=CARTESIAN_POINT('',(0.0121812338948817,-0.0148866942940362,0.0411882341378734));
#37286=CARTESIAN_POINT('',(0.014253871300758,-0.0129173177050997,0.041259874016993));
#37287=CARTESIAN_POINT('',(0.0165589423148337,-0.00996570506020658,0.0413523505246238));
#37288=CARTESIAN_POINT('',(0.0181987394001929,-0.00650877737202476,0.0414469474664291));
#37289=CARTESIAN_POINT('',(0.0190245583516211,-0.00284627763176505,0.0415404863055993));
#37290=CARTESIAN_POINT('',(0.0192349788993391,-1.59539726163646E-6,0.0416107539642663));
#37291=CARTESIAN_POINT('',(0.0190319275532812,0.00279222673795976,0.0416804834955781));
#37292=CARTESIAN_POINT('',(0.0184075959098026,0.00558491368172862,0.0417520799986338));
#37293=CARTESIAN_POINT('',(0.0174002159456161,0.00819885203171055,0.0418211207893093));
#37294=CARTESIAN_POINT('',(0.0155304117868589,0.0115077766069531,0.0419155436438027));
#37295=CARTESIAN_POINT('',(0.0129942997411232,0.0143099062533922,0.0420092587497652));
#37296=CARTESIAN_POINT('',(0.00989525219106396,0.0164943213741518,0.0421027240848228));
#37297=CARTESIAN_POINT('',(0.00739018379856946,0.0177598494195308,0.0421728334549609));
#37298=CARTESIAN_POINT('',(0.00467632015585543,0.0186587240946092,0.0422440867836995));
#37299=CARTESIAN_POINT('',(0.00191797928105586,0.019139444207654,0.0423130970541599));
#37300=CARTESIAN_POINT('',(-0.000939580996455013,0.0192127314628508,0.0423842646067995));
#37301=CARTESIAN_POINT('',(-0.00465786360752577,0.018757941368385,0.0424780497498932));
#37302=CARTESIAN_POINT('',(-0.00826216839263219,0.0174718493774394,0.0425712861204916));
#37303=CARTESIAN_POINT('',(-0.0114344912440321,0.0154686357718066,0.0426652059172387));
#37304=CARTESIAN_POINT('',(-0.0135973082957804,0.0136059152434581,0.0427360529788289));
#37305=CARTESIAN_POINT('',(-0.0154285214424727,0.0114874784926826,0.0428051467613729));
#37306=CARTESIAN_POINT('',(-0.0169623829047404,0.00907163903114544,0.0428766144053203));
#37307=CARTESIAN_POINT('',(-0.0181003765664633,0.00651102758883087,0.0429466099962544));
#37308=CARTESIAN_POINT('',(-0.0191177805482954,0.00284995029113454,0.043040145704006));
#37309=CARTESIAN_POINT('',(-0.0193076442662596,-0.000922083928633924,0.0431340336701195));
#37310=CARTESIAN_POINT('',(-0.0186616566678583,-0.00466251490238888,0.0432279439783494));
#37311=CARTESIAN_POINT('',(-0.0177855984884859,-0.00732641341906906,0.0432972980389548));
#37312=CARTESIAN_POINT('',(-0.0165026697800636,-0.00988354444963145,0.0433689452125143));
#37313=CARTESIAN_POINT('',(-0.0148934742398978,-0.0121738803150184,0.0434385501993439));
#37314=CARTESIAN_POINT('',(-0.0129255270265096,-0.0142454806427628,0.0435089315675407));
#37315=CARTESIAN_POINT('',(-0.00997363753172828,-0.0165550355305691,0.0436024404412654));
#37316=CARTESIAN_POINT('',(-0.00651591788045801,-0.0181956490664393,0.0436966553566115));
#37317=CARTESIAN_POINT('',(-0.00285917471887072,-0.0190218574159515,0.0437895534176288));
#37318=CARTESIAN_POINT('',(-1.05277131322721E-5,-0.0192359682957396,0.0438611833771685));
#37319=CARTESIAN_POINT('',(0.00278148828475611,-0.0190335330487122,0.0439304599081606));
#37320=CARTESIAN_POINT('',(0.00557400542520404,-0.018410296510478,0.0440011115084237));
#37321=CARTESIAN_POINT('',(0.00819095256643428,-0.0174042318789018,0.0440711755507273));
#37322=CARTESIAN_POINT('',(0.0114970905449255,-0.0155386360544783,0.044165649129919));
#37323=CARTESIAN_POINT('',(0.0142998874984641,-0.0130047891899287,0.044258106598296));
#37324=CARTESIAN_POINT('',(0.0164908396020408,-0.0099029506612536,0.0443533197536154));
#37325=CARTESIAN_POINT('',(0.0177548865816707,-0.00740121656659391,0.0444224149752557));
#37326=CARTESIAN_POINT('',(0.0186560074938801,-0.00468541369120382,0.044493277880731));
#37327=CARTESIAN_POINT('',(0.0191388070731541,-0.00192739063184559,0.0445633351153983));
#37328=CARTESIAN_POINT('',(0.0192136610128768,0.000927057006012885,0.0446341570303284));
#37329=CARTESIAN_POINT('',(0.018759240023971,0.00464974285234913,0.0447269745742573));
#37330=CARTESIAN_POINT('',(0.0174759318076413,0.00825514969859494,0.0448218815682069));
#37331=CARTESIAN_POINT('',(0.0154759249806765,0.0114239507166203,0.0449149351018996));
#37332=CARTESIAN_POINT('',(0.0142331749641786,0.0128696482775912,0.0449616671411353));
#37333=CARTESIAN_POINT('',(0.0135704061500135,0.0135353688366664,0.0449858818020359));
#37334=CARTESIAN_POINT('',(0.0135703818080404,0.0135353510208537,0.0449857053491134));
#37335=CARTESIAN_POINT('',(0.0135704061500135,0.0135353688366664,0.0449858818020359));
#37336=CARTESIAN_POINT('',(0.0135697787646435,0.0135359980612715,0.0449859048203564));
#37337=CARTESIAN_POINT('',(0.0135691513405032,0.0135366272436449,0.0449859278421744));
#37338=CARTESIAN_POINT('',(0.0135685238776161,0.0135372563838022,0.044985950867507));
#37339=CARTESIAN_POINT('',(0.0135684991741454,0.013537238300348,0.0449857717828516));
#37340=CARTESIAN_POINT('',(0.0133154147536411,0.0135536195643592,0.0451879940399793));
#37341=CARTESIAN_POINT('',(0.0133539318946654,0.0135157713941986,0.0451308262115416));
#37342=CARTESIAN_POINT('',(0.0134070278463947,0.0134882525375867,0.0450704755958725));
#37343=CARTESIAN_POINT('',(0.0135303802320928,0.0135096732135866,0.0449939978015681));
#37344=CARTESIAN_POINT('',(0.0135685175242368,0.0135372652440246,0.0449859511372893));
#37345=CARTESIAN_POINT('',(0.0133154066073941,0.0135536114581477,0.0451879939181472));
#37346=CARTESIAN_POINT('',(0.019,-3.9861646017376E-17,0.0448084035990546));
#37347=CARTESIAN_POINT('',(0.019,0.00251516724482142,0.0448716686934959));
#37348=CARTESIAN_POINT('',(0.0179878255210343,0.0075443863126556,0.0449981988823785));
#37349=CARTESIAN_POINT('',(0.0151095869241771,0.011790947767256,0.045124729071261));
#37350=CARTESIAN_POINT('',(0.013315398557798,0.0135536032569568,0.0451879941657023));
#37351=CARTESIAN_POINT('',(0.019,-4.91593209544621E-17,0.0448084035990546));
#37352=CARTESIAN_POINT('',(-0.019,7.9723292034752E-17,0.0433082162077251));
#37353=CARTESIAN_POINT('',(-0.019,-0.00248709418409184,0.0433707240156971));
#37354=CARTESIAN_POINT('',(-0.0180107055600589,-0.00746012312352672,0.0434957396316413));
#37355=CARTESIAN_POINT('',(-0.0137847972460807,-0.0137848390811386,0.0436832630555575));
#37356=CARTESIAN_POINT('',(-0.00746027851088496,-0.0180106936071851,0.0438707864794736));
#37357=CARTESIAN_POINT('',(-6.62381636648879E-17,-0.0194946531964074,0.0440583099033898));
#37358=CARTESIAN_POINT('',(0.00746027851088484,-0.0180106936071852,0.044245833327306));
#37359=CARTESIAN_POINT('',(0.0137847972460806,-0.0137848390811387,0.0444333567512222));
#37360=CARTESIAN_POINT('',(0.0180107055600588,-0.00746012312352681,0.0446208801751384));
#37361=CARTESIAN_POINT('',(0.019,-0.00248709418409196,0.0447458957910825));
#37362=CARTESIAN_POINT('',(0.019,-3.9861646017376E-17,0.0448084035990546));
#37363=CARTESIAN_POINT('',(-0.019,6.35745487137311E-18,0.0433082162077251));
#37364=CARTESIAN_POINT('',(0.019,-3.9861646017376E-17,0.0418080680515213));
#37365=CARTESIAN_POINT('',(0.019,0.00248709418409188,0.0418705742246965));
#37366=CARTESIAN_POINT('',(0.0180107055600589,0.00746012312352676,0.0419955865710468));
#37367=CARTESIAN_POINT('',(0.0137847972460807,0.0137848390811386,0.0421831050905722));
#37368=CARTESIAN_POINT('',(0.00746027851088491,0.0180106936071852,0.0423706236100977));
#37369=CARTESIAN_POINT('',(2.09173148415435E-17,0.0194946531964074,0.0425581421296232));
#37370=CARTESIAN_POINT('',(-0.00746027851088488,0.0180106936071852,0.0427456606491487));
#37371=CARTESIAN_POINT('',(-0.0137847972460807,0.0137848390811386,0.0429331791686741));
#37372=CARTESIAN_POINT('',(-0.0180107055600589,0.00746012312352679,0.0431206976881996));
#37373=CARTESIAN_POINT('',(-0.019,0.00248709418409192,0.0432457100345499));
#37374=CARTESIAN_POINT('',(-0.019,0.,0.0433082162077251));
#37375=CARTESIAN_POINT('',(0.019,8.95355988618673E-18,0.0418080680515213));
#37376=CARTESIAN_POINT('',(-0.019,7.9723292034752E-17,0.0403085360942082));
#37377=CARTESIAN_POINT('',(-0.019,-0.00248709418409184,0.0403710165924296));
#37378=CARTESIAN_POINT('',(-0.0180107055600589,-0.00746012312352672,0.0404959775888723));
#37379=CARTESIAN_POINT('',(-0.0137847972460807,-0.0137848390811386,0.0406834190835365));
#37380=CARTESIAN_POINT('',(-0.00746027851088496,-0.0180106936071851,0.0408708605782006));
#37381=CARTESIAN_POINT('',(-6.62381636648879E-17,-0.0194946531964074,0.0410583020728647));
#37382=CARTESIAN_POINT('',(0.00746027851088484,-0.0180106936071852,0.0412457435675289));
#37383=CARTESIAN_POINT('',(0.0137847972460806,-0.0137848390811387,0.041433185062193));
#37384=CARTESIAN_POINT('',(0.0180107055600588,-0.00746012312352681,0.0416206265568572));
#37385=CARTESIAN_POINT('',(0.019,-0.00248709418409196,0.0417455875532999));
#37386=CARTESIAN_POINT('',(0.019,-3.9861646017376E-17,0.0418080680515213));
#37387=CARTESIAN_POINT('',(-0.019,-5.14795421335563E-17,0.0403085360942082));
#37388=CARTESIAN_POINT('',(0.019,-1.60883575115789E-14,0.0388082819344598));
#37389=CARTESIAN_POINT('',(0.0190000000000021,0.0024870941840765,0.0388707925244493));
#37390=CARTESIAN_POINT('',(0.0180107055600646,0.00746012312351353,0.0389958137044283));
#37391=CARTESIAN_POINT('',(0.0137847972460896,0.0137848390811301,0.0391833454743969));
#37392=CARTESIAN_POINT('',(0.00746027851089453,0.0180106936071815,0.0393708772443654));
#37393=CARTESIAN_POINT('',(8.25327519264503E-15,0.0194946531964077,0.039558409014334));
#37394=CARTESIAN_POINT('',(-0.00746027851087928,0.0180106936071878,0.0397459407843026));
#37395=CARTESIAN_POINT('',(-0.0137847972460779,0.0137848390811417,0.0399334725542711));
#37396=CARTESIAN_POINT('',(-0.0180107055600583,0.00746012312352879,0.0401210043242397));
#37397=CARTESIAN_POINT('',(-0.019,0.00248709418409259,0.0402460255042187));
#37398=CARTESIAN_POINT('',(-0.019,0.,0.0403085360942082));
#37399=CARTESIAN_POINT('',(0.019,-1.61262072877242E-14,0.0388082819344598));
#37400=CARTESIAN_POINT('',(-0.019,7.9723292034752E-17,0.0373080333342866));
#37401=CARTESIAN_POINT('',(-0.019,-0.00248709418409117,0.0373705436926271));
#37402=CARTESIAN_POINT('',(-0.0180107055600594,-0.00746012312352471,0.0374955644093082));
#37403=CARTESIAN_POINT('',(-0.0137847972460834,-0.0137848390811355,0.0376830954843299));
#37404=CARTESIAN_POINT('',(-0.00746027851089055,-0.0180106936071825,0.0378706265593515));
#37405=CARTESIAN_POINT('',(-8.29022911553176E-15,-0.0194946531964072,0.0380581576343732));
#37406=CARTESIAN_POINT('',(0.00746027851087523,-0.0180106936071889,0.0382456887093948));
#37407=CARTESIAN_POINT('',(0.0137847972460717,-0.0137848390811472,0.0384332197844165));
#37408=CARTESIAN_POINT('',(0.0180107055600531,-0.00746012312354004,0.0386207508594381));
#37409=CARTESIAN_POINT('',(0.0189999999999979,-0.00248709418410734,0.0387457715761192));
#37410=CARTESIAN_POINT('',(0.019,-1.60883575115789E-14,0.0388082819344598));
#37411=CARTESIAN_POINT('',(-0.019,4.54954461515252E-17,0.0373080333342866));
#37412=CARTESIAN_POINT('',(0.0135947752080227,0.0132733600509943,0.0361780495049504));
#37413=CARTESIAN_POINT('',(0.0109753255973188,0.0159562397807274,0.0362722148240618));
#37414=CARTESIAN_POINT('',(0.00410759749193419,0.0197186661240115,0.0364605454622845));
#37415=CARTESIAN_POINT('',(-0.00759708232316353,0.0186558030226723,0.0367430414196185));
#37416=CARTESIAN_POINT('',(-0.0167144641966965,0.0112394322580518,0.0370255373769525));
#37417=CARTESIAN_POINT('',(-0.019,0.00374958129758905,0.0372138680151752));
#37418=CARTESIAN_POINT('',(-0.019,0.,0.0373080333342866));
#37419=CARTESIAN_POINT('',(0.0135947999945552,0.0132733842837834,0.0361780492531812));
#37420=CARTESIAN_POINT('',(0.0135722168793318,0.0135335509805304,0.0359858244640535));
#37421=CARTESIAN_POINT('',(0.0135448185599411,0.0134952138392626,0.0359934900823968));
#37422=CARTESIAN_POINT('',(0.0135257317133337,0.0133692298759541,0.0360662817720579));
#37423=CARTESIAN_POINT('',(0.01355510517062,0.0133140557191526,0.0361236111063028));
#37424=CARTESIAN_POINT('',(0.0135948247028973,0.013273408596571,0.0361780493788477));
#37425=CARTESIAN_POINT('',(0.0134214493584107,0.0137296865857405,0.0432866344382823));
#37426=CARTESIAN_POINT('',(0.0135335436975079,0.0135722252250888,0.0430141821297884));
#37427=CARTESIAN_POINT('',(0.013495210770777,0.0135448275134576,0.0430065171585731));
#37428=CARTESIAN_POINT('',(0.0133692322905148,0.0135257199693753,0.0429337223945325));
#37429=CARTESIAN_POINT('',(0.0133140317184763,0.0135551063111274,0.0428763716821991));
#37430=CARTESIAN_POINT('',(0.0132733898758911,0.0135948055585231,0.0428219506155445));
#37431=CARTESIAN_POINT('',(0.0135335224965767,0.0135722054159043,0.043014358959348));
#37432=CARTESIAN_POINT('',(0.0132733749216108,0.0135947904241369,0.0428219507431747));
#37433=CARTESIAN_POINT('',(0.013273389787819,0.013594805644538,0.0428219507440773));
#37434=CARTESIAN_POINT('',(0.0132873978720912,0.0135810767699496,0.0436106318019714));
#37435=CARTESIAN_POINT('',(0.0133014061630618,0.0135673481069843,0.044399312859878));
#37436=CARTESIAN_POINT('',(0.0133154146613603,0.0135536196550256,0.0451879939177751));
#37437=CARTESIAN_POINT('',(0.0135684900658114,0.0135372510065474,0.0449857721696874));
#37438=CARTESIAN_POINT('',(0.0135773102099061,0.0135436364574972,0.0449837092908326));
#37439=CARTESIAN_POINT('',(0.013585610235647,0.0135507472552975,0.0449816684977748));
#37440=CARTESIAN_POINT('',(0.0135932791745505,0.0135584892152446,0.04497965012538));
#37441=CARTESIAN_POINT('',(0.0135932855747001,0.0135584828160982,0.0449796496479541));
#37442=CARTESIAN_POINT('',(0.0135581119696951,0.0135929312435436,0.0430202462678972));
#37443=CARTESIAN_POINT('',(0.0135698386395681,0.0135814462998891,0.0436733806520518));
#37444=CARTESIAN_POINT('',(0.0135815653094411,0.0135699613562345,0.0443265150362065));
#37445=CARTESIAN_POINT('',(0.0135932919793141,0.01355847641258,0.0449796494203611));
#37446=CARTESIAN_POINT('',(0.0135581121542913,0.0135929310589486,0.0430202462613394));
#37447=CARTESIAN_POINT('',(0.0134129571505461,0.0137267074203667,0.0430647873816228));
#37448=CARTESIAN_POINT('',(0.0137072504062847,0.0134443055379105,0.0344382290633684));
#37449=CARTESIAN_POINT('',(0.0135929312391456,0.0135581119741857,0.0359797534819639));
#37450=CARTESIAN_POINT('',(0.0135814462969616,0.0135698386425573,0.0353266191814339));
#37451=CARTESIAN_POINT('',(0.0135699613547775,0.0135815653109288,0.0346734848809039));
#37452=CARTESIAN_POINT('',(0.0135584764125934,0.0135932919793003,0.0340203505803739));
#37453=CARTESIAN_POINT('',(0.0135929265320308,0.0135581166810912,0.0359797536492453));
#37454=CARTESIAN_POINT('',(0.0135584942938894,0.013593274088762,0.0340203499447281));
#37455=CARTESIAN_POINT('',(0.0135929218292959,0.0135581213835245,0.0359797540662325));
#37456=CARTESIAN_POINT('',(0.0135853714857596,0.0135505002845721,0.0359817380910061));
#37457=CARTESIAN_POINT('',(0.0135784328080303,0.0135422677164711,0.0359837004096582));
#37458=CARTESIAN_POINT('',(0.0135721957749986,0.0135335294431583,0.035985641334575));
#37459=CARTESIAN_POINT('',(0.0135948247912817,0.013273408506102,0.0361780492510671));
#37460=CARTESIAN_POINT('',(0.013582176399302,0.0132862934770642,0.0354520328340541));
#37461=CARTESIAN_POINT('',(0.0135695281552721,0.0132991785925841,0.034726016417029));
#37462=CARTESIAN_POINT('',(0.0135568800588317,0.0133120638530298,0.0340000000000049));
#37463=CARTESIAN_POINT('',(0.0135568795107147,0.0133120633124194,0.0340000000714098));
#37464=CARTESIAN_POINT('',(0.0135568800588317,0.0133120638530298,0.0340000000000049));
#37465=CARTESIAN_POINT('',(0.0134973437325541,0.0133726944056705,0.0340021345712315));
#37466=CARTESIAN_POINT('',(0.0134833406019767,0.0134731784383755,0.0340041824205536));
#37467=CARTESIAN_POINT('',(0.0135240277273972,0.0135478066093083,0.0340048056241338));
#37468=CARTESIAN_POINT('',(0.0135239956136941,0.0135478241103007,0.0340048065022042));
#37469=CARTESIAN_POINT('',(0.013524003738558,0.0135477557735323,0.0340049411805581));
#37470=CARTESIAN_POINT('',(0.0135307046512648,0.0135597739884161,0.034010635057669));
#37471=CARTESIAN_POINT('',(0.0135386771238806,0.013571204328877,0.0340148023321076));
#37472=CARTESIAN_POINT('',(0.0135477915582315,0.0135817709703549,0.0340174403420765));
#37473=CARTESIAN_POINT('',(0.0135477529825173,0.0135818241209862,0.0340173607059137));
#37474=CARTESIAN_POINT('',(0.0135478083242499,0.013581796823751,0.0340172784089037));
#37475=CARTESIAN_POINT('',(0.0135512239240925,0.013585753873175,0.034018307096211));
#37476=CARTESIAN_POINT('',(0.0135547955159251,0.0135895776046143,0.0340193306530654));
#37477=CARTESIAN_POINT('',(0.0135585121708165,0.0135932562026847,0.0340203490599872));
#37478=CARTESIAN_POINT('',(0.0116902830159151,0.0149778931431562,0.0428599463516431));
#37479=CARTESIAN_POINT('',(0.0116931710101275,0.0149756390564587,0.0430503063057597));
#37480=CARTESIAN_POINT('',(0.0118103172895557,0.0151254370962809,0.0430596673970548));
#37481=CARTESIAN_POINT('',(0.0120521347075991,0.0146954669938212,0.0428510193710697));
#37482=CARTESIAN_POINT('',(0.0120463403333191,0.0146998796691399,0.0430329133156896));
#37483=CARTESIAN_POINT('',(0.012169281878152,0.0148333572635523,0.043050300662135));
#37484=CARTESIAN_POINT('',(0.0124034181196442,0.0144002110811048,0.0428449791580437));
#37485=CARTESIAN_POINT('',(0.0124025987870145,0.014401052044687,0.0430207675215794));
#37486=CARTESIAN_POINT('',(0.0125195284727906,0.014530291707653,0.0430433330239107));
#37487=CARTESIAN_POINT('',(0.0130845840208317,0.0137842127534686,0.0428285872315281));
#37488=CARTESIAN_POINT('',(0.0130842898532399,0.0137843803990833,0.0429976801221143));
#37489=CARTESIAN_POINT('',(0.013202356541565,0.0139023415876872,0.0430257919690624));
#37490=CARTESIAN_POINT('',(0.0134144470800416,0.0134634970025393,0.0428172753093004));
#37491=CARTESIAN_POINT('',(0.0134174053542952,0.0134605501176648,0.0429862619436122));
#37492=CARTESIAN_POINT('',(0.0135355961119401,0.0135781436477725,0.0430144185077102));
#37493=CARTESIAN_POINT('',(0.0140525177593388,0.0127960887236721,0.0427941261457912));
#37494=CARTESIAN_POINT('',(0.014055317366581,0.0127930130042102,0.0429630677168436));
#37495=CARTESIAN_POINT('',(0.0141790411357716,0.0129046942850932,0.0429912609479785));
#37496=CARTESIAN_POINT('',(0.0143616949765598,0.0124481002284708,0.0427824935191819));
#37497=CARTESIAN_POINT('',(0.0143644074366707,0.0124449724353076,0.042951387722865));
#37498=CARTESIAN_POINT('',(0.0144907980623338,0.0125535396640404,0.0429796190399368));
#37499=CARTESIAN_POINT('',(0.0149497857727254,0.0117353051620916,0.0427593621514848));
#37500=CARTESIAN_POINT('',(0.0149523431506991,0.0117320456807852,0.0429281817614341));
#37501=CARTESIAN_POINT('',(0.0150837971203497,0.0118342876556258,0.0429564729838029));
#37502=CARTESIAN_POINT('',(0.0152294723517477,0.0113698647436651,0.0427478385465288));
#37503=CARTESIAN_POINT('',(0.0152319770460271,0.0113665102266746,0.0429166303007036));
#37504=CARTESIAN_POINT('',(0.0153658192417093,0.0114655502020432,0.0429449439662434));
#37505=CARTESIAN_POINT('',(0.0160263071195749,0.0102469551436804,0.0427132524624603));
#37506=CARTESIAN_POINT('',(0.0160285673500078,0.0102434197484808,0.0428820330083143));
#37507=CARTESIAN_POINT('',(0.0161693473214105,0.0103325727791095,0.0429103551701594));
#37508=CARTESIAN_POINT('',(0.0165014481567208,0.0094630354913846,0.042690150225392));
#37509=CARTESIAN_POINT('',(0.0165036238241023,0.00945922543135878,0.0428590308671038));
#37510=CARTESIAN_POINT('',(0.0166485580443778,0.00954171177013287,0.0428872730454636));
#37511=CARTESIAN_POINT('',(0.0173387201681154,0.00782404083015533,0.0426437283881698));
#37512=CARTESIAN_POINT('',(0.0173405252860055,0.00782005818368833,0.0428127489102698));
#37513=CARTESIAN_POINT('',(0.0174928823059129,0.00788821699864262,0.042840878879618));
#37514=CARTESIAN_POINT('',(0.0177017792545385,0.00696362252345879,0.0426204378972089));
#37515=CARTESIAN_POINT('',(0.0177032239234523,0.00695998520536297,0.0427893636130864));
#37516=CARTESIAN_POINT('',(0.0178587818090731,0.00702013455170138,0.0428175686439992));
#37517=CARTESIAN_POINT('',(0.01829135151316,0.0052222109539592,0.0425745084349314));
#37518=CARTESIAN_POINT('',(0.0182924116960155,0.00521845009209468,0.0427431979283701));
#37519=CARTESIAN_POINT('',(0.0184528145256494,0.00526322955959588,0.0427715929411472));
#37520=CARTESIAN_POINT('',(0.018521285815859,0.00433610970738375,0.0425516847293725));
#37521=CARTESIAN_POINT('',(0.0185222391423024,0.00433204131040263,0.0427202675416825));
#37522=CARTESIAN_POINT('',(0.0186844239914438,0.00436927932320634,0.042748749164781));
#37523=CARTESIAN_POINT('',(0.0187697946121533,0.00298408765527847,0.0425171503472629));
#37524=CARTESIAN_POINT('',(0.01877045363091,0.00297994313561533,0.042685728914949));
#37525=CARTESIAN_POINT('',(0.0189347575854476,0.00300534506766644,0.042714213540631));
#37526=CARTESIAN_POINT('',(0.0188365030539556,0.0025295870523152,0.0425055923622042));
#37527=CARTESIAN_POINT('',(0.018837067060276,0.00252538076843415,0.0426741900952649));
#37528=CARTESIAN_POINT('',(0.0190019562100111,0.00254684875031955,0.0427026594088152));
#37529=CARTESIAN_POINT('',(0.0189370424924125,0.00161278628388406,0.042482336595439));
#37530=CARTESIAN_POINT('',(0.0189374045043678,0.0016085482150996,0.0426510039425693));
#37531=CARTESIAN_POINT('',(0.0191032191867231,0.00162199833661797,0.0426794171728615));
#37532=CARTESIAN_POINT('',(0.0189708812277667,0.00114859680187076,0.0424705911901054));
#37533=CARTESIAN_POINT('',(0.0189711379065816,0.00114433652145144,0.0426393079072488));
#37534=CARTESIAN_POINT('',(0.0191372911038253,0.00115373805721631,0.0426676814839808));
#37535=CARTESIAN_POINT('',(0.0190209950275129,-0.000237033433351926,0.0424355926553317));
#37536=CARTESIAN_POINT('',(0.0190209497223709,-0.000241456245903946,0.0426044396407925));
#37537=CARTESIAN_POINT('',(0.0191876388490383,-0.000244031484226691,0.042632709358546));
#37538=CARTESIAN_POINT('',(0.0189870113680649,-0.00115373022849519,0.0424125803189054));
#37539=CARTESIAN_POINT('',(0.0189867827922777,-0.00115767434941267,0.0425814574287911));
#37540=CARTESIAN_POINT('',(0.0191531423808799,-0.00116873009402599,0.0426097014877259));
#37541=CARTESIAN_POINT('',(0.01878820108735,-0.00297341454097277,0.0423668250938457));
#37542=CARTESIAN_POINT('',(0.0187875748666947,-0.00297729522553448,0.0425354908799519));
#37543=CARTESIAN_POINT('',(0.0189518834296028,-0.00300425733578145,0.0425639051805033));
#37544=CARTESIAN_POINT('',(0.0186233771455114,-0.00387639995695613,0.0423439862261447));
#37545=CARTESIAN_POINT('',(0.0186225432584859,-0.00388042491741729,0.0425125064146396));
#37546=CARTESIAN_POINT('',(0.0187852255652517,-0.00391507702103005,0.0425410381574683));
#37547=CARTESIAN_POINT('',(0.018274665533442,-0.00522022632396231,0.042309152018482));
#37548=CARTESIAN_POINT('',(0.0182735185981123,-0.00522424059044953,0.0424776276212393));
#37549=CARTESIAN_POINT('',(0.018433065606184,-0.00527057225040032,0.0425061948623966));
#37550=CARTESIAN_POINT('',(0.0181415131957001,-0.00566548389294523,0.0422974690443417));
#37551=CARTESIAN_POINT('',(0.0181402488570975,-0.00566952979746723,0.0424659542399351));
#37552=CARTESIAN_POINT('',(0.0182986445061403,-0.00571969889912052,0.0424945138859628));
#37553=CARTESIAN_POINT('',(0.0178456356258476,-0.00653800412056035,0.0422742355721382));
#37554=CARTESIAN_POINT('',(0.01784417337783,-0.00654199865587599,0.0424427903170468));
#37555=CARTESIAN_POINT('',(0.0180000251383591,-0.00659981281907227,0.0424712938630216));
#37556=CARTESIAN_POINT('',(0.0176824727806309,-0.00696706185954262,0.0422626389575521));
#37557=CARTESIAN_POINT('',(0.0176808958611167,-0.00697105930894539,0.0424312511668981));
#37558=CARTESIAN_POINT('',(0.0178353846391573,-0.0070326110295655,0.042459708658246));
#37559=CARTESIAN_POINT('',(0.0171480895942689,-0.00823299469432104,0.0422278683197848));
#37560=CARTESIAN_POINT('',(0.0171461373322301,-0.00823709568725569,0.0423966772546488));
#37561=CARTESIAN_POINT('',(0.0172962060414754,-0.00830958663110433,0.0424249776750704));
#37562=CARTESIAN_POINT('',(0.0167322082218721,-0.00904873968945994,0.0422047043777687));
#37563=CARTESIAN_POINT('',(0.0167302252983698,-0.00905240950799154,0.0423737030474594));
#37564=CARTESIAN_POINT('',(0.0168766534262386,-0.00913246361302278,0.0424018492301041));
#37565=CARTESIAN_POINT('',(0.016017776215106,-0.0102294899975369,0.0421700643431915));
#37566=CARTESIAN_POINT('',(0.0160155304590875,-0.0102330052947774,0.0423390256013007));
#37567=CARTESIAN_POINT('',(0.016155636454386,-0.0103233270447803,0.0423672030318007));
#37568=CARTESIAN_POINT('',(0.0157639583700152,-0.0106166212588865,0.0421585036680659));
#37569=CARTESIAN_POINT('',(0.0157616695074945,-0.0106200230247405,0.0423274092588773));
#37570=CARTESIAN_POINT('',(0.0158994422981835,-0.0107137457762176,0.0423556313959451));
#37571=CARTESIAN_POINT('',(0.0152272801277975,-0.0113729930254,0.0421353516005726));
#37572=CARTESIAN_POINT('',(0.0152248306979017,-0.0113762692680501,0.0423041230377585));
#37573=CARTESIAN_POINT('',(0.0153577455710004,-0.0114765124210403,0.0423324532441816));
#37574=CARTESIAN_POINT('',(0.0149467207633388,-0.0117391073542602,0.0421238563386887));
#37575=CARTESIAN_POINT('',(0.0149441912424758,-0.011742330856736,0.042292551641195));
#37576=CARTESIAN_POINT('',(0.0150745657995214,-0.0118457083325256,0.0423209430424921));
#37577=CARTESIAN_POINT('',(0.014069384387219,-0.0128022199314398,0.0420894336026386));
#37578=CARTESIAN_POINT('',(0.0140667495585985,-0.0128050961186576,0.0422579508410219));
#37579=CARTESIAN_POINT('',(0.0141891092920901,-0.0129177740881277,0.0422864839229229));
#37580=CARTESIAN_POINT('',(0.0134371299761888,-0.0134641659672828,0.0420665540087471));
#37581=CARTESIAN_POINT('',(0.0134340693086654,-0.0134672128418654,0.0422350107166076));
#37582=CARTESIAN_POINT('',(0.0135511085133077,-0.0135853119533646,0.0422635938651249));
#37583=CARTESIAN_POINT('',(0.0124182379819621,-0.0143874049856545,0.0420319064132249));
#37584=CARTESIAN_POINT('',(0.0124150273123975,-0.0143901774409011,0.042200448692967));
#37585=CARTESIAN_POINT('',(0.0125231164314169,-0.0145164470673288,0.0422289622752316));
#37586=CARTESIAN_POINT('',(0.0120668099875688,-0.0146834930653284,0.0420203064047687));
#37587=CARTESIAN_POINT('',(0.0120634984437343,-0.0146862124321403,0.0421888988715361));
#37588=CARTESIAN_POINT('',(0.0121685715444792,-0.0148150826757778,0.0422173722479392));
#37589=CARTESIAN_POINT('',(0.0113398839142431,-0.0152518820047602,0.0419969773954634));
#37590=CARTESIAN_POINT('',(0.0113364404448756,-0.0152544443950376,0.0421656892462165));
#37591=CARTESIAN_POINT('',(0.0114352161544657,-0.0153883695391954,0.0421940666469763));
#37592=CARTESIAN_POINT('',(0.0109628963113278,-0.0155250853649475,0.0419852045877687));
#37593=CARTESIAN_POINT('',(0.0109593996535451,-0.015527552715629,0.0421539852232674));
#37594=CARTESIAN_POINT('',(0.0110549026147746,-0.0156639311220682,0.0421823072906783));
#37595=CARTESIAN_POINT('',(0.00981181685212698,-0.0162966786354659,0.0419502110722857));
#37596=CARTESIAN_POINT('',(0.00980802468690172,-0.01629897358581,0.0421191318727581));
#37597=CARTESIAN_POINT('',(0.00989364532800342,-0.0164421136866359,0.0421473424316667));
#37598=CARTESIAN_POINT('',(0.00901475697726111,-0.0167502804088702,0.0419273086335697));
#37599=CARTESIAN_POINT('',(0.00901132318991663,-0.0167521431827161,0.0420961716539068));
#37600=CARTESIAN_POINT('',(0.00908946333972755,-0.0168994032707856,0.042124427101066));
#37601=CARTESIAN_POINT('',(0.00736294102394891,-0.017539237059026,0.0418815910047469));
#37602=CARTESIAN_POINT('',(0.00735934332100566,-0.0175407328683054,0.0420502112706503));
#37603=CARTESIAN_POINT('',(0.00742286512687939,-0.0176945902813653,0.0420786619207783));
#37604=CARTESIAN_POINT('',(0.00650818842987571,-0.0178745959943225,0.0418587210379212));
#37605=CARTESIAN_POINT('',(0.00650426173646775,-0.0178760265082283,0.0420272155291122));
#37606=CARTESIAN_POINT('',(0.00656049360996185,-0.0180325388998404,0.0420557680753826));
#37607=CARTESIAN_POINT('',(0.00518125028045295,-0.0182857614055599,0.041823816448597));
#37608=CARTESIAN_POINT('',(0.00517721155912882,-0.0182869059511596,0.0419923098442186));
#37609=CARTESIAN_POINT('',(0.00522182413452343,-0.0184469637090321,0.0420208627463016));
#37610=CARTESIAN_POINT('',(0.00473302918526943,-0.0184068044888232,0.041812126906403));
#37611=CARTESIAN_POINT('',(0.00472890347372164,-0.0184078641754975,0.0419806453549743));
#37612=CARTESIAN_POINT('',(0.0047696534380224,-0.0185689808298537,0.0420091782601784));
#37613=CARTESIAN_POINT('',(0.0038358425246037,-0.0186144655814991,0.0417888747841534));
#37614=CARTESIAN_POINT('',(0.00383165727851394,-0.0186153295086939,0.0419574872132742));
#37615=CARTESIAN_POINT('',(0.0038645762329874,-0.0187783348169813,0.0419859444304395));
#37616=CARTESIAN_POINT('',(0.00338529441764298,-0.0187015910797529,0.0417772706777386));
#37617=CARTESIAN_POINT('',(0.00338105873145118,-0.0187023559206568,0.0419459499657417));
#37618=CARTESIAN_POINT('',(0.00341007283725043,-0.0188661831320287,0.0419743535313619));
#37619=CARTESIAN_POINT('',(0.00202788112853736,-0.0189136619130776,0.0417424975737002));
#37620=CARTESIAN_POINT('',(0.00202335886061544,-0.0189141621421916,0.0419113796263766));
#37621=CARTESIAN_POINT('',(0.00204075058140732,-0.0190799965482407,0.0419396213395313));
#37622=CARTESIAN_POINT('',(0.00111527657161592,-0.0189895589037079,0.0417193881771659));
#37623=CARTESIAN_POINT('',(0.00111124227504146,-0.0189898031317301,0.0418884155584991));
#37624=CARTESIAN_POINT('',(0.00112015474861678,-0.0191564722530023,0.0419165384790431));
#37625=CARTESIAN_POINT('',(-0.000265294000998375,-0.0190037211195645,0.0416848185347678));
#37626=CARTESIAN_POINT('',(-0.000269428442369693,-0.0190036621380701,0.0418537311390249));
#37627=CARTESIAN_POINT('',(-0.000272495772136029,-0.0191702742242257,0.0418819477804248));
#37628=CARTESIAN_POINT('',(-0.000728732033634883,-0.0189916745362715,0.0416732557504993));
#37629=CARTESIAN_POINT('',(-0.000732820037092626,-0.0189915195967747,0.0418420994331531));
#37630=CARTESIAN_POINT('',(-0.000739986546925877,-0.0191579229371231,0.0418703714712338));
#37631=CARTESIAN_POINT('',(-0.00165373562203119,-0.0189335657117441,0.0416501273390889));
#37632=CARTESIAN_POINT('',(-0.00165780624299728,-0.0189332081609065,0.0418188303614342));
#37633=CARTESIAN_POINT('',(-0.00167306542317714,-0.019098906581222,0.0418472155134374));
#37634=CARTESIAN_POINT('',(-0.00211248068853893,-0.0188877839132358,0.0416386316906292));
#37635=CARTESIAN_POINT('',(-0.00211656646631519,-0.0188873284324626,0.0418072640790303));
#37636=CARTESIAN_POINT('',(-0.00213580880466304,-0.0190525260587537,0.0418357059935484));
#37637=CARTESIAN_POINT('',(-0.00347773927072136,-0.0187015815591903,0.0416041849706497));
#37638=CARTESIAN_POINT('',(-0.00348162652046194,-0.0187008479423524,0.0417726705774203));
#37639=CARTESIAN_POINT('',(-0.00351295591739027,-0.0188641701699972,0.0418012290733437));
#37640=CARTESIAN_POINT('',(-0.00437333147735052,-0.0185125519319189,0.0415812587715974));
#37641=CARTESIAN_POINT('',(-0.00437759833950889,-0.0185115353469389,0.0417497243726128));
#37642=CARTESIAN_POINT('',(-0.00441633674311674,-0.0186732446887795,0.0417783005161147));
#37643=CARTESIAN_POINT('',(-0.00569496546372668,-0.0181322232552342,0.0415465561867922));
#37644=CARTESIAN_POINT('',(-0.00569903285637957,-0.0181309470948967,0.0417151481291254));
#37645=CARTESIAN_POINT('',(-0.00574948949371243,-0.0182893784412442,0.041743621825817));
#37646=CARTESIAN_POINT('',(-0.00613187049197437,-0.0179892539573154,0.0415349403823787));
#37647=CARTESIAN_POINT('',(-0.00613593199273233,-0.0179878677665463,0.041703592466749));
#37648=CARTESIAN_POINT('',(-0.00619020606605926,-0.0181451101082577,0.0417320179172437));
#37649=CARTESIAN_POINT('',(-0.00699824753201534,-0.0176702468899496,0.0415115949679377));
#37650=CARTESIAN_POINT('',(-0.00700224077842883,-0.0176686672242183,0.0416803700106387));
#37651=CARTESIAN_POINT('',(-0.00706413549155712,-0.0178232177429544,0.041708696666812));
#37652=CARTESIAN_POINT('',(-0.00742903192881274,-0.0174935023824463,0.0414998280884315));
#37653=CARTESIAN_POINT('',(-0.0074329489177034,-0.0174918378058293,0.0416686662427243));
#37654=CARTESIAN_POINT('',(-0.00749867232381402,-0.0176448802050545,0.041696942049135));
#37655=CARTESIAN_POINT('',(-0.00869032741724389,-0.0169213112197901,0.0414649178500639));
#37656=CARTESIAN_POINT('',(-0.00869418687519932,-0.0169193355548257,0.0416338437926145));
#37657=CARTESIAN_POINT('',(-0.00877088847995754,-0.0170674546052026,0.0416620501385558));
#37658=CARTESIAN_POINT('',(-0.00949541012943664,-0.0164825663036929,0.0414420968225364));
#37659=CARTESIAN_POINT('',(-0.00949879916290607,-0.0164806289998969,0.0416108965446497));
#37660=CARTESIAN_POINT('',(-0.00958282526174183,-0.0166245274441401,0.0416392030299223));
#37661=CARTESIAN_POINT('',(-0.011035843026309,-0.015493481667479,0.0413963760214746));
#37662=CARTESIAN_POINT('',(-0.0110390142666174,-0.0154912068770508,0.0415649356273811));
#37663=CARTESIAN_POINT('',(-0.0111363429551393,-0.0156261549868809,0.0415934348585898));
#37664=CARTESIAN_POINT('',(-0.0117711969806298,-0.0149431487864239,0.0413734589339542));
#37665=CARTESIAN_POINT('',(-0.0117745442615457,-0.0149405081863807,0.0415419254432952));
#37666=CARTESIAN_POINT('',(-0.0118779346569039,-0.0150707384352058,0.0415705006369759));
#37667=CARTESIAN_POINT('',(-0.0128199481592734,-0.0140308097662266,0.0413384716889231));
#37668=CARTESIAN_POINT('',(-0.012823067714203,-0.0140279603099078,0.0415069895682356));
#37669=CARTESIAN_POINT('',(-0.0129356768813544,-0.0141501790244631,0.0415355227587738));
#37670=CARTESIAN_POINT('',(-0.0131583924556861,-0.0137138083624527,0.0413267762023185));
#37671=CARTESIAN_POINT('',(-0.0131614799831733,-0.0137108438196155,0.0414953358982116));
#37672=CARTESIAN_POINT('',(-0.0132770380386662,-0.0138303492432787,0.0415238356278214));
#37673=CARTESIAN_POINT('',(-0.0138069700858022,-0.0130606052260107,0.0413035058920913));
#37674=CARTESIAN_POINT('',(-0.0138099208402457,-0.0130574883812653,0.0414721829022311));
#37675=CARTESIAN_POINT('',(-0.0139312251053164,-0.0131713498971273,0.0415005882390922));
#37676=CARTESIAN_POINT('',(-0.0141181439008517,-0.0127235089245412,0.0412918967450829));
#37677=CARTESIAN_POINT('',(-0.0141210247482436,-0.0127203095251467,0.0414606478017125));
#37678=CARTESIAN_POINT('',(-0.0142451005343464,-0.0128312773693915,0.0414889936415347));
#37679=CARTESIAN_POINT('',(-0.0150129218862625,-0.0116812175165574,0.0412571354604048));
#37680=CARTESIAN_POINT('',(-0.0150157186559916,-0.0116776467432949,0.0414260831456741));
#37681=CARTESIAN_POINT('',(-0.0151476205529159,-0.011779777158378,0.0414542721088526));
#37682=CARTESIAN_POINT('',(-0.01555798632197,-0.0109451809228585,0.0412341123150795));
#37683=CARTESIAN_POINT('',(-0.0155602657948406,-0.0109419608402871,0.0414031309680951));
#37684=CARTESIAN_POINT('',(-0.0156973111570896,-0.0110372036045412,0.041431260883828));
#37685=CARTESIAN_POINT('',(-0.0162971169504362,-0.0097783413757642,0.0411995908304197));
#37686=CARTESIAN_POINT('',(-0.0162992291652279,-0.00977481775363762,0.0413684386072347));
#37687=CARTESIAN_POINT('',(-0.0164424487701677,-0.00985986039481064,0.0413967074338958));
#37688=CARTESIAN_POINT('',(-0.0165311120487054,-0.00937746317451068,0.0411880216094757));
#37689=CARTESIAN_POINT('',(-0.0165331316590963,-0.00937390677878347,0.0413567935110557));
#37690=CARTESIAN_POINT('',(-0.0166783146320643,-0.0094553672421763,0.0413851233286793));
#37691=CARTESIAN_POINT('',(-0.0169683564716308,-0.00856092050002925,0.0411649046912745));
#37692=CARTESIAN_POINT('',(-0.0169701970106566,-0.00855726823880796,0.0413335398874641));
#37693=CARTESIAN_POINT('',(-0.0171190407602751,-0.00863148649995367,0.0413619794574576));
#37694=CARTESIAN_POINT('',(-0.0171708318982631,-0.00814698393664201,0.0411534035337962));
#37695=CARTESIAN_POINT('',(-0.0171726031991398,-0.00814325333577635,0.0413219778223036));
#37696=CARTESIAN_POINT('',(-0.0173231215110601,-0.00821384212091386,0.04135046633409));
#37697=CARTESIAN_POINT('',(-0.017731052841533,-0.00688861571725598,0.0411189213796909));
#37698=CARTESIAN_POINT('',(-0.0177325036627002,-0.00688486082694156,0.0412873887707809));
#37699=CARTESIAN_POINT('',(-0.0178878115569066,-0.00694425476119435,0.0413159619695044));
#37700=CARTESIAN_POINT('',(-0.0180418326806221,-0.00602770999892709,0.0410959463402988));
#37701=CARTESIAN_POINT('',(-0.0180432304820099,-0.00602349188773519,0.0412644359078562));
#37702=CARTESIAN_POINT('',(-0.0182011250457587,-0.00607574524266206,0.0412929929117318));
#37703=CARTESIAN_POINT('',(-0.0184143243537723,-0.00470349999157568,0.0410611960622287));
#37704=CARTESIAN_POINT('',(-0.018415385042611,-0.00469935355214511,0.0412298456009654));
#37705=CARTESIAN_POINT('',(-0.0185767091459214,-0.0047398876927624,0.0412582730424759));
#37706=CARTESIAN_POINT('',(-0.0185228150547828,-0.00425660020659874,0.0410495686245358));
#37707=CARTESIAN_POINT('',(-0.0185237743487955,-0.00425241841302469,0.041218284609882));
#37708=CARTESIAN_POINT('',(-0.0186861086030493,-0.00428906376273253,0.0412466586769884));
#37709=CARTESIAN_POINT('',(-0.0187077611289919,-0.00335156626267243,0.0410262187428564));
#37710=CARTESIAN_POINT('',(-0.0187085187711582,-0.00334734607949911,0.0411950507959571));
#37711=CARTESIAN_POINT('',(-0.0188725694807397,-0.00337608669774606,0.0412233316825547));
#37712=CARTESIAN_POINT('',(-0.0187842366968955,-0.00289229495447753,0.0410144682252158));
#37713=CARTESIAN_POINT('',(-0.0187848784700295,-0.00288812412115976,0.0411833510122318));
#37714=CARTESIAN_POINT('',(-0.0189496506391086,-0.00291278606496349,0.0412115909366078));
#37715=CARTESIAN_POINT('',(-0.0189616205224653,-0.00151941459674208,0.0409796698818028));
#37716=CARTESIAN_POINT('',(-0.0189619553202701,-0.00151523087861793,0.0411485646407798));
#37717=CARTESIAN_POINT('',(-0.0191282421326548,-0.00152787230521512,0.0411767959526733));
#37718=CARTESIAN_POINT('',(-0.0190124404528775,-0.000604158586940465,0.0409568928165333));
#37719=CARTESIAN_POINT('',(-0.019012577162559,-0.000600234906611998,0.0411256224683206));
#37720=CARTESIAN_POINT('',(-0.0191790764987429,-0.0006045732690382,0.0411539854380646));
#37721=CARTESIAN_POINT('',(-0.0189824657699048,0.00122633309780874,0.0409111447946851));
#37722=CARTESIAN_POINT('',(-0.0189822006506171,0.00123025769157615,0.0410796570137007));
#37723=CARTESIAN_POINT('',(-0.019148119656424,0.00124193696623813,0.0411081942232454));
#37724=CARTESIAN_POINT('',(-0.018901681485365,0.00214156878432867,0.0408881742600273));
#37725=CARTESIAN_POINT('',(-0.0189011856661895,0.00214588577272389,0.0410566312425167));
#37726=CARTESIAN_POINT('',(-0.0190663413782543,0.00216515858537636,0.0410852142632578));
#37727=CARTESIAN_POINT('',(-0.0186033079109007,0.00397200385251819,0.0408414167966276));
#37728=CARTESIAN_POINT('',(-0.0186024021643551,0.00397628464649719,0.04101000529016));
#37729=CARTESIAN_POINT('',(-0.0187650302612908,0.00401157895411037,0.0410384821772507));
#37730=CARTESIAN_POINT('',(-0.0183884060347462,0.00486877543600975,0.0408180973509746));
#37731=CARTESIAN_POINT('',(-0.0183872407774818,0.00487312486704268,0.0409868575445279));
#37732=CARTESIAN_POINT('',(-0.0185482076679463,0.0049161996783548,0.0410151969013339));
#37733=CARTESIAN_POINT('',(-0.0178349912586725,0.00661449450434864,0.0407717946732109));
#37734=CARTESIAN_POINT('',(-0.0178334421068741,0.00661870714934465,0.0409407905791265));
#37735=CARTESIAN_POINT('',(-0.0179897532959718,0.0066771387497462,0.0409689407226237));
#37736=CARTESIAN_POINT('',(-0.0174961250798382,0.00746554037439665,0.0407488694971596));
#37737=CARTESIAN_POINT('',(-0.0174946130470671,0.00746911998997856,0.0409178491190281));
#37738=CARTESIAN_POINT('',(-0.0176476722262288,0.0075355226464926,0.0409460105147068));
#37739=CARTESIAN_POINT('',(-0.0168928793059809,0.00870877719466603,0.0407143705486902));
#37740=CARTESIAN_POINT('',(-0.0168910022413453,0.00871241404999286,0.0408831464914586));
#37741=CARTESIAN_POINT('',(-0.0170386211619198,0.00878938945676106,0.0409114730783643));
#37742=CARTESIAN_POINT('',(-0.0166749785102286,0.009119172623828,0.0407027900269581));
#37743=CARTESIAN_POINT('',(-0.016673014372315,0.00912276786271566,0.0408714896140114));
#37744=CARTESIAN_POINT('',(-0.0168186292924956,0.00920328236964801,0.0408998775668188));
#37745=CARTESIAN_POINT('',(-0.0162111810736432,0.00992027347694162,0.040679672638002));
#37746=CARTESIAN_POINT('',(-0.0162090391497371,0.00992377055421589,0.0408482493232186));
#37747=CARTESIAN_POINT('',(-0.0163504414828778,0.0100112107376009,0.0408767357850865));
#37748=CARTESIAN_POINT('',(-0.0159659475062535,0.0103101504290009,0.0406681615251639));
#37749=CARTESIAN_POINT('',(-0.0159636955796252,0.0103136390279756,0.0408366905658618));
#37750=CARTESIAN_POINT('',(-0.0161029146929399,0.0104044111131456,0.0408652153212605));
#37751=CARTESIAN_POINT('',(-0.0151912304606125,0.0114485476658325,0.0406336358038875));
#37752=CARTESIAN_POINT('',(-0.0151887570996142,0.0114518230940977,0.0408021035855928));
#37753=CARTESIAN_POINT('',(-0.0153210581004132,0.0115525415338422,0.0408306766175204));
#37754=CARTESIAN_POINT('',(-0.014622929391933,0.0121659929574409,0.0406106136156221));
#37755=CARTESIAN_POINT('',(-0.0146200524401287,0.0121694312704499,0.0407791444424219));
#37756=CARTESIAN_POINT('',(-0.0147476614088916,0.0122761729483964,0.0408076683603165));
#37757=CARTESIAN_POINT('',(-0.0136929237305084,0.013180068356081,0.0405758288898158));
#37758=CARTESIAN_POINT('',(-0.0136899494192345,0.0131831608238865,0.0407445413794423));
#37759=CARTESIAN_POINT('',(-0.0138093974149318,0.0132990263264894,0.0407729182659139));
#37760=CARTESIAN_POINT('',(-0.0133699463592963,0.0135077049833778,0.0405641959706274));
#37761=CARTESIAN_POINT('',(-0.0133669040498033,0.0135107142257478,0.0407329759851868));
#37762=CARTESIAN_POINT('',(-0.0134835617534226,0.0136295024291177,0.0407612985551758));
#37763=CARTESIAN_POINT('',(-0.0126974466340598,0.0141417257979227,0.0405408572390954));
#37764=CARTESIAN_POINT('',(-0.0126942704203723,0.0141445792357152,0.0407097330667613));
#37765=CARTESIAN_POINT('',(-0.0128050897757068,0.0142689756279715,0.0407379788512432));
#37766=CARTESIAN_POINT('',(-0.0123473085932254,0.0144484142221285,0.0405291421134551));
#37767=CARTESIAN_POINT('',(-0.0123441362264028,0.0144511258181016,0.0406980432058043));
#37768=CARTESIAN_POINT('',(-0.0124518316916227,0.0145782718212011,0.0407262686057894));
#37769=CARTESIAN_POINT('',(-0.0112739729442342,0.0153214994754053,0.0404944578563007));
#37770=CARTESIAN_POINT('',(-0.0112706968323,0.0153239022315645,0.040663288702221));
#37771=CARTESIAN_POINT('',(-0.0113688367160017,0.0154586468259733,0.0406915709389472));
#37772=CARTESIAN_POINT('',(-0.0105227406984075,0.015846449056652,0.0404716901640879));
#37773=CARTESIAN_POINT('',(-0.0105194393318638,0.0158486533708075,0.0406403488733642));
#37774=CARTESIAN_POINT('',(-0.0106107746025583,0.015987838740842,0.0406687690173338));
#37775=CARTESIAN_POINT('',(-0.00895054844538835,0.0167846865337946,0.0404258943877726));
#37776=CARTESIAN_POINT('',(-0.00894702830538813,0.0167865531939525,0.0405943749416822));
#37777=CARTESIAN_POINT('',(-0.00902446640469956,0.0169337143448247,0.0406229375719325));
#37778=CARTESIAN_POINT('',(-0.00812959521963859,0.0171979852881533,0.0404028663029833));
#37779=CARTESIAN_POINT('',(-0.00812559482701923,0.0171998652676137,0.0405713328036029));
#37780=CARTESIAN_POINT('',(-0.00819621891715045,0.0173504161809429,0.0405999083468083));
#37781=CARTESIAN_POINT('',(-0.00641509672436712,0.017908309535624,0.0403560080925695));
#37782=CARTESIAN_POINT('',(-0.00641091300938563,0.0179098201634833,0.0405246641763426));
#37783=CARTESIAN_POINT('',(-0.00646659766446683,0.0180667225222605,0.0405530870384352));
#37784=CARTESIAN_POINT('',(-0.00554091433977066,0.0181971572148494,0.0403327083910855));
#37785=CARTESIAN_POINT('',(-0.00553667044157995,0.0181984389167098,0.0405015540723921));
#37786=CARTESIAN_POINT('',(-0.00558474581842807,0.0183580808702938,0.0405298243010591));
#37787=CARTESIAN_POINT('',(-0.00376554510048333,0.0186456142971705,0.0402864854352754));
#37788=CARTESIAN_POINT('',(-0.00376123008776989,0.0186464944816664,0.0404555036912967));
#37789=CARTESIAN_POINT('',(-0.003793777162837,0.0188101927161195,0.0404836357763015));
#37790=CARTESIAN_POINT('',(-0.00286343258050692,0.0188055903779473,0.0402636501187532));
#37791=CARTESIAN_POINT('',(-0.00285961923148408,0.0188061864461319,0.0404325693382625));
#37792=CARTESIAN_POINT('',(-0.0028837112541823,0.0189712087558258,0.0404607794640954));
#37793=CARTESIAN_POINT('',(-0.00148820256203909,0.0189472325693201,0.0402291505505034));
#37794=CARTESIAN_POINT('',(-0.00148412777908813,0.0189475506496586,0.0403978539570062));
#37795=CARTESIAN_POINT('',(-0.0014963771872161,0.0191134985983846,0.0404262388044884));
#37796=CARTESIAN_POINT('',(-0.00102418033302645,0.0189780140213413,0.0402175547526945));
#37797=CARTESIAN_POINT('',(-0.00102007596487487,0.0189782370293938,0.040386186882504));
#37798=CARTESIAN_POINT('',(-0.00102827742850561,0.0191443495699763,0.0404146290013965));
#37799=CARTESIAN_POINT('',(-9.94653092085578E-5,0.0190053694571048,0.0401944269820207));
#37800=CARTESIAN_POINT('',(-9.5347232664673E-5,0.0190053897152703,0.0403629579225951));
#37801=CARTESIAN_POINT('',(-9.54513631700061E-5,0.0191715910880823,0.0403914809997104));
#37802=CARTESIAN_POINT('',(0.000360908106152808,0.0190021130416573,0.040182902582199));
#37803=CARTESIAN_POINT('',(0.00036508457391054,0.0190020340033433,0.0403514016925515));
#37804=CARTESIAN_POINT('',(0.000368953206577203,0.0191681528175206,0.0403799503793336));
#37805=CARTESIAN_POINT('',(0.00173621476613258,0.0189427499883702,0.0401483286629736));
#37806=CARTESIAN_POINT('',(0.00174038507151665,0.018942367524321,0.0403168150310215));
#37807=CARTESIAN_POINT('',(0.00175629267941908,0.019107900727566,0.0403453733464093));
#37808=CARTESIAN_POINT('',(0.00264536369269936,0.0188373023911365,0.0401252635252426));
#37809=CARTESIAN_POINT('',(0.0026498181005769,0.0188366634599821,0.0402938505069245));
#37810=CARTESIAN_POINT('',(0.00267338975743924,0.019001418134499,0.0403223292851573));
#37811=CARTESIAN_POINT('',(0.00399750571961914,0.0185803774351344,0.0400904610146314));
#37812=CARTESIAN_POINT('',(0.00400170347017837,0.0185794760270892,0.0402592365037631));
#37813=CARTESIAN_POINT('',(0.00403734421194199,0.0187420999168206,0.0402875627973426));
#37814=CARTESIAN_POINT('',(0.00444628218356663,0.0184782136197958,0.0400788298521094));
#37815=CARTESIAN_POINT('',(0.00445042005209088,0.0184772168738629,0.0402476677986115));
#37816=CARTESIAN_POINT('',(0.0044900385877306,0.0186389941549713,0.0402759437723264));
#37817=CARTESIAN_POINT('',(0.00533986815207782,0.0182400551521407,0.0400555200353558));
#37818=CARTESIAN_POINT('',(0.00534393651522462,0.0182388647581097,0.0402244184479622));
#37819=CARTESIAN_POINT('',(0.00539139235855439,0.018398589225329,0.040252646219197));
#37820=CARTESIAN_POINT('',(0.00578471697858165,0.0181038543997353,0.0400438539969031));
#37821=CARTESIAN_POINT('',(0.00578866000748204,0.0181025955764972,0.0402127406699899));
#37822=CARTESIAN_POINT('',(0.0058400860869573,0.0182610687836968,0.0402409778479568));
#37823=CARTESIAN_POINT('',(0.00709142101432577,0.0176511111999784,0.0400092547774132));
#37824=CARTESIAN_POINT('',(0.00709510071739637,0.0176496216435868,0.0401780135018141));
#37825=CARTESIAN_POINT('',(0.00715805298410857,0.0178038862360618,0.0402063533533533));
#37826=CARTESIAN_POINT('',(0.00793306601481205,0.0172888585230262,0.0399864822613801));
#37827=CARTESIAN_POINT('',(0.00793673177941187,0.0172871845585934,0.0401550748827933));
#37828=CARTESIAN_POINT('',(0.0080069017507295,0.0174380718168385,0.0401835482854934));
#37829=CARTESIAN_POINT('',(0.00955857914425509,0.0164460247527357,0.0399406223908872));
#37830=CARTESIAN_POINT('',(0.00956207819624298,0.016443983806927,0.0401090888995002));
#37831=CARTESIAN_POINT('',(0.00964637023866028,0.0165873089892121,0.0401376628762792));
#37832=CARTESIAN_POINT('',(0.0103426468499878,0.0159653185213969,0.0399175291538284));
#37833=CARTESIAN_POINT('',(0.0103464020038493,0.0159628707005397,0.0400860241419123));
#37834=CARTESIAN_POINT('',(0.0104372015299546,0.0161022307137298,0.0401145769416713));
#37835=CARTESIAN_POINT('',(0.01184973396054,0.0148810464826116,0.0398705942900101));
#37836=CARTESIAN_POINT('',(0.0118532676421069,0.0148782502110272,0.0400393259823159));
#37837=CARTESIAN_POINT('',(0.0119573719452351,0.0150082890904317,0.0400676883273018));
#37838=CARTESIAN_POINT('',(0.0125544556346826,0.0142906873536392,0.0398473241536116));
#37839=CARTESIAN_POINT('',(0.0125577009027439,0.0142878293504653,0.0400162524377134));
#37840=CARTESIAN_POINT('',(0.0126682600067235,0.0144127392115931,0.040044455699943));
#37841=CARTESIAN_POINT('',(0.0138702467674847,0.0130174634983839,0.0398012190609471));
#37842=CARTESIAN_POINT('',(0.0138731763361025,0.0130143463746749,0.0399702245532373));
#37843=CARTESIAN_POINT('',(0.0139952835666706,0.0131281092670227,0.0399983668028166));
#37844=CARTESIAN_POINT('',(0.014481306834379,0.0123345873702583,0.0397784453084914));
#37845=CARTESIAN_POINT('',(0.0144838228841967,0.012331656650006,0.0399472909001995));
#37846=CARTESIAN_POINT('',(0.0146113743771591,0.0124389662669217,0.0399755604113871));
#37847=CARTESIAN_POINT('',(0.0153260921123727,0.0112393715958483,0.0397439245227315));
#37848=CARTESIAN_POINT('',(0.0153285096105525,0.0112360719338832,0.0399125601214955));
#37849=CARTESIAN_POINT('',(0.0154630920701157,0.0113337979723908,0.039940999371801));
#37850=CARTESIAN_POINT('',(0.0155966863258303,0.0108608051472629,0.0397323104378551));
#37851=CARTESIAN_POINT('',(0.0155990470192725,0.0108574170854443,0.039900884452663));
#37852=CARTESIAN_POINT('',(0.0157359025015417,0.0109518057717685,0.0399293731818519));
#37853=CARTESIAN_POINT('',(0.0161064285816707,0.0100894336380538,0.0397091645442032));
#37854=CARTESIAN_POINT('',(0.0161086256317495,0.0100859246916167,0.039877665024853));
#37855=CARTESIAN_POINT('',(0.0162498417096541,0.0101734992112851,0.0399062124401483));
#37856=CARTESIAN_POINT('',(0.0163459130563638,0.00969647156966717,0.0396976246968182));
#37857=CARTESIAN_POINT('',(0.0163480572635308,0.0096928566267872,0.0398661107170753));
#37858=CARTESIAN_POINT('',(0.0164913098660663,0.00977702593089619,0.0398946698174529));
#37859=CARTESIAN_POINT('',(0.0170192632791019,0.00849625891948276,0.039663001559238));
#37860=CARTESIAN_POINT('',(0.0170211738557721,0.00849243937980604,0.0398315233381999));
#37861=CARTESIAN_POINT('',(0.0171702868223079,0.00856614567002418,0.039860053468202));
#37862=CARTESIAN_POINT('',(0.017408256052215,0.00766779115074893,0.0396399001523585));
#37863=CARTESIAN_POINT('',(0.017410054063016,0.0076636774840293,0.0398085548241078));
#37864=CARTESIAN_POINT('',(0.01756261565577,0.00773038834989212,0.039836979076401));
#37865=CARTESIAN_POINT('',(0.017901776908571,0.00638255305449936,0.0396050998642632));
#37866=CARTESIAN_POINT('',(0.0179032179134461,0.00637851585957844,0.0397739321898089));
#37867=CARTESIAN_POINT('',(0.018060308309342,0.0064338436493023,0.0398022128536858));
#37868=CARTESIAN_POINT('',(0.0180512316794584,0.00594702367635226,0.039593478757892));
#37869=CARTESIAN_POINT('',(0.0180525517787113,0.00594301535819439,0.0397623614354607));
#37870=CARTESIAN_POINT('',(0.018211010758672,0.00599448261796389,0.039790601447071));
#37871=CARTESIAN_POINT('',(0.0183192930082589,0.00506137920236497,0.0395702177801257));
#37872=CARTESIAN_POINT('',(0.0183204096468456,0.00505733680610022,0.0397391088448937));
#37873=CARTESIAN_POINT('',(0.01848119299716,0.00510103722662414,0.0397673427472158));
#37874=CARTESIAN_POINT('',(0.0184375671426192,0.00461176875866541,0.039558593934693));
#37875=CARTESIAN_POINT('',(0.0184385674168231,0.00460777563908313,0.0397274423032781));
#37876=CARTESIAN_POINT('',(0.0186003367749354,0.00464745017759764,0.0397557104366488));
#37877=CARTESIAN_POINT('',(0.0187403696193654,0.00326308434116236,0.0395240534487004));
#37878=CARTESIAN_POINT('',(0.0187410285340265,0.00325922569557295,0.039692738761433));
#37879=CARTESIAN_POINT('',(0.0189052541067636,0.00328684376191785,0.0397211373335475));
#37880=CARTESIAN_POINT('',(0.0188754608754345,0.00235697139997309,0.039501263479842));
#37881=CARTESIAN_POINT('',(0.0188759732692699,0.00235290135231658,0.0396697996507904));
#37882=CARTESIAN_POINT('',(0.0190411319121178,0.00237273756414135,0.0396983185594243));
#37883=CARTESIAN_POINT('',(0.0190146343871304,0.000531052317676733,0.0394553276067802));
#37884=CARTESIAN_POINT('',(0.0190147467538104,0.000526926096965941,0.0396237985830803));
#37885=CARTESIAN_POINT('',(0.0191809803724045,0.000530781571160013,0.039652369114602));
#37886=CARTESIAN_POINT('',(0.0190186313319651,-0.000390183701124072,0.0394321458755341));
#37887=CARTESIAN_POINT('',(0.0190185238403849,-0.000394709366226374,0.0396006873315976));
#37888=CARTESIAN_POINT('',(0.0191848667598328,-0.000398521301419501,0.0396292028825932));
#37889=CARTESIAN_POINT('',(0.0188901598408957,-0.00224108059811265,0.039385203330183));
#37890=CARTESIAN_POINT('',(0.0188896397216407,-0.002245594987928,0.0395540134298593));
#37891=CARTESIAN_POINT('',(0.0190550980401844,-0.00226562263151752,0.0395823129296947));
#37892=CARTESIAN_POINT('',(0.0187592919286394,-0.00315070366996476,0.0393619574272701));
#37893=CARTESIAN_POINT('',(0.0187586023982082,-0.00315481802553601,0.0395309559011705));
#37894=CARTESIAN_POINT('',(0.0189230501531979,-0.00318320959294909,0.0395591022467701));
#37895=CARTESIAN_POINT('',(0.0183695100994604,-0.00493954107034915,0.0393160026007698));
#37896=CARTESIAN_POINT('',(0.0183684362350318,-0.00494351963126534,0.0394849528870032));
#37897=CARTESIAN_POINT('',(0.0185293451004069,-0.00498756854556453,0.03951313924705));
#37898=CARTESIAN_POINT('',(0.0181105844945499,-0.00581875143553138,0.0392932469575121));
#37899=CARTESIAN_POINT('',(0.0181094075575356,-0.00582245957346899,0.0394620130085385));
#37900=CARTESIAN_POINT('',(0.0182677162314112,-0.00587435703973338,0.0394903466503783));
#37901=CARTESIAN_POINT('',(0.0176238757386468,-0.00711419627923065,0.0392586871160342));
#37902=CARTESIAN_POINT('',(0.0176223390233472,-0.00711799882055952,0.0394272641248127));
#37903=CARTESIAN_POINT('',(0.0177762141027418,-0.00718095020999036,0.0394557503297173));
#37904=CARTESIAN_POINT('',(0.0174443626195664,-0.0075437181923097,0.0392470527849549));
#37905=CARTESIAN_POINT('',(0.0174427151918118,-0.00754752961849986,0.0394155815388059));
#37906=CARTESIAN_POINT('',(0.017594968480881,-0.0076141672192643,0.0394441065231024));
#37907=CARTESIAN_POINT('',(0.0170570743207949,-0.00838270165178186,0.0392238833103385));
#37908=CARTESIAN_POINT('',(0.017055236896513,-0.0083864394927787,0.0393923701383704));
#37909=CARTESIAN_POINT('',(0.0172040278677065,-0.00846038096201471,0.0394209284103667));
#37910=CARTESIAN_POINT('',(0.0168491312318907,-0.00879301415280329,0.0392123270661835));
#37911=CARTESIAN_POINT('',(0.0168471745089513,-0.00879676231529845,0.0393808173590088));
#37912=CARTESIAN_POINT('',(0.0169941627928814,-0.00887423627012989,0.0394093729459777));
#37913=CARTESIAN_POINT('',(0.0161833521667382,-0.00999701942034864,0.0391776573453862));
#37914=CARTESIAN_POINT('',(0.0161810727591944,-0.0100007222612511,0.0393462289924078));
#37915=CARTESIAN_POINT('',(0.0163223246381786,-0.0100886642409526,0.0393747193412268));
#37916=CARTESIAN_POINT('',(0.0156837813279877,-0.010763917526042,0.0391545287438872));
#37917=CARTESIAN_POINT('',(0.0156812560616843,-0.0107675778681655,0.0393232583031528));
#37918=CARTESIAN_POINT('',(0.0158183322906461,-0.0108622516976936,0.0393516221034215));
#37919=CARTESIAN_POINT('',(0.0148506052656618,-0.0118604490874667,0.0391197539368408));
#37920=CARTESIAN_POINT('',(0.0148479422599114,-0.0118637853368753,0.0392886298438068));
#37921=CARTESIAN_POINT('',(0.0149777130769401,-0.0119682589810861,0.0393168755614208));
#37922=CARTESIAN_POINT('',(0.0145588562855003,-0.0122169562012742,0.0391081591766584));
#37923=CARTESIAN_POINT('',(0.0145561740152432,-0.0122201533101118,0.0392770603641225));
#37924=CARTESIAN_POINT('',(0.0146833441921296,-0.0123278209611957,0.039305285685237));
#37925=CARTESIAN_POINT('',(0.0139465923348996,-0.0129115017488216,0.0390849487544811));
#37926=CARTESIAN_POINT('',(0.013943770796447,-0.0129145481191218,0.0392538016449171));
#37927=CARTESIAN_POINT('',(0.0140655078405243,-0.0130282424901708,0.0392820663107823));
#37928=CARTESIAN_POINT('',(0.0136268604230468,-0.0132484253304702,0.0390733528866772));
#37929=CARTESIAN_POINT('',(0.0136240004475653,-0.0132513693465652,0.0392421472865775));
#37930=CARTESIAN_POINT('',(0.0137428414645763,-0.0133679856135985,0.039270458921805));
#37931=CARTESIAN_POINT('',(0.0126400342360209,-0.0142154116865179,0.0390388473222273));
#37932=CARTESIAN_POINT('',(0.0126371160587943,-0.0142179882435716,0.0392074636684212));
#37933=CARTESIAN_POINT('',(0.01274698114767,-0.0143430328723232,0.0392359174436133));
#37934=CARTESIAN_POINT('',(0.0119408999779254,-0.0148072091698214,0.0390160292372545));
#37935=CARTESIAN_POINT('',(0.0119376451764601,-0.0148098347142087,0.0391845224127175));
#37936=CARTESIAN_POINT('',(0.0120414882136077,-0.014939730316981,0.0392130760164094));
#37937=CARTESIAN_POINT('',(0.0108314094346948,-0.0156169844585444,0.0389815148716734));
#37938=CARTESIAN_POINT('',(0.0108279596023054,-0.0156193773669341,0.0391500085767657));
#37939=CARTESIAN_POINT('',(0.0109220694615437,-0.0157563147823449,0.0391785612300089));
#37940=CARTESIAN_POINT('',(0.0104514076807421,-0.0158738715579762,0.0389699659783551));
#37941=CARTESIAN_POINT('',(0.0104478492511976,-0.0158762130743749,0.0391384844945757));
#37942=CARTESIAN_POINT('',(0.0105386895813438,-0.0160153790697043,0.0391670173443847));
#37943=CARTESIAN_POINT('',(0.00967075750576919,-0.0163611787476578,0.0389467298609994));
#37944=CARTESIAN_POINT('',(0.00966707931299868,-0.0163633545379347,0.03911534247122));
#37945=CARTESIAN_POINT('',(0.00975113060579868,-0.0165068460555297,0.0391437995424063));
#37946=CARTESIAN_POINT('',(0.00926909941956286,-0.0165921264293511,0.038935013836733));
#37947=CARTESIAN_POINT('',(0.00926533905731338,-0.0165942249251055,0.0391036939614964));
#37948=CARTESIAN_POINT('',(0.00934593266447067,-0.0167397810986317,0.0391320968632594));
#37949=CARTESIAN_POINT('',(0.00803891101736719,-0.0172405151791966,0.0388998173571397));
#37950=CARTESIAN_POINT('',(0.00803478692916257,-0.0172424556346622,0.0390687027422972));
#37951=CARTESIAN_POINT('',(0.00810491289056058,-0.0173937454431188,0.0390969418160552));
#37952=CARTESIAN_POINT('',(0.00719694598238467,-0.0176080046398765,0.0388766396692177));
#37953=CARTESIAN_POINT('',(0.00719321072406995,-0.0176095393284872,0.039045666972154));
#37954=CARTESIAN_POINT('',(0.00725554598247917,-0.0177643667872925,0.0390737899638824));
#37955=CARTESIAN_POINT('',(0.00547097376848593,-0.0182182958834193,0.0388308058862709));
#37956=CARTESIAN_POINT('',(0.00546714152685369,-0.0182194370884236,0.0389996812944908));
#37957=CARTESIAN_POINT('',(0.00551426182401809,-0.018379386571311,0.039027927476479));
#37958=CARTESIAN_POINT('',(0.00458696587175252,-0.0184610876513518,0.0388080477807771));
#37959=CARTESIAN_POINT('',(0.00458314615199965,-0.0184620486274569,0.0389767348121234));
#37960=CARTESIAN_POINT('',(0.00462238824093536,-0.0186238693783744,0.039005132143214));
#37961=CARTESIAN_POINT('',(0.0032286360895248,-0.0187293596339089,0.0387734340207107));
#37962=CARTESIAN_POINT('',(0.00322457741815377,-0.0187300579773913,0.0389419651805177));
#37963=CARTESIAN_POINT('',(0.00325205678091437,-0.0188939719824896,0.0389704880835262));
#37964=CARTESIAN_POINT('',(0.00276884731162698,-0.018802838132047,0.0387617786153882));
#37965=CARTESIAN_POINT('',(0.0027647144737126,-0.0188034470080187,0.0389302774843512));
#37966=CARTESIAN_POINT('',(0.00278821639135257,-0.0189679407842008,0.0389588263645261));
#37967=CARTESIAN_POINT('',(0.00185214901521399,-0.0189151468744101,0.0387385824745361));
#37968=CARTESIAN_POINT('',(0.00184797733394435,-0.0189155554236529,0.0389070729772705));
#37969=CARTESIAN_POINT('',(0.00186345704344516,-0.0190809879811251,0.0389356282183146));
#37970=CARTESIAN_POINT('',(0.00139400895517379,-0.0189543386481495,0.0387270101188289));
#37971=CARTESIAN_POINT('',(0.00138976923310706,-0.018954649465271,0.0388955215664241));
#37972=CARTESIAN_POINT('',(0.00140129624287683,-0.0191204303942124,0.038924060100892));
#37973=CARTESIAN_POINT('',(2.02044472024443E-5,-0.0190221042475243,0.0386923001021622));
#37974=CARTESIAN_POINT('',(1.57892815349546E-5,-0.0190221186024429,0.038860932720944));
#37975=CARTESIAN_POINT('',(1.54463184923638E-5,-0.0191885778823327,0.0388893743542784));
#37976=CARTESIAN_POINT('',(-0.000894847146022175,-0.0190011239467331,0.0386691556625014));
#37977=CARTESIAN_POINT('',(-0.000899209950171493,-0.019000911146055,0.0388379620111464));
#37978=CARTESIAN_POINT('',(-0.000907622778345695,-0.0191673736523758,0.0388662636778043));
#37979=CARTESIAN_POINT('',(-0.00226619172341018,-0.0188699560342946,0.0386344327853979));
#37980=CARTESIAN_POINT('',(-0.00227039970073797,-0.0188694512736974,0.0388033310914829));
#37981=CARTESIAN_POINT('',(-0.00229093120188463,-0.0190348059068781,0.0388315589464256));
#37982=CARTESIAN_POINT('',(-0.00272310077466777,-0.0188095535313365,0.0386228755156377));
#37983=CARTESIAN_POINT('',(-0.00272719692133164,-0.0188089615890709,0.0387917624583608));
#37984=CARTESIAN_POINT('',(-0.00275181268614869,-0.0189737424064369,0.0388199994159973));
#37985=CARTESIAN_POINT('',(-0.00363649386734613,-0.0186545033230575,0.0385996963066169));
#37986=CARTESIAN_POINT('',(-0.00364054066666757,-0.0186537130073739,0.038768495053176));
#37987=CARTESIAN_POINT('',(-0.00367313781043775,-0.0188170009701307,0.0387968032840231));
#37988=CARTESIAN_POINT('',(-0.00409075605437804,-0.0185601084600659,0.0385881226133647));
#37989=CARTESIAN_POINT('',(-0.0040947621471106,-0.0185592271993151,0.0387568547743207));
#37990=CARTESIAN_POINT('',(-0.00413133684550116,-0.018721587751719,0.0387852164985522));
#37991=CARTESIAN_POINT('',(-0.0054318056149998,-0.0182302806435945,0.0385536307897916));
#37992=CARTESIAN_POINT('',(-0.00543553993399363,-0.0182291542340229,0.0387221874031463));
#37993=CARTESIAN_POINT('',(-0.00548399425265249,-0.018388326153721,0.0387506890170043));
#37994=CARTESIAN_POINT('',(-0.00630289095283724,-0.0179474880114046,0.0385307760697278));
#37995=CARTESIAN_POINT('',(-0.00630691296692065,-0.0179460723628009,0.0386992425394241));
#37996=CARTESIAN_POINT('',(-0.00636260342768857,-0.0181027456265969,0.0387278177568434));
#37997=CARTESIAN_POINT('',(-0.00757562532439882,-0.0174304214239084,0.0384961973636378));
#37998=CARTESIAN_POINT('',(-0.00757950058939342,-0.0174287378520263,0.0386647159219878));
#37999=CARTESIAN_POINT('',(-0.00764637739074726,-0.017580874673372,0.038693248565823));
#38000=CARTESIAN_POINT('',(-0.00799419906197303,-0.0172425253962202,0.0384846255795232));
#38001=CARTESIAN_POINT('',(-0.00799808179991143,-0.0172407235900233,0.0386531854624822));
#38002=CARTESIAN_POINT('',(-0.00806858952341075,-0.0173912690974159,0.0386816850418112));
#38003=CARTESIAN_POINT('',(-0.00881982373767343,-0.0168351599314685,0.0384613513896509));
#38004=CARTESIAN_POINT('',(-0.0088236265238929,-0.0168331696460589,0.0386300286865617));
#38005=CARTESIAN_POINT('',(-0.00890140257395309,-0.016980241638005,0.0386584337931134));
#38006=CARTESIAN_POINT('',(-0.0092281569464443,-0.0166149242814184,0.0384496112284667));
#38007=CARTESIAN_POINT('',(-0.00923192123330994,-0.0166128313434524,0.0386183634345208));
#38008=CARTESIAN_POINT('',(-0.00931329725815699,-0.0167580465585342,0.0386467083577091));
#38009=CARTESIAN_POINT('',(-0.0104262512167785,-0.0159107398818068,0.0384144447107859));
#38010=CARTESIAN_POINT('',(-0.010430058486001,-0.0159082629531776,0.038583395354492));
#38011=CARTESIAN_POINT('',(-0.0105218200738479,-0.0160475866150257,0.0386115819744312));
#38012=CARTESIAN_POINT('',(-0.0111817027229834,-0.0153885444447047,0.0383913655628602));
#38013=CARTESIAN_POINT('',(-0.011184900762079,-0.0153862348573815,0.0385603823310762));
#38014=CARTESIAN_POINT('',(-0.0112837736795533,-0.0155206792071819,0.0385885137817382));
#38015=CARTESIAN_POINT('',(-0.0126091384792972,-0.014242450727376,0.0383456160376428));
#38016=CARTESIAN_POINT('',(-0.0126120620289027,-0.0142398454093418,0.0385144101986019));
#38017=CARTESIAN_POINT('',(-0.0127232467361194,-0.0143639888582395,0.0385427214008471));
#38018=CARTESIAN_POINT('',(-0.0132811162660052,-0.0136185486283295,0.0383228413906641));
#38019=CARTESIAN_POINT('',(-0.0132839880962257,-0.0136157600325511,0.0384914554416962));
#38020=CARTESIAN_POINT('',(-0.0134008120630799,-0.0137342997068811,0.0385199115843236));
#38021=CARTESIAN_POINT('',(-0.0145393021716353,-0.0122662793207722,0.0382766022493712));
#38022=CARTESIAN_POINT('',(-0.0145418913362455,-0.0122631986723181,0.0384450692067015));
#38023=CARTESIAN_POINT('',(-0.0146695491666348,-0.0123697456593811,0.0384736427431037));
#38024=CARTESIAN_POINT('',(-0.0151238750047054,-0.0115381541874378,0.0382531625212542));
#38025=CARTESIAN_POINT('',(-0.0151265669586711,-0.0115346068146102,0.038421653469323));
#38026=CARTESIAN_POINT('',(-0.0152590825261153,-0.0116351206443961,0.0384502094001571));
#38027=CARTESIAN_POINT('',(-0.015912946196592,-0.0103919821327371,0.0382180073303503));
#38028=CARTESIAN_POINT('',(-0.0159152891678387,-0.0103883973346115,0.0383866624251464));
#38029=CARTESIAN_POINT('',(-0.0160549201441163,-0.0104788084790954,0.038415085410731));
#38030=CARTESIAN_POINT('',(-0.0161622506892229,-0.00999971846528998,0.038206255530585));
#38031=CARTESIAN_POINT('',(-0.016164506233904,-0.00999606979149996,0.0383749782187102));
#38032=CARTESIAN_POINT('',(-0.0163063720435345,-0.0100830863974814,0.0384033468945532));
#38033=CARTESIAN_POINT('',(-0.0166284019221505,-0.00920374740210582,0.0381829405297265));
#38034=CARTESIAN_POINT('',(-0.0166304788976319,-0.0091999980748227,0.0383517776941159));
#38035=CARTESIAN_POINT('',(-0.0167765104297406,-0.00928009400932628,0.038380054478062));
#38036=CARTESIAN_POINT('',(-0.0168459427003453,-0.0087991026560107,0.0381713480300838));
#38037=CARTESIAN_POINT('',(-0.01684789442206,-0.00879536529539895,0.0383402335991688));
#38038=CARTESIAN_POINT('',(-0.0169958968586454,-0.00887187768206122,0.0383684712909901));
#38039=CARTESIAN_POINT('',(-0.0174528532182407,-0.00756557245685109,0.038136798429106));
#38040=CARTESIAN_POINT('',(-0.0174545163799049,-0.00756173319037529,0.0383056887441116));
#38041=CARTESIAN_POINT('',(-0.0176077926838441,-0.00762742152354258,0.0383339236141263));
#38042=CARTESIAN_POINT('',(-0.0177967463233965,-0.00671719229774001,0.0381140518336256));
#38043=CARTESIAN_POINT('',(-0.0177981441576787,-0.00671352296714926,0.0382827768219074));
#38044=CARTESIAN_POINT('',(-0.0179542998344343,-0.00677144528966483,0.0383111435427684));
#38045=CARTESIAN_POINT('',(-0.0183620354818313,-0.00496794776825526,0.0380681118033921));
#38046=CARTESIAN_POINT('',(-0.018363051915718,-0.00496414667738891,0.0382366207910613));
#38047=CARTESIAN_POINT('',(-0.0185238543331827,-0.0050066603498049,0.038265160581824));
#38048=CARTESIAN_POINT('',(-0.0185837873782487,-0.00406064450754518,0.0380447542023251));
#38049=CARTESIAN_POINT('',(-0.0185847093982919,-0.00405639286329004,0.0382132118941942));
#38050=CARTESIAN_POINT('',(-0.0187472682210555,-0.00409134689971549,0.0382417943471708));
#38051=CARTESIAN_POINT('',(-0.0188891167679676,-0.00224660963736494,0.0379983688731513));
#38052=CARTESIAN_POINT('',(-0.0188896422389133,-0.00224226097750333,0.0381669629359119));
#38053=CARTESIAN_POINT('',(-0.019054959181508,-0.00226136487600709,0.038195435365985));
#38054=CARTESIAN_POINT('',(-0.018975165678065,-0.0013350944840303,0.0379752144272462));
#38055=CARTESIAN_POINT('',(-0.0189754684707854,-0.00133060510680013,0.0381439802865186));
#38056=CARTESIAN_POINT('',(-0.0191417252033731,-0.0013418586227537,0.0381723150679244));
#38057=CARTESIAN_POINT('',(-0.0190054818029713,3.88443657746849E-5,0.0379404708993792));
#38058=CARTESIAN_POINT('',(-0.0190054745100075,4.31324813444525E-5,0.038109416100263));
#38059=CARTESIAN_POINT('',(-0.019172150328964,4.41105638862011E-5,0.038137605958912));
#38060=CARTESIAN_POINT('',(-0.0189990633653289,0.0004979394949072,0.0379288939423862));
#38061=CARTESIAN_POINT('',(-0.0189989535531816,0.000502132561226291,0.0380978803450399));
#38062=CARTESIAN_POINT('',(-0.0191656014577857,0.000507218265721521,0.0381260369267217));
#38063=CARTESIAN_POINT('',(-0.0189525853241847,0.00141840122316238,0.0379057637185006));
#38064=CARTESIAN_POINT('',(-0.0189522734866402,0.00142255874284645,0.0380747227358514));
#38065=CARTESIAN_POINT('',(-0.0191184478191296,0.00143571143768376,0.0381029019710031));
#38066=CARTESIAN_POINT('',(-0.0189122530979747,0.00188166508702157,0.037894151408753));
#38067=CARTESIAN_POINT('',(-0.0189118489177943,0.00188574527054257,0.038063053667648));
#38068=CARTESIAN_POINT('',(-0.0190775767604459,0.00190301444061339,0.0380912784925379));
#38069=CARTESIAN_POINT('',(-0.0187412890444881,0.00325883536209297,0.0378595082246926));
#38070=CARTESIAN_POINT('',(-0.0187406125358451,0.00326263690836655,0.0380282153208414));
#38071=CARTESIAN_POINT('',(-0.0189045331436087,0.0032921695621697,0.0380565962252799));
#38072=CARTESIAN_POINT('',(-0.0185618374760872,0.00415882992177338,0.0378366889422303));
#38073=CARTESIAN_POINT('',(-0.0185609491431853,0.00416281716727193,0.0380052367866357));
#38074=CARTESIAN_POINT('',(-0.0187231061596535,0.00419996532698986,0.0380337462943037));
#38075=CARTESIAN_POINT('',(-0.0180761523716431,0.00592371439588828,0.0377907874534993));
#38076=CARTESIAN_POINT('',(-0.0180748688338159,0.00592761944990612,0.0379592560582077));
#38077=CARTESIAN_POINT('',(-0.0182326246185282,0.00598016232025265,0.0379878284457428));
#38078=CARTESIAN_POINT('',(-0.0177699181807482,0.00678860415922227,0.0377677064269697));
#38079=CARTESIAN_POINT('',(-0.0177683037398952,0.0067927937783899,0.0379362404139646));
#38080=CARTESIAN_POINT('',(-0.0179235668226707,0.00685257390989074,0.0379647618166968));
#38081=CARTESIAN_POINT('',(-0.0172124925922568,0.00805877679345812,0.0377326384506189));
#38082=CARTESIAN_POINT('',(-0.0172106741003609,0.00806266492587303,0.0379013568168212));
#38083=CARTESIAN_POINT('',(-0.0173611188275609,0.00813380938310562,0.0379297289888462));
#38084=CARTESIAN_POINT('',(-0.0170100440513287,0.00847767119971143,0.0377208747988973));
#38085=CARTESIAN_POINT('',(-0.0170081349381613,0.00848149858679464,0.0378896612092541));
#38086=CARTESIAN_POINT('',(-0.0171568587931086,0.00855635316807159,0.0379179786338746));
#38087=CARTESIAN_POINT('',(-0.0165788942837513,0.00929261921778571,0.0376975970371511));
#38088=CARTESIAN_POINT('',(-0.0165768089937421,0.00929634189729705,0.0378664761540591));
#38089=CARTESIAN_POINT('',(-0.0167218201734232,0.00937836824818123,0.0378947193042335));
#38090=CARTESIAN_POINT('',(-0.0163494612799744,0.00969046055170924,0.0376860418887991));
#38091=CARTESIAN_POINT('',(-0.0163473352581449,0.00969404843687843,0.0378549427356594));
#38092=CARTESIAN_POINT('',(-0.0164902999149588,0.00977963570563989,0.0378831683516885));
#38093=CARTESIAN_POINT('',(-0.0156203482955152,0.0108556141477693,0.0376515924539111));
#38094=CARTESIAN_POINT('',(-0.0156180284090897,0.0108589406749027,0.0378204180917313));
#38095=CARTESIAN_POINT('',(-0.0157544376251322,0.0109547386773052,0.0378487044876896));
#38096=CARTESIAN_POINT('',(-0.0150800660109407,0.0115947011823282,0.0376288479886084));
#38097=CARTESIAN_POINT('',(-0.0150776530141183,0.0115978559373221,0.0377975020919996));
#38098=CARTESIAN_POINT('',(-0.0152090726333725,0.0117000441151153,0.0378259259415872));
#38099=CARTESIAN_POINT('',(-0.0138899671273516,0.0129967034129007,0.0375828447234847));
#38100=CARTESIAN_POINT('',(-0.0138872362715129,0.012999608535133,0.0377513232998163));
#38101=CARTESIAN_POINT('',(-0.0140080363523487,0.0131138898465719,0.0377798875104862));
#38102=CARTESIAN_POINT('',(-0.0132352395046215,0.0136628607595305,0.0375594358076555));
#38103=CARTESIAN_POINT('',(-0.0132320559776592,0.0136659307572992,0.0377279052139145));
#38104=CARTESIAN_POINT('',(-0.0133474072445037,0.01378571121355,0.0377564784160232));
#38105=CARTESIAN_POINT('',(-0.0118541866040858,0.0148769482366017,0.0375130004253377));
#38106=CARTESIAN_POINT('',(-0.0118507133088228,0.0148797301405445,0.037681662651709));
#38107=CARTESIAN_POINT('',(-0.0119540859306551,0.0150102460804287,0.0377100805846133));
#38108=CARTESIAN_POINT('',(-0.0111245971527733,0.0154299398798176,0.0374898310539834));
#38109=CARTESIAN_POINT('',(-0.0111210000172843,0.0154325211989581,0.0376586824095242));
#38110=CARTESIAN_POINT('',(-0.0112180880535137,0.0155680677046641,0.0376869480447593));
#38111=CARTESIAN_POINT('',(-0.00997220227959034,0.0161791566010563,0.0374551387958382));
#38112=CARTESIAN_POINT('',(-0.00996857621133361,0.0161813926709487,0.0376241191859782));
#38113=CARTESIAN_POINT('',(-0.0100554962773422,0.0163236603376851,0.0376522808569229));
#38114=CARTESIAN_POINT('',(-0.00957836420746147,0.0164154651534365,0.0374436011601459));
#38115=CARTESIAN_POINT('',(-0.00957477908506208,0.0164175580583187,0.0376125866569281));
#38116=CARTESIAN_POINT('',(-0.00965815868034406,0.016561933580948,0.0376407441702482));
#38117=CARTESIAN_POINT('',(-0.0087709104510153,0.0168607143073696,0.0374205183467233));
#38118=CARTESIAN_POINT('',(-0.00876724454505143,0.0168626198141756,0.0375894250550103));
#38119=CARTESIAN_POINT('',(-0.00884348370640528,0.0170107899134816,0.0376176464448556));
#38120=CARTESIAN_POINT('',(-0.00835552574480931,0.0170704106985969,0.0374089138537229));
#38121=CARTESIAN_POINT('',(-0.00835185234045116,0.0170722108662611,0.0375777503312692));
#38122=CARTESIAN_POINT('',(-0.00842437110571596,0.0172221429219192,0.0376060281742487));
#38123=CARTESIAN_POINT('',(-0.00709535000394028,0.0176496724016442,0.0373743041538517));
#38124=CARTESIAN_POINT('',(-0.00709177332643238,0.017651093352714,0.0375429359937664));
#38125=CARTESIAN_POINT('',(-0.00715290993974597,0.0178059340849104,0.0375713771896712));
#38126=CARTESIAN_POINT('',(-0.00623594483585662,0.0179708283088807,0.0373514569820704));
#38127=CARTESIAN_POINT('',(-0.00623201002423933,0.0179721951179589,0.0375199580659789));
#38128=CARTESIAN_POINT('',(-0.0062858482836886,0.018129549085295,0.0375485052860181));
#38129=CARTESIAN_POINT('',(-0.00447973693691539,0.0184870126055874,0.0373054773677039));
#38130=CARTESIAN_POINT('',(-0.00447566124786949,0.0184880002476111,0.0374739656879611));
#38131=CARTESIAN_POINT('',(-0.00451411766434778,0.0186497894895065,0.0375025224533009));
#38132=CARTESIAN_POINT('',(-0.00358293467330361,0.0186820427185273,0.0372823466294694));
#38133=CARTESIAN_POINT('',(-0.00357850782552124,0.0186828778714969,0.0374509379058908));
#38134=CARTESIAN_POINT('',(-0.00360943877298218,0.0188464195850049,0.037479413249492));
#38135=CARTESIAN_POINT('',(-0.00220875574312944,0.0188768491364344,0.0372472514308504));
#38136=CARTESIAN_POINT('',(-0.00220449059337534,0.0188773499285656,0.0374160326403601));
#38137=CARTESIAN_POINT('',(-0.0022232067701182,0.0190427855844601,0.0374443543460284));
#38138=CARTESIAN_POINT('',(-0.00174634370278357,0.0189251840013327,0.0372355034658549));
#38139=CARTESIAN_POINT('',(-0.00174210867013681,0.0189255738019317,0.0374043467624972));
#38140=CARTESIAN_POINT('',(-0.00175674155373469,0.0190914932990551,0.0374326184330959));
#38141=CARTESIAN_POINT('',(-0.000826925959229854,0.0189875880319355,0.0372122807955014));
#38142=CARTESIAN_POINT('',(-0.000822695137451099,0.018987772823908,0.0373811798831107));
#38143=CARTESIAN_POINT('',(-0.000829275233720999,0.0191542684591979,0.037409407128447));
#38144=CARTESIAN_POINT('',(-0.000368042929881957,0.0190019572021535,0.0372007721319376));
#38145=CARTESIAN_POINT('',(-0.000363906221962559,0.0190020383817323,0.0373696562651259));
#38146=CARTESIAN_POINT('',(-0.000366380226777539,0.0191686249449107,0.0373978955030339));
#38147=CARTESIAN_POINT('',(0.00100616796991394,0.0189954457294153,0.0371663944497608));
#38148=CARTESIAN_POINT('',(0.00101012857597821,0.0189952254684106,0.0373351479087102));
#38149=CARTESIAN_POINT('',(0.00101984822205786,0.0191615481916715,0.0373634919782864));
#38150=CARTESIAN_POINT('',(0.00191906942536007,0.0189252033176999,0.0371436379295908));
#38151=CARTESIAN_POINT('',(0.00192308311659654,0.0189248035834472,0.0373122263406783));
#38152=CARTESIAN_POINT('',(0.00194071232178894,0.0190902698078212,0.0373407031328573));
#38153=CARTESIAN_POINT('',(0.00373829288974369,0.0186513086496933,0.0370975552521172));
#38154=CARTESIAN_POINT('',(0.0037422675429787,0.0186505057536746,0.0372660211976757));
#38155=CARTESIAN_POINT('',(0.00377577997758983,0.0188133693612429,0.0372945956264843));
#38156=CARTESIAN_POINT('',(0.00464927567758443,0.0184452957233617,0.0370740963463626));
#38157=CARTESIAN_POINT('',(0.00465361877516417,0.0184441880652167,0.0372425962806732));
#38158=CARTESIAN_POINT('',(0.00469469620446711,0.0186053679006123,0.0372711450893036));
#38159=CARTESIAN_POINT('',(0.00640788824246925,0.0179104345821219,0.0370276234011098));
#38160=CARTESIAN_POINT('',(0.00641213455974086,0.0179089297463029,0.0371963613560363));
#38161=CARTESIAN_POINT('',(0.00646865877424517,0.0180656268478557,0.037224718661612));
#38162=CARTESIAN_POINT('',(0.00726207630727607,0.0175813053681433,0.0370044523100431));
#38163=CARTESIAN_POINT('',(0.00726606320926511,0.0175796532564351,0.037173385881105));
#38164=CARTESIAN_POINT('',(0.00733032923813791,0.0177335936136366,0.0372015848501821));
#38165=CARTESIAN_POINT('',(0.00850599272108748,0.0169958259732782,0.0369698402137862));
#38166=CARTESIAN_POINT('',(0.00850976493640867,0.0169939382644222,0.0371388274221191));
#38167=CARTESIAN_POINT('',(0.00858499122493516,0.0171427289552142,0.0371669838066493));
#38168=CARTESIAN_POINT('',(0.00891438003054646,0.0167853089728822,0.0369583414018185));
#38169=CARTESIAN_POINT('',(0.00891801964524323,0.0167833776381234,0.0371272959471482));
#38170=CARTESIAN_POINT('',(0.00899687630653875,0.0169302306085211,0.0371554785530948));
#38171=CARTESIAN_POINT('',(0.00971840175291147,0.016332955519842,0.0369352875453021));
#38172=CARTESIAN_POINT('',(0.00972192944744112,0.0163308544625574,0.0371041284248019));
#38173=CARTESIAN_POINT('',(0.00980775423010033,0.0164735976811781,0.0371324027994236));
#38174=CARTESIAN_POINT('',(0.010115519109279,0.0160900516915207,0.0369236852535701));
#38175=CARTESIAN_POINT('',(0.0101189831416029,0.0160878761573662,0.0370924497054347));
#38176=CARTESIAN_POINT('',(0.0102082411546516,0.0162283894770379,0.0371207855168135));
#38177=CARTESIAN_POINT('',(0.011270743586706,0.0153239779478668,0.0368890886031778));
#38178=CARTESIAN_POINT('',(0.0112738475288275,0.0153216765286443,0.0370576557087243));
#38179=CARTESIAN_POINT('',(0.0113732583737178,0.0154551150530701,0.0370861487868824));
#38180=CARTESIAN_POINT('',(0.0119960433226631,0.0147625421329569,0.0368662057002651));
#38181=CARTESIAN_POINT('',(0.0119993377869907,0.0147598621502207,0.0370346769756178));
#38182=CARTESIAN_POINT('',(0.0121047025895979,0.0148884994495844,0.0370632482888409));
#38183=CARTESIAN_POINT('',(0.0133594794395941,0.0135411230970551,0.0368201469046876));
#38184=CARTESIAN_POINT('',(0.0133625258969465,0.0135381225996254,0.0369886716378074));
#38185=CARTESIAN_POINT('',(0.0134798097341667,0.0136560742344555,0.0370171994129493));
#38186=CARTESIAN_POINT('',(0.0139976186714959,0.01288114301712,0.0367969732272835));
#38187=CARTESIAN_POINT('',(0.0140006506527497,0.0128778290839074,0.0369656331369593));
#38188=CARTESIAN_POINT('',(0.0141234832663436,0.0129902601921686,0.0369940531835233));
#38189=CARTESIAN_POINT('',(0.0148871651265421,0.0118146776498597,0.0367618712903768));
#38190=CARTESIAN_POINT('',(0.0148898311117952,0.0118113208332762,0.0369307085403116));
#38191=CARTESIAN_POINT('',(0.0150206911999236,0.0119143565375086,0.0369589852579205));
#38192=CARTESIAN_POINT('',(0.0151714138970381,0.0114472840332302,0.0367501501470596));
#38193=CARTESIAN_POINT('',(0.0151739527294179,0.0114439186647624,0.0369190362901996));
#38194=CARTESIAN_POINT('',(0.0153073745596128,0.0115437077107914,0.0369472735194286));
#38195=CARTESIAN_POINT('',(0.0157082289777055,0.0106987687962991,0.0367270025048148));
#38196=CARTESIAN_POINT('',(0.0157105865147794,0.0106953068463507,0.0368958908144695));
#38197=CARTESIAN_POINT('',(0.0158486853398397,0.0107885189926399,0.0369241269577371));
#38198=CARTESIAN_POINT('',(0.0159619428674269,0.0103163047026149,0.0367155289826961));
#38199=CARTESIAN_POINT('',(0.0159641782183735,0.0103128486834407,0.036884373293912));
#38200=CARTESIAN_POINT('',(0.0161044773088418,0.0104026139781047,0.0369126447041816));
#38201=CARTESIAN_POINT('',(0.0166797308494157,0.00914470502924076,0.0366811972170258));
#38202=CARTESIAN_POINT('',(0.0166816017193964,0.00914126628356073,0.0368498775850132));
#38203=CARTESIAN_POINT('',(0.0168280801599711,0.00922047590564887,0.0368782801257313));
#38204=CARTESIAN_POINT('',(0.0171006766352299,0.00833148822032756,0.0366584160864228));
#38205=CARTESIAN_POINT('',(0.0171024790722256,0.00832779764663219,0.0368269487267926));
#38206=CARTESIAN_POINT('',(0.017252357518434,0.00839995519488384,0.0368554704816954));
#38207=CARTESIAN_POINT('',(0.0176445139573953,0.00706277824544435,0.0366237857316965));
#38208=CARTESIAN_POINT('',(0.0176460648564801,0.00705890305230766,0.0367922715457667));
#38209=CARTESIAN_POINT('',(0.0178005846173115,0.00711997051471082,0.0368208306062401));
#38210=CARTESIAN_POINT('',(0.0178114967886425,0.00663064607588128,0.0366121409164746));
#38211=CARTESIAN_POINT('',(0.0178129748056691,0.00662667350514105,0.0367806354324629));
#38212=CARTESIAN_POINT('',(0.0179689296391234,0.00668401444243181,0.0368091876132652));
#38213=CARTESIAN_POINT('',(0.0181136579656142,0.00575415331218789,0.0365887630218576));
#38214=CARTESIAN_POINT('',(0.0181149468808211,0.00575009966218317,0.0367573264175973));
#38215=CARTESIAN_POINT('',(0.0182735869117889,0.0057997897582315,0.0367858230275019));
#38216=CARTESIAN_POINT('',(0.0182478310032561,0.00531297353456236,0.0365771140207169));
#38217=CARTESIAN_POINT('',(0.018249030517764,0.00530884742971662,0.0367457347909464));
#38218=CARTESIAN_POINT('',(0.0184088854457252,0.00535472955377455,0.0367741854134964));
#38219=CARTESIAN_POINT('',(0.018600988193285,0.00398087109094014,0.0365422440402653));
#38220=CARTESIAN_POINT('',(0.0186019530843162,0.00397643426041515,0.0367110601598061));
#38221=CARTESIAN_POINT('',(0.0187650148720769,0.00401092391464825,0.0367393548042703));
#38222=CARTESIAN_POINT('',(0.0187708608753656,0.00308142894533311,0.0365190923932619));
#38223=CARTESIAN_POINT('',(0.0187715368712848,0.00307732305295663,0.0366880943303872));
#38224=CARTESIAN_POINT('',(0.0189363401960049,0.00310359636864942,0.0367162378719251));
#38225=CARTESIAN_POINT('',(0.0189279634989396,0.00171531436468066,0.0364845827643801));
#38226=CARTESIAN_POINT('',(0.0189283390501015,0.00171116260852284,0.0366535411453261));
#38227=CARTESIAN_POINT('',(0.0190944145090531,0.00172549529433406,0.0366817208931037));
#38228=CARTESIAN_POINT('',(0.018963983478816,0.00125710692474757,0.0364731051806145));
#38229=CARTESIAN_POINT('',(0.0189642564545632,0.00125301548742518,0.0366420074484449));
#38230=CARTESIAN_POINT('',(0.0191305660401824,0.00126326236653834,0.0366702322676994));
#38231=CARTESIAN_POINT('',(0.0190026530986991,0.00033490657735888,0.0364500633580356));
#38232=CARTESIAN_POINT('',(0.0190027232547102,0.000330815741490651,0.0366188320274701));
#38233=CARTESIAN_POINT('',(0.0191691840164528,0.00033297175633165,0.0366471644579997));
#38234=CARTESIAN_POINT('',(0.019005161708661,-0.000130707036364811,0.0364384584739173));
#38235=CARTESIAN_POINT('',(0.0190051352620632,-0.000134805107419141,0.0366071509145178));
#38236=CARTESIAN_POINT('',(0.0191715078304247,-0.000136721059686821,0.0366355446099033));
#38237=CARTESIAN_POINT('',(0.018961975556038,-0.00151542291755907,0.0364038573031784));
#38238=CARTESIAN_POINT('',(0.0189616516139013,-0.0015193124786197,0.036572373712744));
#38239=CARTESIAN_POINT('',(0.0191273800290963,-0.00153354890875932,0.0366009074512625));
#38240=CARTESIAN_POINT('',(0.0188665153486165,-0.0024274179881491,0.0363809331684296));
#38241=CARTESIAN_POINT('',(0.0188659579023432,-0.00243170631394234,0.0365493931119482));
#38242=CARTESIAN_POINT('',(0.0190307969644883,-0.00245349709780482,0.0365779736750566));
#38243=CARTESIAN_POINT('',(0.018545820612552,-0.00422969234056243,0.0363347989938727));
#38244=CARTESIAN_POINT('',(0.0185448595612686,-0.00423393749797188,0.0365033744097998));
#38245=CARTESIAN_POINT('',(0.0187069583442499,-0.00427150106843692,0.0365318617477388));
#38246=CARTESIAN_POINT('',(0.0183205926808351,-0.00511997279119293,0.0363115915560491));
#38247=CARTESIAN_POINT('',(0.0183193857280646,-0.00512425118141887,0.03648032703392));
#38248=CARTESIAN_POINT('',(0.0184797066320657,-0.00516956856814049,0.0365086860629788));
#38249=CARTESIAN_POINT('',(0.0178818398582988,-0.00643850624540062,0.0362765066738982));
#38250=CARTESIAN_POINT('',(0.0178803952622417,-0.00644252177524659,0.0364453859504565));
#38251=CARTESIAN_POINT('',(0.0180369260922356,-0.0064995733336445,0.0364736289751795));
#38252=CARTESIAN_POINT('',(0.0177192671303535,-0.00687309947165825,0.0362648324652074));
#38253=CARTESIAN_POINT('',(0.0177177597326137,-0.00687698699387712,0.0364337333983774));
#38254=CARTESIAN_POINT('',(0.0178728419492951,-0.00693792755685441,0.0364619589459061));
#38255=CARTESIAN_POINT('',(0.0173656132613296,-0.00772317292581675,0.0362417572165986));
#38256=CARTESIAN_POINT('',(0.0173639262756046,-0.00772696373847354,0.0364106054406504));
#38257=CARTESIAN_POINT('',(0.0175158214621759,-0.00779531716318344,0.0364388738637441));
#38258=CARTESIAN_POINT('',(0.0171740610956206,-0.0081401059249469,0.0362303035090353));
#38259=CARTESIAN_POINT('',(0.0171723044984121,-0.00814381578093226,0.0363990930090974));
#38260=CARTESIAN_POINT('',(0.0173224233726417,-0.0082158214229691,0.0364274085936535));
#38261=CARTESIAN_POINT('',(0.0165559248141777,-0.00936697120146884,0.0361959942743846));
#38262=CARTESIAN_POINT('',(0.0165539948838148,-0.00937035510245631,0.0363646063064641));
#38263=CARTESIAN_POINT('',(0.0166983735051786,-0.00945317342502582,0.0363930635492081));
#38264=CARTESIAN_POINT('',(0.0160860880286729,-0.010153094424609,0.0361731779386068));
#38265=CARTESIAN_POINT('',(0.016083853004231,-0.0101566361433608,0.0363416684933638));
#38266=CARTESIAN_POINT('',(0.0162241091707267,-0.0102459909534076,0.0363702242164136));
#38267=CARTESIAN_POINT('',(0.0152933608774182,-0.0112838380743594,0.0361384739484449));
#38268=CARTESIAN_POINT('',(0.0152908671216402,-0.0112872183148005,0.0363069689458261));
#38269=CARTESIAN_POINT('',(0.0154241499532452,-0.0113864396905706,0.0363355205556882));
#38270=CARTESIAN_POINT('',(0.0150134609046653,-0.0116537805840718,0.0361267920987623));
#38271=CARTESIAN_POINT('',(0.0150108462100671,-0.0116571471098475,0.0362953136654874));
#38272=CARTESIAN_POINT('',(0.0151417283120323,-0.0117595700123999,0.0363238440647179));
#38273=CARTESIAN_POINT('',(0.0144276705469642,-0.0123716180358861,0.0361033948396687));
#38274=CARTESIAN_POINT('',(0.0144248879956393,-0.0123748653478363,0.0362720137224976));
#38275=CARTESIAN_POINT('',(0.0145507063085901,-0.0124836165091143,0.0363004657579308));
#38276=CARTESIAN_POINT('',(0.0141233515699902,-0.0127177757869468,0.0360917386081692));
#38277=CARTESIAN_POINT('',(0.0141204692867383,-0.0127209738099472,0.036260425760229));
#38278=CARTESIAN_POINT('',(0.0142436908282717,-0.0128327805268058,0.0362888230033628));
#38279=CARTESIAN_POINT('',(0.0131770131949719,-0.0137189593412155,0.0360568696793308));
#38280=CARTESIAN_POINT('',(0.0131737412271933,-0.0137221233895215,0.0362257603444948));
#38281=CARTESIAN_POINT('',(0.0132889779293669,-0.0138426541031448,0.0362539951485338));
#38282=CARTESIAN_POINT('',(0.0125017814668455,-0.0143368853017285,0.0360337816477872));
#38283=CARTESIAN_POINT('',(0.0124987491438331,-0.0143395397828666,0.0362028095268066));
#38284=CARTESIAN_POINT('',(0.0126077753735881,-0.0144659152885397,0.0362309320457858));
#38285=CARTESIAN_POINT('',(0.0114227446193982,-0.0151898357581618,0.0359993506669855));
#38286=CARTESIAN_POINT('',(0.0114194417068658,-0.0151923179076328,0.0361682566460626));
#38287=CARTESIAN_POINT('',(0.0115189958909884,-0.0153259415942862,0.0361964786244854));
#38288=CARTESIAN_POINT('',(0.0110519919396605,-0.0154617814951672,0.0359878837661081));
#38289=CARTESIAN_POINT('',(0.0110486648770015,-0.0154641620043371,0.0361567203751101));
#38290=CARTESIAN_POINT('',(0.0111448792418167,-0.0156001083291818,0.0361849981130821));
#38291=CARTESIAN_POINT('',(0.0102878646876576,-0.0159803958964433,0.0359648386603841));
#38292=CARTESIAN_POINT('',(0.0102844273139459,-0.0159826064635074,0.0361335349989411));
#38293=CARTESIAN_POINT('',(0.0103738367441834,-0.0161229349409537,0.036161925518539));
#38294=CARTESIAN_POINT('',(0.0098932911377497,-0.0162276251860447,0.0359532272935491));
#38295=CARTESIAN_POINT('',(0.00988978065682202,-0.0162297670937197,0.0361218530719544));
#38296=CARTESIAN_POINT('',(0.0099757011286439,-0.0163721603468361,0.0361503002884256));
#38297=CARTESIAN_POINT('',(0.00869387420900978,-0.0169194759404076,0.035918607098746));
#38298=CARTESIAN_POINT('',(0.00869034660227495,-0.0169212768624291,0.0360870893761529));
#38299=CARTESIAN_POINT('',(0.00876551477290953,-0.0170696169282755,0.0361156505378651));
#38300=CARTESIAN_POINT('',(0.00786843804549885,-0.0173183579629828,0.0358956386852973));
#38301=CARTESIAN_POINT('',(0.00786443472044417,-0.0173201673320902,0.0360641062936784));
#38302=CARTESIAN_POINT('',(0.0079327484477341,-0.0174717737992693,0.0360926808363628));
#38303=CARTESIAN_POINT('',(0.00616721922613437,-0.0179945338040935,0.0358494377904948));
#38304=CARTESIAN_POINT('',(0.00616304254324382,-0.0179959756148133,0.0360180747453525));
#38305=CARTESIAN_POINT('',(0.00621652364098048,-0.0181536144369596,0.0360465129090835));
#38306=CARTESIAN_POINT('',(0.00529144001220449,-0.0182718361121899,0.0358262080660678));
#38307=CARTESIAN_POINT('',(0.0052872486792983,-0.0182730424973861,0.0359950206772658));
#38308=CARTESIAN_POINT('',(0.00533305796727003,-0.0184333095392014,0.036023317273135));
#38309=CARTESIAN_POINT('',(0.00393855418278351,-0.0185930800037985,0.0357911672875431));
#38310=CARTESIAN_POINT('',(0.00393441101622293,-0.0185939582056733,0.0359600665272096));
#38311=CARTESIAN_POINT('',(0.00396828548438073,-0.0187571049648598,0.0359882936532595));
#38312=CARTESIAN_POINT('',(0.00348406197957908,-0.0186834968768611,0.0357795515499011));
#38313=CARTESIAN_POINT('',(0.00347999570770636,-0.0186842562470553,0.0359484353312303));
#38314=CARTESIAN_POINT('',(0.00350979662203613,-0.0188481742293118,0.0359766748522456));
#38315=CARTESIAN_POINT('',(0.00257552661300216,-0.0188302524170799,0.0357565296715141));
#38316=CARTESIAN_POINT('',(0.00257144268580103,-0.0188308095699434,0.035925322804152));
#38317=CARTESIAN_POINT('',(0.00259325999889579,-0.0189958767125214,0.0359536355516433));
#38318=CARTESIAN_POINT('',(0.00212033184012026,-0.018886869367471,0.0357450875726116));
#38319=CARTESIAN_POINT('',(0.00211625489474283,-0.0188873287106048,0.0359138145667818));
#38320=CARTESIAN_POINT('',(0.00213405629354057,-0.0190527966293634,0.0359421804492124));
#38321=CARTESIAN_POINT('',(0.000752012093046373,-0.0190071840175358,0.035710780080294));
#38322=CARTESIAN_POINT('',(0.000748109685983577,-0.0190073255153809,0.0358793332535717));
#38323=CARTESIAN_POINT('',(0.000753706604604977,-0.0191736087781649,0.0359078376370782));
#38324=CARTESIAN_POINT('',(-0.000163833649728999,-0.0190216050376802,0.0356879200859886));
#38325=CARTESIAN_POINT('',(-0.000168104459227904,-0.0190215649227648,0.035856385020059));
#38326=CARTESIAN_POINT('',(-0.000170161240575154,-0.0191878298444561,0.035884961489837));
#38327=CARTESIAN_POINT('',(-0.00154313375493487,-0.0189428301246924,0.0356531407796446));
#38328=CARTESIAN_POINT('',(-0.00154734732021483,-0.018942487564402,0.0358216619959281));
#38329=CARTESIAN_POINT('',(-0.00156152930468212,-0.0191080719713565,0.0358501925027523));
#38330=CARTESIAN_POINT('',(-0.00200553802655285,-0.0188995280394954,0.035641425773187));
#38331=CARTESIAN_POINT('',(-0.00200979696251775,-0.0188990745436516,0.0358099902070311));
#38332=CARTESIAN_POINT('',(-0.00202797804982009,-0.0190643219579432,0.0358384861311067));
#38333=CARTESIAN_POINT('',(-0.00292365854862329,-0.0187794186167379,0.0356180154682183));
#38334=CARTESIAN_POINT('',(-0.0029279022118001,-0.0187787597635309,0.0357866999464391));
#38335=CARTESIAN_POINT('',(-0.00295412988974707,-0.0189430592887084,0.0358150992871516));
#38336=CARTESIAN_POINT('',(-0.00337795740793425,-0.0187029448940798,0.0356063569578135));
#38337=CARTESIAN_POINT('',(-0.00338219373654105,-0.0187021778709024,0.0357751163672398));
#38338=CARTESIAN_POINT('',(-0.00341240350341812,-0.0188658828347146,0.0358034554891367));
#38339=CARTESIAN_POINT('',(-0.00472692781808232,-0.0184255021436554,0.0355715087063121));
#38340=CARTESIAN_POINT('',(-0.00473132273337695,-0.0184243896130631,0.035740463350948));
#38341=CARTESIAN_POINT('',(-0.00477316172383682,-0.0185858864378482,0.0357686467238541));
#38342=CARTESIAN_POINT('',(-0.00560774563104161,-0.0181767552827158,0.0355485132903271));
#38343=CARTESIAN_POINT('',(-0.00561151282205915,-0.0181756053784645,0.035717528399292));
#38344=CARTESIAN_POINT('',(-0.00566162890118377,-0.0183347876745961,0.035745661182169));
#38345=CARTESIAN_POINT('',(-0.00690130839944473,-0.0177082538182991,0.0355141335005034));
#38346=CARTESIAN_POINT('',(-0.00690513394921139,-0.0177067610821227,0.0356829736687975));
#38347=CARTESIAN_POINT('',(-0.00696632560854634,-0.0178616695579185,0.0357112486182751));
#38348=CARTESIAN_POINT('',(-0.00732786701516761,-0.0175361287238716,0.0355026692113962));
#38349=CARTESIAN_POINT('',(-0.00733164200843698,-0.017534553312147,0.0356714338948254));
#38350=CARTESIAN_POINT('',(-0.0073965431904294,-0.0176878468471484,0.0356997695200506));
#38351=CARTESIAN_POINT('',(-0.00817151566703478,-0.0171592475742844,0.0354796072250903));
#38352=CARTESIAN_POINT('',(-0.00817520837825819,-0.0171574869932219,0.0356482364567335));
#38353=CARTESIAN_POINT('',(-0.00824742094186209,-0.0173073061966473,0.0356766808108588));
#38354=CARTESIAN_POINT('',(-0.00858934050716055,-0.0169539387269213,0.0354679864751644));
#38355=CARTESIAN_POINT('',(-0.00859302665771972,-0.0169520724615698,0.0356365553227494));
#38356=CARTESIAN_POINT('',(-0.00866882261477138,-0.01710003058645,0.0356650481939536));
#38357=CARTESIAN_POINT('',(-0.00980833503611941,-0.0162987054282184,0.035433336011985));
#38358=CARTESIAN_POINT('',(-0.00981178625827609,-0.016296620164032,0.0356018022451308));
#38359=CARTESIAN_POINT('',(-0.00989827033312281,-0.0164386371414768,0.0356303763771952));
#38360=CARTESIAN_POINT('',(-0.0105818582595534,-0.0158070307930283,0.035410322798043));
#38361=CARTESIAN_POINT('',(-0.0105855487126754,-0.0158045469626697,0.0355788165800883));
#38362=CARTESIAN_POINT('',(-0.010678461477246,-0.0159424955200915,0.0356073702040998));
#38363=CARTESIAN_POINT('',(-0.0120524426450354,-0.0147165407961638,0.0353640686396772));
#38364=CARTESIAN_POINT('',(-0.0120559075893778,-0.0147137185160198,0.0355327736044921));
#38365=CARTESIAN_POINT('',(-0.0121617899069155,-0.0148422678510516,0.0355611573495344));
#38366=CARTESIAN_POINT('',(-0.0127495106129697,-0.0141177348621299,0.0353408302732254));
#38367=CARTESIAN_POINT('',(-0.0127526531198844,-0.0141148948912311,0.0355097152778329));
#38368=CARTESIAN_POINT('',(-0.0128649418112909,-0.0142381832734485,0.0355379531024191));
#38369=CARTESIAN_POINT('',(-0.0140640980308915,-0.0128086535235012,0.035294208453188));
#38370=CARTESIAN_POINT('',(-0.0140669123797478,-0.0128055615864941,0.0354630977749176));
#38371=CARTESIAN_POINT('',(-0.0141906727480833,-0.0129173343768273,0.0354913334496882));
#38372=CARTESIAN_POINT('',(-0.0146674069019048,-0.0121122061437758,0.0352713151253847));
#38373=CARTESIAN_POINT('',(-0.0146699184948938,-0.0121091832973698,0.035440036275915));
#38374=CARTESIAN_POINT('',(-0.0147989395557303,-0.0122144984851512,0.0354684060970901));
#38375=CARTESIAN_POINT('',(-0.0157641239006939,-0.0106456921117857,0.0352255501119424));
#38376=CARTESIAN_POINT('',(-0.0157663186936035,-0.0106424218237481,0.0353940576562385));
#38377=CARTESIAN_POINT('',(-0.0159046881144227,-0.0107347128770398,0.0354225986144043));
#38378=CARTESIAN_POINT('',(-0.0162586300252783,-0.00987451380899395,0.0352026403041944));
#38379=CARTESIAN_POINT('',(-0.0162608829420131,-0.00987079107989347,0.0353710978626173));
#38380=CARTESIAN_POINT('',(-0.0164032860051871,-0.00995663241126164,0.0353996804267765));
#38381=CARTESIAN_POINT('',(-0.0169180517691241,-0.00865978017347781,0.0351677876717183));
#38382=CARTESIAN_POINT('',(-0.016919990653101,-0.00865599475686332,0.0353363508374712));
#38383=CARTESIAN_POINT('',(-0.0170682756651896,-0.00873114150250666,0.0353648476304432));
#38384=CARTESIAN_POINT('',(-0.0171248289518239,-0.0082434408190218,0.0351560446564631));
#38385=CARTESIAN_POINT('',(-0.0171266915858875,-0.00823956726551623,0.0353246654407593));
#38386=CARTESIAN_POINT('',(-0.0172768170667127,-0.008311131019232,0.0353531160574958));
#38387=CARTESIAN_POINT('',(-0.0175057833600715,-0.00740011027729877,0.035132630000989));
#38388=CARTESIAN_POINT('',(-0.0175074618837968,-0.00739614457712032,0.0353013859018486));
#38389=CARTESIAN_POINT('',(-0.017661032054276,-0.00746037704417608,0.0353297278574223));
#38390=CARTESIAN_POINT('',(-0.0176798425091695,-0.00697379259955303,0.0351209752849925));
#38391=CARTESIAN_POINT('',(-0.0176814170602976,-0.00696979623835056,0.0352898076032935));
#38392=CARTESIAN_POINT('',(-0.0178365863050473,-0.00703031247343333,0.0353180880602619));
#38393=CARTESIAN_POINT('',(-0.0181539581319484,-0.0056812200825124,0.0350861705288966));
#38394=CARTESIAN_POINT('',(-0.0181553082467342,-0.00567694642197531,0.0352551707870785));
#38395=CARTESIAN_POINT('',(-0.0183147029008516,-0.00572637091688139,0.0352833174288937));
#38396=CARTESIAN_POINT('',(-0.0184061981139469,-0.00480141276233039,0.035063277094861));
#38397=CARTESIAN_POINT('',(-0.0184071921267651,-0.00479765830709078,0.03523225027595));
#38398=CARTESIAN_POINT('',(-0.0185688744888827,-0.00483879487407327,0.0352604168793913));
#38399=CARTESIAN_POINT('',(-0.0186889294040412,-0.00345461157176816,0.0350289233414967));
#38400=CARTESIAN_POINT('',(-0.018689671368071,-0.00345058715816061,0.0351976913984222));
#38401=CARTESIAN_POINT('',(-0.0188535109674506,-0.00348008264673463,0.0352260243248854));
#38402=CARTESIAN_POINT('',(-0.0187671737170645,-0.00300114582666555,0.0350174544050953));
#38403=CARTESIAN_POINT('',(-0.0187678225433682,-0.00299709954103612,0.035186147134013));
#38404=CARTESIAN_POINT('',(-0.0189322391930674,-0.00302261047148245,0.0352145405972404));
#38405=CARTESIAN_POINT('',(-0.0188909159202362,-0.00208494155648397,0.0349943638038464));
#38406=CARTESIAN_POINT('',(-0.0188913643710508,-0.00208086367720278,0.0351629355397262));
#38407=CARTESIAN_POINT('',(-0.0190566924975937,-0.00209833028062096,0.0351914259662282));
#38408=CARTESIAN_POINT('',(-0.0189362711550871,-0.00162179856622392,0.0349827318494094));
#38409=CARTESIAN_POINT('',(-0.0189366263747109,-0.00161765906985487,0.0351512568869062));
#38410=CARTESIAN_POINT('',(-0.019102274027967,-0.00163111402455153,0.0351797848456837));
#38411=CARTESIAN_POINT('',(-0.0190208368298371,-0.00024114246053665,0.0349480433217033));
#38412=CARTESIAN_POINT('',(-0.0190208853968919,-0.000237030054909648,0.0351165120695049));
#38413=CARTESIAN_POINT('',(-0.0191871591507164,-0.000238336653427598,0.0351450843400414));
#38414=CARTESIAN_POINT('',(-0.0190100560265515,0.000675166803218607,0.0349249873572056));
#38415=CARTESIAN_POINT('',(-0.0190098842172453,0.000679648750286042,0.0350935242556918));
#38416=CARTESIAN_POINT('',(-0.0191761360813997,0.000685993308868359,0.0351220432919113));
#38417=CARTESIAN_POINT('',(-0.0188570830529375,0.00249969979785826,0.0348786981384304));
#38418=CARTESIAN_POINT('',(-0.0188565049119517,0.00250416120399566,0.0350474721130656));
#38419=CARTESIAN_POINT('',(-0.0190216222788578,0.00252648896835062,0.0350758005679836));
#38420=CARTESIAN_POINT('',(-0.0187149048326804,0.00340792494756124,0.0348554874810762));
#38421=CARTESIAN_POINT('',(-0.0187141768543059,0.00341195073388233,0.0350244173224227));
#38422=CARTESIAN_POINT('',(-0.0188781294109306,0.00344264883378809,0.0350526189203356));
#38423=CARTESIAN_POINT('',(-0.0182935911308715,0.0052159504293076,0.0348089597471648));
#38424=CARTESIAN_POINT('',(-0.0182924738681908,0.00521984354838879,0.0349777832279153));
#38425=CARTESIAN_POINT('',(-0.018452547375611,0.00526634224321446,0.0350060713410159));
#38426=CARTESIAN_POINT('',(-0.0180194587189408,0.00609403747428862,0.0347861076178894));
#38427=CARTESIAN_POINT('',(-0.0180181939337391,0.0060978076924339,0.0349547581780811));
#38428=CARTESIAN_POINT('',(-0.0181755974548477,0.00615199150236652,0.0349831848912084));
#38429=CARTESIAN_POINT('',(-0.0173500477454275,0.00779833498209935,0.0347403003356644));
#38430=CARTESIAN_POINT('',(-0.0173484029273116,0.00780197274722938,0.0349087789228932));
#38431=CARTESIAN_POINT('',(-0.0174997017420979,0.00787097230989661,0.0349373431390131));
#38432=CARTESIAN_POINT('',(-0.0169546694139038,0.00862490930693604,0.0347173366651471));
#38433=CARTESIAN_POINT('',(-0.0169526543496618,0.00862884823398127,0.0348858068825127));
#38434=CARTESIAN_POINT('',(-0.0171006519871961,0.00870468149543935,0.0349143794419575));
#38435=CARTESIAN_POINT('',(-0.0162686860858967,0.00982559524458752,0.0346824162041079));
#38436=CARTESIAN_POINT('',(-0.0162664768054821,0.00982925613773177,0.0348510359353158));
#38437=CARTESIAN_POINT('',(-0.0164084926672397,0.00991579353543065,0.0348794872876429));
#38438=CARTESIAN_POINT('',(-0.0160233612223135,0.0102208476249506,0.0346706515686278));
#38439=CARTESIAN_POINT('',(-0.0160210437661859,0.0102244771619029,0.0348393400591364));
#38440=CARTESIAN_POINT('',(-0.016160983761665,0.0103144874313735,0.034867736231845));
#38441=CARTESIAN_POINT('',(-0.0155071783420045,0.0109882323829841,0.0346472437132341));
#38442=CARTESIAN_POINT('',(-0.0155046880682326,0.0109917502076387,0.0348160726583768));
#38443=CARTESIAN_POINT('',(-0.0156402140687233,0.0110885504931114,0.0348443559162426));
#38444=CARTESIAN_POINT('',(-0.0152364648233893,0.0113604855289649,0.0346356001016534));
#38445=CARTESIAN_POINT('',(-0.0152339091320912,0.0113639109933041,0.0348045006911381));
#38446=CARTESIAN_POINT('',(-0.0153670984922735,0.011464041519689,0.0348327262025861));
#38447=CARTESIAN_POINT('',(-0.0143873413094915,0.0124437284250746,0.0346008656037464));
#38448=CARTESIAN_POINT('',(-0.0143844751282124,0.0124470545266044,0.0347698845094911));
#38449=CARTESIAN_POINT('',(-0.0145103762353732,0.0125566260963977,0.0347980160624915));
#38450=CARTESIAN_POINT('',(-0.0137721352635693,0.0131213741649385,0.0345780643470608));
#38451=CARTESIAN_POINT('',(-0.0137694818893377,0.0131241809415071,0.0347469744606031));
#38452=CARTESIAN_POINT('',(-0.0138895112515776,0.0132399470206423,0.0347751919476471));
#38453=CARTESIAN_POINT('',(-0.0127756253635579,0.0140710319093379,0.0345437131909995));
#38454=CARTESIAN_POINT('',(-0.0127725972833309,0.0140737786150071,0.0347124090405052));
#38455=CARTESIAN_POINT('',(-0.012883865704725,0.014197492280553,0.0347407999552201));
#38456=CARTESIAN_POINT('',(-0.0124311249251211,0.0143764065730164,0.0345322328101261));
#38457=CARTESIAN_POINT('',(-0.0124280148068597,0.014379097791852,0.0347008592833387));
#38458=CARTESIAN_POINT('',(-0.0125362170837346,0.0145053941696239,0.0347293059401341));
#38459=CARTESIAN_POINT('',(-0.0117168670088797,0.0149642560908607,0.0345091027245447));
#38460=CARTESIAN_POINT('',(-0.0117136215730514,0.0149667956603315,0.0346776315441962));
#38461=CARTESIAN_POINT('',(-0.0118154798778907,0.0150981234397663,0.0347061563112278));
#38462=CARTESIAN_POINT('',(-0.0113471776301141,0.0152464405664509,0.0344974581748037));
#38463=CARTESIAN_POINT('',(-0.0113438235877949,0.015248937087422,0.0346659571752721));
#38464=CARTESIAN_POINT('',(-0.0114424601046325,0.0153826585151736,0.034694505939985));
#38465=CARTESIAN_POINT('',(-0.0102183752170634,0.0160447614000967,0.0344627249289449));
#38466=CARTESIAN_POINT('',(-0.0102148320542317,0.0160470183317958,0.0346312187415583));
#38467=CARTESIAN_POINT('',(-0.0103035592236308,0.0161876779090066,0.0346597711170653));
#38468=CARTESIAN_POINT('',(-0.00943380695794407,0.0165179153350184,0.0344396288436497));
#38469=CARTESIAN_POINT('',(-0.00942988974465749,0.0165201371650897,0.0346082295981398));
#38470=CARTESIAN_POINT('',(-0.00951206580947337,0.0166648848158917,0.0346366973123326));
#38471=CARTESIAN_POINT('',(-0.00780188490406774,0.0173484533223647,0.0343933234065022));
#38472=CARTESIAN_POINT('',(-0.00779777914175426,0.0173503145054647,0.034562171101279));
#38473=CARTESIAN_POINT('',(-0.00786576731965972,0.0175025251763002,0.0345904404061971));
#38474=CARTESIAN_POINT('',(-0.00695372238075959,0.0177061261627772,0.0343701512269808));
#38475=CARTESIAN_POINT('',(-0.00695002520057826,0.0177075890954631,0.034539100426332));
#38476=CARTESIAN_POINT('',(-0.0070101380881009,0.0178631977841725,0.0345672863120182));
#38477=CARTESIAN_POINT('',(-0.00519515796776929,0.018299494318991,0.0343237363307037));
#38478=CARTESIAN_POINT('',(-0.00519136109862996,0.0183005601040781,0.0344924904081236));
#38479=CARTESIAN_POINT('',(-0.00523596905492631,0.0184610903605914,0.034520833944751));
#38480=CARTESIAN_POINT('',(-0.00430497969731492,0.0185284965405738,0.0343009075934802));
#38481=CARTESIAN_POINT('',(-0.00430107815167976,0.0185294115816766,0.0344694813381066));
#38482=CARTESIAN_POINT('',(-0.00433788529026169,0.0186916714610529,0.0344979698502093));
#38483=CARTESIAN_POINT('',(-0.00250372476356489,0.0188565478430348,0.0342550702880657));
#38484=CARTESIAN_POINT('',(-0.00249972990529646,0.0188570709966858,0.034423500382658));
#38485=CARTESIAN_POINT('',(-0.00252074042207348,0.0190219709299539,0.0344521034780259));
#38486=CARTESIAN_POINT('',(-0.00159264608432865,0.0189555845333338,0.0342320626380529));
#38487=CARTESIAN_POINT('',(-0.0015881755748559,0.0189559473119425,0.0344005162798639));
#38488=CARTESIAN_POINT('',(-0.00160166636770651,0.0191216793941357,0.0344291022586503));
#38489=CARTESIAN_POINT('',(-0.000210002491991403,0.0190044356819909,0.034197081799291));
#38490=CARTESIAN_POINT('',(-0.000205708220503096,0.0190044849460703,0.0343657219829218));
#38491=CARTESIAN_POINT('',(-0.000206904170197636,0.0191708090168374,0.0343941568771733));
#38492=CARTESIAN_POINT('',(0.000255435682216471,0.0190039032550806,0.0341852994832117));
#38493=CARTESIAN_POINT('',(0.000259749403271307,0.0190038432168092,0.0343540184504881));
#38494=CARTESIAN_POINT('',(0.00026261141636447,0.0191702421981893,0.0343823900786291));
#38495=CARTESIAN_POINT('',(0.00117908482266063,0.0189690101296083,0.0341618973737084));
#38496=CARTESIAN_POINT('',(0.00118339102487519,0.0189687444916224,0.0343307637358417));
#38497=CARTESIAN_POINT('',(0.00119434650285929,0.019134972944291,0.0343590169212069));
#38498=CARTESIAN_POINT('',(0.0016379001804294,0.0189348266131091,0.034150262492255));
#38499=CARTESIAN_POINT('',(0.00164214190181302,0.0189344586555448,0.0343191982485964));
#38500=CARTESIAN_POINT('',(0.00165717600464392,0.0191004487829492,0.0343473954438282));
#38501=CARTESIAN_POINT('',(0.00300552223200003,0.01878319300841,0.0341155853588129));
#38502=CARTESIAN_POINT('',(0.00300979096658495,0.018782514997603,0.0342846031666856));
#38503=CARTESIAN_POINT('',(0.00303672412957713,0.0189472313784724,0.0343127355979453));
#38504=CARTESIAN_POINT('',(0.00390554832426864,0.0186169105380753,0.0340927041117735));
#38505=CARTESIAN_POINT('',(0.0039096582421905,0.0186160486743014,0.0342616778831394));
#38506=CARTESIAN_POINT('',(0.00394460615251096,0.0187792043180145,0.0342898449453726));
#38507=CARTESIAN_POINT('',(0.00568208757458414,0.0181536923652092,0.0340465762972639));
#38508=CARTESIAN_POINT('',(0.00568610013138219,0.0181524363616078,0.0342155462581155));
#38509=CARTESIAN_POINT('',(0.00573661376778426,0.0183114590571226,0.0342437162610204));
#38510=CARTESIAN_POINT('',(0.00656322007882397,0.0178543406867263,0.0340232170608366));
#38511=CARTESIAN_POINT('',(0.00656718587587333,0.017852881965957,0.0341922163861871));
#38512=CARTESIAN_POINT('',(0.00662541375372108,0.0180092844977502,0.0342203627200268));
#38513=CARTESIAN_POINT('',(0.00741375790559362,0.0174938901824966,0.0340000000000022));
#38514=CARTESIAN_POINT('',(0.00741762796059613,0.0174922500869792,0.0341689995579578));
#38515=CARTESIAN_POINT('',(0.00748331487893838,0.0176454543212183,0.0341971457690361));
#38516=CARTESIAN_POINT('',(0.00749179746249453,0.0176780363949439,0.0340000000000022));
#38517=CARTESIAN_POINT('',(0.00748331487893831,0.0176454543212184,0.0341971457690361));
#38518=CARTESIAN_POINT('',(0.00741375790559352,0.0174938901824966,0.034));
#38519=CARTESIAN_POINT('',(-0.019,0.,0.0349419586621878));
#38520=CARTESIAN_POINT('',(-0.019,0.00312176764345404,0.0348634621070055));
#38521=CARTESIAN_POINT('',(-0.0174298121913408,0.00936163759178525,0.0347064689966408));
#38522=CARTESIAN_POINT('',(-0.0109250154031967,0.0164955140888929,0.0344709793310939));
#38523=CARTESIAN_POINT('',(-0.00181847642276099,0.0197010597411713,0.034235489665547));
#38524=CARTESIAN_POINT('',(0.00453944946718008,0.0187119970007115,0.0340784965551823));
#38525=CARTESIAN_POINT('',(0.00741375790559356,0.0174938901824965,0.034));
#38526=CARTESIAN_POINT('',(-0.019,-3.2076351825911E-17,0.0349419586621878));
#38527=CARTESIAN_POINT('',(0.019,-3.9861646017376E-17,0.0364417130293248));
#38528=CARTESIAN_POINT('',(0.019,-0.00248709418409196,0.0363792232640274));
#38529=CARTESIAN_POINT('',(0.0180107055600589,-0.00746012312352682,0.0362542437334327));
#38530=CARTESIAN_POINT('',(0.0137847972460806,-0.0137848390811387,0.0360667744375406));
#38531=CARTESIAN_POINT('',(0.00746027851088484,-0.0180106936071852,0.0358793051416484));
#38532=CARTESIAN_POINT('',(-6.51922979228107E-17,-0.0194946531964074,0.0356918358457563));
#38533=CARTESIAN_POINT('',(-0.00746027851088496,-0.0180106936071851,0.0355043665498642));
#38534=CARTESIAN_POINT('',(-0.0137847972460807,-0.0137848390811386,0.035316897253972));
#38535=CARTESIAN_POINT('',(-0.0180107055600589,-0.00746012312352672,0.0351294279580799));
#38536=CARTESIAN_POINT('',(-0.019,-0.00248709418409184,0.0350044484274852));
#38537=CARTESIAN_POINT('',(-0.019,7.9723292034752E-17,0.0349419586621878));
#38538=CARTESIAN_POINT('',(0.019,-3.3932914654129E-18,0.0364417130293248));
#38539=CARTESIAN_POINT('',(-0.019,0.,0.0379414621394879));
#38540=CARTESIAN_POINT('',(-0.019,0.00248709418409192,0.0378789725932311));
#38541=CARTESIAN_POINT('',(-0.0180107055600589,0.00746012312352679,0.0377539935007175));
#38542=CARTESIAN_POINT('',(-0.0137847972460807,0.0137848390811386,0.0375665248619471));
#38543=CARTESIAN_POINT('',(-0.00746027851088488,0.0180106936071852,0.0373790562231767));
#38544=CARTESIAN_POINT('',(2.09173148415435E-17,0.0194946531964074,0.0371915875844063));
#38545=CARTESIAN_POINT('',(0.00746027851088491,0.0180106936071852,0.037004118945636));
#38546=CARTESIAN_POINT('',(0.0137847972460807,0.0137848390811386,0.0368166503068656));
#38547=CARTESIAN_POINT('',(0.0180107055600589,0.00746012312352675,0.0366291816680952));
#38548=CARTESIAN_POINT('',(0.019,0.00248709418409188,0.0365042025755816));
#38549=CARTESIAN_POINT('',(0.019,-3.9861646017376E-17,0.0364417130293248));
#38550=CARTESIAN_POINT('',(-0.019,2.6601721082709E-17,0.0379414621394879));
#38551=CARTESIAN_POINT('',(0.019,6.13906938284383E-17,0.0394419409570244));
#38552=CARTESIAN_POINT('',(0.019,-0.00248709418409186,0.0393794210062937));
#38553=CARTESIAN_POINT('',(0.0180107055600589,-0.00746012312352674,0.0392543811048323));
#38554=CARTESIAN_POINT('',(0.0137847972460807,-0.0137848390811386,0.0390668212526403));
#38555=CARTESIAN_POINT('',(0.00746027851088491,-0.0180106936071852,0.0388792614004482));
#38556=CARTESIAN_POINT('',(-2.12659367555693E-17,-0.0194946531964074,0.0386917015482561));
#38557=CARTESIAN_POINT('',(-0.00746027851088491,-0.0180106936071852,0.0385041416960641));
#38558=CARTESIAN_POINT('',(-0.0137847972460807,-0.0137848390811386,0.038316581843872));
#38559=CARTESIAN_POINT('',(-0.0180107055600589,-0.00746012312352674,0.03812902199168));
#38560=CARTESIAN_POINT('',(-0.019,-0.00248709418409185,0.0380039820902186));
#38561=CARTESIAN_POINT('',(-0.019,7.9723292034752E-17,0.0379414621394879));
#38562=CARTESIAN_POINT('',(0.019,5.51687858964173E-17,0.0394419409570244));
#38563=CARTESIAN_POINT('',(-0.019,0.,0.0409417911129512));
#38564=CARTESIAN_POINT('',(-0.019,0.00248709418409192,0.0408792973564542));
#38565=CARTESIAN_POINT('',(-0.0180107055600589,0.00746012312352678,0.0407543098434603));
#38566=CARTESIAN_POINT('',(-0.0137847972460807,0.0137848390811386,0.0405668285739695));
#38567=CARTESIAN_POINT('',(-0.00746027851088491,0.0180106936071852,0.0403793473044786));
#38568=CARTESIAN_POINT('',(-3.20732160903668E-17,0.0194946531964074,0.0401918660349878));
#38569=CARTESIAN_POINT('',(0.00746027851088485,0.0180106936071852,0.0400043847654969));
#38570=CARTESIAN_POINT('',(0.0137847972460806,0.0137848390811386,0.0398169034960061));
#38571=CARTESIAN_POINT('',(0.0180107055600588,0.00746012312352683,0.0396294222265152));
#38572=CARTESIAN_POINT('',(0.019,0.00248709418409198,0.0395044347135213));
#38573=CARTESIAN_POINT('',(0.019,6.13906938284383E-17,0.0394419409570244));
#38574=CARTESIAN_POINT('',(-0.019,4.74885777153119E-15,0.0409417911129512));
#38575=CARTESIAN_POINT('',(0.019,1.90546421099058E-14,0.0424415956712427));
#38576=CARTESIAN_POINT('',(0.0190000000000025,-0.00248709418407366,0.0423791038146472));
#38577=CARTESIAN_POINT('',(0.0180107055600657,-0.00746012312351111,0.0422541201014563));
#38578=CARTESIAN_POINT('',(0.0137847972460913,-0.0137848390811285,0.0420666445316698));
#38579=CARTESIAN_POINT('',(0.00746027851089627,-0.0180106936071808,0.0418791689618834));
#38580=CARTESIAN_POINT('',(9.73352383959826E-15,-0.0194946531964077,0.0416916933920969));
#38581=CARTESIAN_POINT('',(-0.00746027851087828,-0.0180106936071883,0.0415042178223105));
#38582=CARTESIAN_POINT('',(-0.0137847972460775,-0.0137848390811422,0.0413167422525241));
#38583=CARTESIAN_POINT('',(-0.0180107055600582,-0.00746012312352912,0.0411292666827376));
#38584=CARTESIAN_POINT('',(-0.019,-0.00248709418409264,0.0410042829695467));
#38585=CARTESIAN_POINT('',(-0.019,7.9723292034752E-17,0.0409417911129512));
#38586=CARTESIAN_POINT('',(0.019,1.90573078608331E-14,0.0424415956712427));
#38587=CARTESIAN_POINT('',(0.0132733600509949,0.0135947752080221,0.0428219504950535));
#38588=CARTESIAN_POINT('',(0.0150800156837313,0.0118308335220045,0.0427585580244184));
#38589=CARTESIAN_POINT('',(0.0179798105748163,0.00757378477671875,0.0426317730831481));
#38590=CARTESIAN_POINT('',(0.0189999999999975,0.00252497422701,0.0425049881418778));
#38591=CARTESIAN_POINT('',(0.019,1.90546421099058E-14,0.0424415956712427));
#38592=CARTESIAN_POINT('',(0.0135335405895343,0.0135722295367336,0.0430141822613637));
#38593=CARTESIAN_POINT('',(0.0135341500471712,0.0135716215917096,0.0430141616768234));
#38594=CARTESIAN_POINT('',(0.0135347594691913,0.0135710136063163,0.0430141410888615));
#38595=CARTESIAN_POINT('',(0.0135353688555734,0.0135704055805392,0.0430141204974931));
#38596=CARTESIAN_POINT('',(0.0135353510208537,0.0135703818080405,0.0430142946508867));
#38597=CARTESIAN_POINT('',(0.0135353688555734,0.0135704055805392,0.0430141204974931));
#38598=CARTESIAN_POINT('',(0.0161498178403471,0.0109578623504477,0.0429252407150377));
#38599=CARTESIAN_POINT('',(0.018896002464485,0.00590598767738096,0.0427847623969909));
#38600=CARTESIAN_POINT('',(0.0193098145538766,-0.000625315742798855,0.0426233441156423));
#38601=CARTESIAN_POINT('',(0.018756637468961,-0.00425420435492626,0.0425326941106314));
#38602=CARTESIAN_POINT('',(0.017939462958948,-0.00693277608908051,0.0424630453307758));
#38603=CARTESIAN_POINT('',(0.0167719383093269,-0.00941371737899657,0.0423943015591571));
#38604=CARTESIAN_POINT('',(0.0152275971629559,-0.011749218418051,0.0423251314671479));
#38605=CARTESIAN_POINT('',(0.0133927598958916,-0.0138018238182261,0.0422570767083249));
#38606=CARTESIAN_POINT('',(0.0112669003617152,-0.015588270498333,0.0421876505427081));
#38607=CARTESIAN_POINT('',(0.00890096294820859,-0.0170486177791914,0.0421184486185939));
#38608=CARTESIAN_POINT('',(0.0063781955005646,-0.0181446735945083,0.042050625438433));
#38609=CARTESIAN_POINT('',(0.00367453763971176,-0.018878268632462,0.041980836710611));
#38610=CARTESIAN_POINT('',(0.00095276270518741,-0.0192096809442985,0.0419121587103747));
#38611=CARTESIAN_POINT('',(-0.00184583529240445,-0.0191442027451065,0.04184309187272));
#38612=CARTESIAN_POINT('',(-0.00546575961568702,-0.0185311108673583,0.0417521611352773));
#38613=CARTESIAN_POINT('',(-0.00894299434047007,-0.0171264964984881,0.0416589517043263));
#38614=CARTESIAN_POINT('',(-0.011969492833948,-0.0150542322956112,0.0415685362868275));
#38615=CARTESIAN_POINT('',(-0.0140294246337335,-0.0131558205092909,0.0414986313581724));
#38616=CARTESIAN_POINT('',(-0.0157584853266227,-0.0110265159034489,0.0414300096906797));
#38617=CARTESIAN_POINT('',(-0.0176676247681137,-0.00782515303996317,0.041338199097655));
#38618=CARTESIAN_POINT('',(-0.0188342416993615,-0.00431655998882969,0.0412464695364074));
#38619=CARTESIAN_POINT('',(-0.0192225789677563,-0.000621704652356598,0.0411542685630935));
#38620=CARTESIAN_POINT('',(-0.0191151445766951,0.00212441003994294,0.0410864281170052));
#38621=CARTESIAN_POINT('',(-0.0186037925464179,0.00487875125399747,0.0410164256524546));
#38622=CARTESIAN_POINT('',(-0.0177208152379379,0.00747598493059139,0.0409479265235543));
#38623=CARTESIAN_POINT('',(-0.016448360009597,0.00996756637677533,0.0408790004502757));
#38624=CARTESIAN_POINT('',(-0.014324722750542,0.012965147511815,0.0407877055934287));
#38625=CARTESIAN_POINT('',(-0.011550414631196,0.015487795214077,0.0406948338092932));
#38626=CARTESIAN_POINT('',(-0.00837128058162158,0.0173152952700514,0.0406043068008098));
#38627=CARTESIAN_POINT('',(-0.0057673062400589,0.0183480298387254,0.040534205167538));
#38628=CARTESIAN_POINT('',(-0.00309772308846666,0.0189819792717225,0.0404658161268834));
#38629=CARTESIAN_POINT('',(0.000613590956548792,0.0193129287051469,0.0403740753133858));
#38630=CARTESIAN_POINT('',(0.00427983448328106,0.0188431233165396,0.0402820726208667));
#38631=CARTESIAN_POINT('',(0.00778010889064711,0.0175885872608356,0.0401901465007869));
#38632=CARTESIAN_POINT('',(0.0102063567334771,0.0163012867396412,0.0401221673372315));
#38633=CARTESIAN_POINT('',(0.0124675930149152,0.0146450218783127,0.0400519767699712));
#38634=CARTESIAN_POINT('',(0.0144237842802552,0.0127225832477427,0.0399837570344856));
#38635=CARTESIAN_POINT('',(0.0161159401675219,0.0104963981981657,0.0399148699216431));
#38636=CARTESIAN_POINT('',(0.0178968799936531,0.00728075889012127,0.0398232181034071));
#38637=CARTESIAN_POINT('',(0.0189651862938166,0.00368753414307424,0.0397307671157354));
#38638=CARTESIAN_POINT('',(0.0192327028976888,3.00353480110928E-5,0.0396399980054814));
#38639=CARTESIAN_POINT('',(0.0190337323354013,-0.00276394975683582,0.0395697780757167));
#38640=CARTESIAN_POINT('',(0.018446230547656,-0.00544438105205532,0.0395016869387841));
#38641=CARTESIAN_POINT('',(0.0171349139652453,-0.00893052771404328,0.0394098557370111));
#38642=CARTESIAN_POINT('',(0.0151220674546025,-0.0120297481353181,0.0393177805662593));
#38643=CARTESIAN_POINT('',(0.0124711767467395,-0.0146408504437676,0.0392260048260426));
#38644=CARTESIAN_POINT('',(0.0102598867147642,-0.0162675495412288,0.0391578555996006));
#38645=CARTESIAN_POINT('',(0.00778642693052377,-0.0175869696511293,0.0390875873063964));
#38646=CARTESIAN_POINT('',(0.00520447288027298,-0.0185150591603213,0.039019639281149));
#38647=CARTESIAN_POINT('',(0.00246754413694701,-0.0190742684960932,0.0389506880769338));
#38648=CARTESIAN_POINT('',(-0.000290406066513938,-0.0192298276349607,0.0388817156801483));
#38649=CARTESIAN_POINT('',(-0.00304518049289391,-0.0189913664368629,0.0388127338115798));
#38650=CARTESIAN_POINT('',(-0.00576121780142906,-0.0183489981346029,0.0387439292815532));
#38651=CARTESIAN_POINT('',(-0.00831583448795037,-0.0173420717943234,0.0386756497980644));
#38652=CARTESIAN_POINT('',(-0.0115547279583845,-0.0154885311234985,0.0385821304483689));
#38653=CARTESIAN_POINT('',(-0.0142851239316347,-0.0130133529355991,0.0384923772384108));
#38654=CARTESIAN_POINT('',(-0.0164584685016815,-0.00995259962459248,0.0383985070890661));
#38655=CARTESIAN_POINT('',(-0.0181280991357095,-0.00668324788376798,0.0383072159644954));
#38656=CARTESIAN_POINT('',(-0.0190770573354136,-0.00305385807602741,0.0382152822618342));
#38657=CARTESIAN_POINT('',(-0.0192239215401177,0.00060811378866868,0.0381233883639684));
#38658=CARTESIAN_POINT('',(-0.0189310231518623,0.00339509759960875,0.0380542489857858));
#38659=CARTESIAN_POINT('',(-0.0182542598980589,0.00605476811571894,0.0379863474074727));
#38660=CARTESIAN_POINT('',(-0.0168302625510012,0.00949424787791312,0.0378931324005353));
#38661=CARTESIAN_POINT('',(-0.0147127376841849,0.0125251302411581,0.0378027441799212));
#38662=CARTESIAN_POINT('',(-0.0119775777837324,0.0150476157199599,0.0377099881368222));
#38663=CARTESIAN_POINT('',(-0.00971403790835766,0.0166002034105028,0.0376412938168035));
#38664=CARTESIAN_POINT('',(-0.00719759777520637,0.0178354879993317,0.0375721916540058));
#38665=CARTESIAN_POINT('',(-0.0045852920319042,0.0186774722401391,0.0375041777335244));
#38666=CARTESIAN_POINT('',(-0.00183392773622591,0.0191462390263392,0.0374342939225838));
#38667=CARTESIAN_POINT('',(0.000930292961064554,0.0192097121327847,0.0373657490387983));
#38668=CARTESIAN_POINT('',(0.00367415075193295,0.0188787530141101,0.0372974987999961));
#38669=CARTESIAN_POINT('',(0.00636867754597101,0.0181475082599207,0.0372277545078323));
#38670=CARTESIAN_POINT('',(0.00888701139462942,0.0170572583903196,0.0371591969319872));
#38671=CARTESIAN_POINT('',(0.0112717973743793,0.0155837321927682,0.0370901295748675));
#38672=CARTESIAN_POINT('',(0.0133751805831766,0.0138197199427338,0.0370220059714728));
#38673=CARTESIAN_POINT('',(0.0158546750963597,0.0110463770905087,0.0369288203331229));
#38674=CARTESIAN_POINT('',(0.0176676936866646,0.00782393198606787,0.0368386594887747));
#38675=CARTESIAN_POINT('',(0.0187543862598064,0.00426286323505308,0.0367455323277807));
#38676=CARTESIAN_POINT('',(0.0191708150624781,0.00155072179234026,0.0366771182045157));
#38677=CARTESIAN_POINT('',(0.0191921575802405,-0.00125232563135686,0.0366080604046766));
#38678=CARTESIAN_POINT('',(0.0188173194808651,-0.00397257306730293,0.0365398125587642));
#38679=CARTESIAN_POINT('',(0.0180470622439191,-0.00665228714291196,0.0364699901440749));
#38680=CARTESIAN_POINT('',(0.0169033075242486,-0.00917314068262214,0.0364016127764803));
#38681=CARTESIAN_POINT('',(0.0154167509158799,-0.0114995951877568,0.0363332673933967));
#38682=CARTESIAN_POINT('',(0.0135873852996124,-0.0136118387317986,0.0362633074197483));
#38683=CARTESIAN_POINT('',(0.0115130064335834,-0.0154069235218565,0.0361950572005525));
#38684=CARTESIAN_POINT('',(0.00915099589266125,-0.0169163410861854,0.0361259786168976));
#38685=CARTESIAN_POINT('',(0.00664816293250691,-0.0180467741812788,0.0360576130065278));
#38686=CARTESIAN_POINT('',(0.00307582408105403,-0.0190768596647923,0.0359646146664873));
#38687=CARTESIAN_POINT('',(-0.000614380751948974,-0.0193129186119715,0.0358744750087052));
#38688=CARTESIAN_POINT('',(-0.0042960343038314,-0.018747026369487,0.0357810926952821));
#38689=CARTESIAN_POINT('',(-0.00691981570441502,-0.0179453056330825,0.0357129970754028));
#38690=CARTESIAN_POINT('',(-0.00945357573199342,-0.0167490017306704,0.0356439203566654));
#38691=CARTESIAN_POINT('',(-0.0125098522922861,-0.0147235243482249,0.0355523919411737));
#38692=CARTESIAN_POINT('',(-0.0151185474142208,-0.0120303297988389,0.0354600967454023));
#38693=CARTESIAN_POINT('',(-0.0170481137245165,-0.00890303733159082,0.0353690195303689));
#38694=CARTESIAN_POINT('',(-0.0181594653228968,-0.0063361992120837,0.0352988708491257));
#38695=CARTESIAN_POINT('',(-0.018875971452887,-0.00368907908914855,0.0352309647005051));
#38696=CARTESIAN_POINT('',(-0.019211490669188,-0.000906538208031904,0.0351617804587047));
#38697=CARTESIAN_POINT('',(-0.0191443011592234,0.00184013369332341,0.035093185607839));
#38698=CARTESIAN_POINT('',(-0.018522526050253,0.00550381644714024,0.0350005226370239));
#38699=CARTESIAN_POINT('',(-0.0171351337536918,0.00893101889174432,0.0349102021080862));
#38700=CARTESIAN_POINT('',(-0.0150269900835202,0.0120043229327353,0.0348166884810567));
#38701=CARTESIAN_POINT('',(-0.0131662745690762,0.0140198448206814,0.0347489116431167));
#38702=CARTESIAN_POINT('',(-0.0109900340176108,0.0157836795334412,0.0346796934145625));
#38703=CARTESIAN_POINT('',(-0.00783682721710034,0.0176592587274472,0.0345878893869752));
#38704=CARTESIAN_POINT('',(-0.00162495554055579,0.0197288917722028,0.0344274670366339));
#38705=CARTESIAN_POINT('',(0.00407409956719794,0.0190912786150354,0.0342894074497274));
#38706=CARTESIAN_POINT('',(0.00748331487893838,0.0176454543212183,0.0341971457690361));
#38707=CARTESIAN_POINT('',(0.0135247164963182,0.0135491354261317,0.0340048173228733));
#38708=CARTESIAN_POINT('',(0.0134522998980134,0.0134185657624297,0.0340037511130871));
#38709=CARTESIAN_POINT('',(0.0135568792897986,0.013312063097876,0.034));
#38710=CARTESIAN_POINT('',(0.0135234994968269,0.0135502855516948,0.0339374949028807));
#38711=CARTESIAN_POINT('',(0.0134507948637152,0.0134196591751994,0.0339250904797292));
#38712=CARTESIAN_POINT('',(0.0135557820741085,0.0133131804919685,0.033921285990061));
#38713=CARTESIAN_POINT('',(0.0135278548856968,0.0135569617878143,0.0338714576447267));
#38714=CARTESIAN_POINT('',(0.0134558017982309,0.0134272067953835,0.0338479166793451));
#38715=CARTESIAN_POINT('',(0.0135612061032408,0.0133207522704363,0.0338440728084942));
#38716=CARTESIAN_POINT('',(0.0135375715470061,0.013568951169631,0.0338067616450345));
#38717=CARTESIAN_POINT('',(0.0134670675691026,0.01344095421085,0.0337722952163498));
#38718=CARTESIAN_POINT('',(0.0135729078908396,0.0133345360558799,0.0337684261530207));
#38719=CARTESIAN_POINT('',(0.0135726991431301,0.0133342900396015,0.0337697801684402));
#38720=CARTESIAN_POINT('',(0.0135610979456742,0.0133206611476437,0.0338451346978836));
#38721=CARTESIAN_POINT('',(0.0135557655877528,0.0133131972815174,0.0339225654745483));
#38722=CARTESIAN_POINT('',(0.0135568792897986,0.013312063097876,0.034));
#38723=CARTESIAN_POINT('',(0.0135726991431301,0.0133342900396015,0.0337697801684401));
#38724=CARTESIAN_POINT('',(0.0135726991346738,0.0133342900312937,0.0337697801656355));
#38725=CARTESIAN_POINT('',(0.0135608689083288,0.0133411879010404,0.0337850169067288));
#38726=CARTESIAN_POINT('',(0.0135261534936828,0.0133696145659868,0.0338380484731189));
#38727=CARTESIAN_POINT('',(0.013493225546999,0.0134285620019686,0.0339197948589413));
#38728=CARTESIAN_POINT('',(0.0135054310078758,0.0135145300695567,0.0339890626438917));
#38729=CARTESIAN_POINT('',(0.0135239956136941,0.0135478241103007,0.0340048065022042));
#38730=CARTESIAN_POINT('',(0.00741375790559351,0.0174938901824966,0.0340000000000028));
#38731=CARTESIAN_POINT('',(0.0074176279605962,0.0174922500869796,0.0341689995579579));
#38732=CARTESIAN_POINT('',(0.00748331487893827,0.0176454543212184,0.0341971457690361));
#38733=CARTESIAN_POINT('',(0.00799464401290268,0.0172477157224201,0.0339801794998395));
#38734=CARTESIAN_POINT('',(0.00800212560069349,0.0172407233498891,0.0341524362276056));
#38735=CARTESIAN_POINT('',(0.00806923059913374,0.0173969713509321,0.0341812894236565));
#38736=CARTESIAN_POINT('',(0.00856561383670638,0.0169720369215461,0.0339604377545791));
#38737=CARTESIAN_POINT('',(0.00857099591731754,0.0169613822002568,0.0341359610403092));
#38738=CARTESIAN_POINT('',(0.0086450247826401,0.0171185073952909,0.0341654757873373));
#38739=CARTESIAN_POINT('',(0.00967269163952337,0.0163690746593947,0.0339214044506673));
#38740=CARTESIAN_POINT('',(0.00967397428338661,0.0163519147228243,0.0341031417042596));
#38741=CARTESIAN_POINT('',(0.00976117260934767,0.0165091869101672,0.0341341741865354));
#38742=CARTESIAN_POINT('',(0.0102074312117974,0.0160428532240274,0.0339021292666557));
#38743=CARTESIAN_POINT('',(0.0102059284872208,0.016022110139271,0.034086845502193));
#38744=CARTESIAN_POINT('',(0.0103001539749249,0.0161794310522496,0.0341187042517711));
#38745=CARTESIAN_POINT('',(0.0112404839068122,0.0153423684648806,0.0338637517753579));
#38746=CARTESIAN_POINT('',(0.0112332853866827,0.0153154078586966,0.0340542850074699));
#38747=CARTESIAN_POINT('',(0.011341079607521,0.0154713323131514,0.0340878936508673));
#38748=CARTESIAN_POINT('',(0.0117387955300322,0.0149681033735197,0.0338446492933245));
#38749=CARTESIAN_POINT('',(0.0117280389869818,0.0149376995987162,0.034038022302507));
#38750=CARTESIAN_POINT('',(0.0118430241296028,0.0150929851913844,0.0340725528860564));
#38751=CARTESIAN_POINT('',(0.0126990967570012,0.014171558726067,0.033806541009908));
#38752=CARTESIAN_POINT('',(0.0126809315014158,0.0141354605322774,0.0340053832026719));
#38753=CARTESIAN_POINT('',(0.012809866962313,0.0142877563781691,0.0340419258464437));
#38754=CARTESIAN_POINT('',(0.0131608718072554,0.0137489868194859,0.0337890310203656));
#38755=CARTESIAN_POINT('',(0.0131389206922079,0.0137100385174954,0.0339891335836076));
#38756=CARTESIAN_POINT('',(0.0132735769552999,0.0138601685116395,0.0340276462825612));
#38757=CARTESIAN_POINT('',(0.0136044777921139,0.0133023653697072,0.0337683091703764));
#38758=CARTESIAN_POINT('',(0.0135736223072447,0.0132643239162051,0.0339726046099247));
#38759=CARTESIAN_POINT('',(0.0137210863278384,0.0134089001480767,0.0340111781184431));
#38760=CARTESIAN_POINT('',(0.00741375790559351,0.0174938901824966,0.034));
#38761=CARTESIAN_POINT('',(0.00970786016513252,0.0165216696766245,0.0339225654745483));
#38762=CARTESIAN_POINT('',(0.0118113590310252,0.0151016843440063,0.0338451346978836));
#38763=CARTESIAN_POINT('',(0.0135726991431301,0.0133342900396015,0.0337697801684402));
#38764=CARTESIAN_POINT('',(0.00748331487893827,0.0176454543212184,0.0341971457690361));
#38765=CARTESIAN_POINT('',(0.00861748461183809,0.0171644604609653,0.034166452298313));
#38766=CARTESIAN_POINT('',(0.0107946770544553,0.0159827433342134,0.0341051551118467));
#38767=CARTESIAN_POINT('',(0.0126732556571759,0.0144434668614907,0.0340483193425882));
#38768=CARTESIAN_POINT('',(0.0135476845953551,0.013581764079206,0.0340174277337795));
#38769=CARTESIAN_POINT('',(0.0134350288425444,0.0134350288425444,0.044));
#38770=CARTESIAN_POINT('',(0.0134350288425444,0.0134350288425444,0.044));
#38771=CARTESIAN_POINT('',(0.0134350288425449,0.0134350288425438,0.035));
#38772=CARTESIAN_POINT('',(0.0134350288425449,0.0134350288425438,0.035));
#38773=CARTESIAN_POINT('',(-0.04,0.,-0.04));
#38774=CARTESIAN_POINT('',(0.,0.,-0.04));
#38775=CARTESIAN_POINT('',(-0.04,0.,-0.04));
#38776=CARTESIAN_POINT('',(0.,0.,0.046));
#38777=CARTESIAN_POINT('',(0.,0.,0.046));
#38778=CARTESIAN_POINT('',(0.0188,0.,0.046));
#38779=CARTESIAN_POINT('',(0.,0.,0.046));
#38780=CARTESIAN_POINT('',(0.0123,0.,0.046));
#38781=CARTESIAN_POINT('',(1.08184846837294E-17,0.,0.03));
#38782=CARTESIAN_POINT('',(-0.0175,0.0303108891324553,0.03));
#38783=CARTESIAN_POINT('',(-0.0183131446174913,0.0432854332797865,0.03));
#38784=CARTESIAN_POINT('',(-0.0283297125253659,0.0375023651018189,0.03));
#38785=CARTESIAN_POINT('',(0.,0.,0.03));
#38786=CARTESIAN_POINT('',(0.,0.,0.03));
#38787=CARTESIAN_POINT('',(-0.019,0.,0.03));
#38788=CARTESIAN_POINT('',(1.0775734895605E-17,0.,0.033));
#38789=CARTESIAN_POINT('',(0.,0.,0.033));
#38790=CARTESIAN_POINT('',(-0.0259053349880927,0.0357284848849959,0.033));
#38791=CARTESIAN_POINT('',(-0.0179891080550886,0.0402989206357321,0.033));
#38792=CARTESIAN_POINT('',(-0.0175,0.0303108891324553,0.033));
#38793=CARTESIAN_POINT('',(0.,0.,0.033));
#38794=CARTESIAN_POINT('',(0.02,0.,0.033));
#38795=CARTESIAN_POINT('',(0.,0.,0.0396457076047696));
#38796=CARTESIAN_POINT('',(0.,0.,0.0396457076047696));
#38797=CARTESIAN_POINT('',(0.05,0.,0.0396457076047696));
#38798=CARTESIAN_POINT('',(-0.0179891080550886,0.0402989206357321,0.033));
#38799=CARTESIAN_POINT('',(-0.0187458295220114,0.0402618644285296,0.03331100188783));
#38800=CARTESIAN_POINT('',(-0.0202815477394373,0.0400153314880262,0.0338032106110653));
#38801=CARTESIAN_POINT('',(-0.0225425615656762,0.0390633626363814,0.0340721518705467));
#38802=CARTESIAN_POINT('',(-0.0245020780652921,0.0375846816769992,0.0338078665554804));
#38803=CARTESIAN_POINT('',(-0.0254946132923719,0.0363657146815882,0.0333112059722862));
#38804=CARTESIAN_POINT('',(-0.0259053349880927,0.0357284848849959,0.033));
#38805=CARTESIAN_POINT('',(-0.0175,0.0303108891324553,0.107));
#38806=CARTESIAN_POINT('',(0.,0.,0.046));
#38807=CARTESIAN_POINT('',(0.,0.,0.034));
#38808=CARTESIAN_POINT('',(0.,0.,0.0458));
#38809=CARTESIAN_POINT('',(0.019,0.,0.0458));
#38810=CARTESIAN_POINT('',(0.,0.,0.));
#38811=CARTESIAN_POINT('',(0.,0.,0.0442));
#38812=CARTESIAN_POINT('',(-0.0121,0.,0.0442));
#38813=CARTESIAN_POINT('',(0.,0.,0.0458));
#38814=CARTESIAN_POINT('',(0.0121,0.,0.0458));
#38815=CARTESIAN_POINT('',(0.,0.,0.046));
#38816=CARTESIAN_POINT('',(0.,0.,0.033));
#38817=CARTESIAN_POINT('',(-0.016,0.,0.033));
#38818=CARTESIAN_POINT('',(0.,0.,0.0400107279868694));
#38819=CARTESIAN_POINT('',(-0.016,0.,0.0400107279868694));
#38820=CARTESIAN_POINT('',(0.,0.,0.));
#38821=CARTESIAN_POINT('',(0.,0.,-0.03));
#38822=CARTESIAN_POINT('',(-0.05,0.,-0.03));
#38823=CARTESIAN_POINT('',(0.,0.,0.027));
#38824=CARTESIAN_POINT('',(-0.05,0.,0.027));
#38825=CARTESIAN_POINT('',(0.,0.,-0.03));
#38826=CARTESIAN_POINT('',(0.0119917500543135,0.0150793149034488,0.0430647002772689));
#38827=CARTESIAN_POINT('',(0.0125011351272437,0.0145712292566673,0.0430467550241789));
#38828=CARTESIAN_POINT('',(0.013010520200174,0.0140631436098858,0.043028809771089));
#38829=CARTESIAN_POINT('',(0.0135199052731042,0.0135550579631043,0.0430108645179991));
#38830=CARTESIAN_POINT('',(0.0150074761996503,0.0120712817856836,0.042958458512828));
#38831=CARTESIAN_POINT('',(0.0162575507862789,0.01032732078082,0.0429056768871633));
#38832=CARTESIAN_POINT('',(0.0185852198899116,0.00558586532020392,0.0427738987465939));
#38833=CARTESIAN_POINT('',(0.0192552744826652,0.00239702668057813,0.0426950802007972));
#38834=CARTESIAN_POINT('',(0.0190021699218141,-0.0039291638470396,0.0425371897621086));
#38835=CARTESIAN_POINT('',(0.0180761838518777,-0.00705722965242059,0.0424582447351112));
#38836=CARTESIAN_POINT('',(0.0148422268308121,-0.0125000201568053,0.0423003225632235));
#38837=CARTESIAN_POINT('',(0.0125382516416315,-0.0148092920302629,0.042221379417481));
#38838=CARTESIAN_POINT('',(0.00710378716781687,-0.0180571812145946,0.0420635018522572));
#38839=CARTESIAN_POINT('',(0.0039786824719132,-0.0189926412444474,0.0419845627080643));
#38840=CARTESIAN_POINT('',(-0.00234668519603218,-0.0192623405937001,0.0418266349581681));
#38841=CARTESIAN_POINT('',(-0.00554006854269375,-0.0185965109372015,0.0417476957409817));
#38842=CARTESIAN_POINT('',(-0.011231462134108,-0.0158233918460566,0.041589817663171));
#38843=CARTESIAN_POINT('',(-0.0137238699102723,-0.0137188110133377,0.0415108784584664));
#38844=CARTESIAN_POINT('',(-0.0174093010078421,-0.00857093437562775,0.0413529508414693));
#38845=CARTESIAN_POINT('',(-0.0185985058296419,-0.00553336791248007,0.0412740115167333));
#38846=CARTESIAN_POINT('',(-0.0193898407789082,0.000748028528479798,0.0411161334534399));
#38847=CARTESIAN_POINT('',(-0.0189911740659409,0.00398568545192271,0.0410371942485536));
#38848=CARTESIAN_POINT('',(-0.0166972840647074,0.00988662641355999,0.0408792666290302));
#38849=CARTESIAN_POINT('',(-0.0148047686356766,0.0125435802427221,0.040800327306438));
#38850=CARTESIAN_POINT('',(-0.00997901329099115,0.0166416575456676,0.0406424492429172));
#38851=CARTESIAN_POINT('',(-0.00705050542285551,0.0180787376270981,0.0405635100380233));
#38852=CARTESIAN_POINT('',(-0.000855796548201768,0.019385878604594,0.0404055824185264));
#38853=CARTESIAN_POINT('',(0.0024036239598539,0.0192547441300795,0.040326643095907));
#38854=CARTESIAN_POINT('',(0.00847383490058702,0.0174562193561262,0.0401687650323922));
#38855=CARTESIAN_POINT('',(0.0112786521558426,0.015790579041134,0.0400898258274887));
#38856=CARTESIAN_POINT('',(0.0157611313736707,0.0113195147787425,0.0399318982080082));
#38857=CARTESIAN_POINT('',(0.0174340840310036,0.0085191134315629,0.039852958885376));
#38858=CARTESIAN_POINT('',(0.0192485100731383,0.00245363650347758,0.0396950808218705));
#38859=CARTESIAN_POINT('',(0.0193881814683697,-0.000805481382629234,0.0396161416169616));
#38860=CARTESIAN_POINT('',(0.0180968400976795,-0.00700350308644694,0.0394582139974826));
#38861=CARTESIAN_POINT('',(0.0166674563386305,-0.00993571732966755,0.0393792746748263));
#38862=CARTESIAN_POINT('',(0.0125820393617557,-0.0147721954235223,0.0392213966113676));
#38863=CARTESIAN_POINT('',(0.009930008131089,-0.0166716921584716,0.0391424574064428));
#38864=CARTESIAN_POINT('',(0.00403493534485767,-0.0189806210057407,0.0389845297869488));
#38865=CARTESIAN_POINT('',(0.000798385059068726,-0.0193877580180761,0.0389055904643503));
#38866=CARTESIAN_POINT('',(-0.00548506356453857,-0.0186128866597783,0.038747712400791));
#38867=CARTESIAN_POINT('',(-0.00852578215354342,-0.0174316212550832,0.0386687731959199));
#38868=CARTESIAN_POINT('',(-0.0136830391876003,-0.01375932831178,0.0385108455764191));
#38869=CARTESIAN_POINT('',(-0.0157941058636261,-0.0112724797461941,0.0384319062538021));
#38870=CARTESIAN_POINT('',(-0.0185821301893177,-0.00558837272865016,0.0382740281902866));
#38871=CARTESIAN_POINT('',(-0.0192563298219162,-0.00239669411864687,0.0381950889853776));
#38872=CARTESIAN_POINT('',(-0.0190027615072474,0.003929342451488,0.0380371613659087));
#38873=CARTESIAN_POINT('',(-0.0180754992816383,0.00705683394845448,0.0379582220432658));
#38874=CARTESIAN_POINT('',(-0.0148418601975698,0.0124997863184206,0.0378003439797702));
#38875=CARTESIAN_POINT('',(-0.0125386461030731,0.0148098863875077,0.0377214047748604));
#38876=CARTESIAN_POINT('',(-0.00710401162363045,0.0180576215447498,0.0375634771553734));
#38877=CARTESIAN_POINT('',(-0.00397861621492044,0.0189919244067349,0.0374845378327532));
#38878=CARTESIAN_POINT('',(0.00234667399305028,0.0192618429362422,0.0373266597692301));
#38879=CARTESIAN_POINT('',(0.00554035103904963,0.0185971742818825,0.0372477205643357));
#38880=CARTESIAN_POINT('',(0.0112317093616142,0.0158238232365207,0.0370897929448454));
#38881=CARTESIAN_POINT('',(0.0137233056605262,0.0137183621985592,0.0370108536222324));
#38882=CARTESIAN_POINT('',(0.0174088782338546,0.00857067271353671,0.0368529755586984));
#38883=CARTESIAN_POINT('',(0.0185992156954128,0.00553349405207063,0.0367740363538192));
#38884=CARTESIAN_POINT('',(0.0193903371194134,-0.000747999597473434,0.0366161087343093));
#38885=CARTESIAN_POINT('',(0.0189904897234335,-0.00398545853288628,0.0365371694116723));
#38886=CARTESIAN_POINT('',(0.016696833777141,-0.00988641562708066,0.0363792913482067));
#38887=CARTESIAN_POINT('',(0.0148052624952997,-0.0125441055225229,0.0363003521432767));
#38888=CARTESIAN_POINT('',(0.00997930898393624,-0.0166420572405772,0.0361424245237952));
#38889=CARTESIAN_POINT('',(0.00705032109213422,-0.018078040606426,0.0360634852011783));
#38890=CARTESIAN_POINT('',(0.000855726728281628,-0.0193853863493642,0.0359056071375901));
#38891=CARTESIAN_POINT('',(-0.00240379359650828,-0.0192554448703678,0.0358266679332148));
#38892=CARTESIAN_POINT('',(-0.00847400777758182,-0.0174566855184124,0.0356687403131495));
#38893=CARTESIAN_POINT('',(-0.0112781694595669,-0.015790043478278,0.0355898009903084));
#38894=CARTESIAN_POINT('',(-0.0157607575092302,-0.01131918706518,0.0354319229308719));
#38895=CARTESIAN_POINT('',(-0.0174347630819637,-0.00851935491177149,0.035352983696314));
#38896=CARTESIAN_POINT('',(-0.0192489951359535,-0.00245374648858159,0.0351950561117514));
#38897=CARTESIAN_POINT('',(-0.019387468746271,0.000805369882804851,0.0351161167829709));
#38898=CARTESIAN_POINT('',(-0.018096358790058,0.00700336721469534,0.0349582385556631));
#38899=CARTESIAN_POINT('',(-0.0166680470003033,0.00993616961891969,0.0348793005385675));
#38900=CARTESIAN_POINT('',(-0.0125823814601453,0.0147725289177495,0.0347213713419553));
#38901=CARTESIAN_POINT('',(-0.00992974481013676,0.0166710547380506,0.034642433347362));
#38902=CARTESIAN_POINT('',(-0.00403488070884202,0.0189802566810074,0.0344845596813018));
#38903=CARTESIAN_POINT('',(-0.000797607311307338,0.0193877129329866,0.0344055828137047));
#38904=CARTESIAN_POINT('',(0.00443737678994076,0.0187430425425944,0.0342740271499158));
#38905=CARTESIAN_POINT('',(0.00648716110805819,0.018136769321841,0.0342214697017214));
#38906=CARTESIAN_POINT('',(0.0102850157450545,0.0162842186741472,0.034116047314547));
#38907=CARTESIAN_POINT('',(0.0120323096863351,0.0150388096576012,0.0340632655330976));
#38908=CARTESIAN_POINT('',(0.0135198806212156,0.0135550334919025,0.0340108594337564));
#38909=CARTESIAN_POINT('',(0.0140292460652998,0.0130469674307547,0.0339929148400313));
#38910=CARTESIAN_POINT('',(0.0145386115093839,0.0125389013696069,0.0339749702463062));
#38911=CARTESIAN_POINT('',(0.0150479769534681,0.0120308353084591,0.0339570256525811));
#38912=CARTESIAN_POINT('',(0.0123579083616226,0.0155369748779275,0.0431499982326393));
#38913=CARTESIAN_POINT('',(0.0128829926152429,0.0150130780695355,0.0431320339636127));
#38914=CARTESIAN_POINT('',(0.0134080768688632,0.0144891812611435,0.0431140696945862));
#38915=CARTESIAN_POINT('',(0.0139331611224835,0.0139652844527515,0.0430961054255596));
#38916=CARTESIAN_POINT('',(0.0154665787885716,0.0124353345148957,0.0430436438876373));
#38917=CARTESIAN_POINT('',(0.0167531705810892,0.0106397945897671,0.0429909630839482));
#38918=CARTESIAN_POINT('',(0.0191517105955881,0.00575220601775009,0.0428590290562634));
#38919=CARTESIAN_POINT('',(0.0198412884492578,0.00246649476446469,0.0427802902482966));
#38920=CARTESIAN_POINT('',(0.0195795672614152,-0.00405098811972438,0.0426224546125279));
#38921=CARTESIAN_POINT('',(0.0186253272917594,-0.00727387508204592,0.0425435404344177));
#38922=CARTESIAN_POINT('',(0.0152913159926029,-0.012883209458447,0.042385492980283));
#38923=CARTESIAN_POINT('',(0.0129169889019614,-0.0152618586794028,0.0423065754957256));
#38924=CARTESIAN_POINT('',(0.00731750168182736,-0.0186072475248359,0.0421487662461117));
#38925=CARTESIAN_POINT('',(0.00409770260301624,-0.0195708558383439,0.0420698594839678));
#38926=CARTESIAN_POINT('',(-0.00242185886210048,-0.0198478911012018,0.0419117993361283));
#38927=CARTESIAN_POINT('',(-0.00571179382904948,-0.0191611066251957,0.0418328929598499));
#38928=CARTESIAN_POINT('',(-0.0115750659571972,-0.0163031656068709,0.0416750818535991));
#38929=CARTESIAN_POINT('',(-0.0141428342863435,-0.0141347036578673,0.041596175228296));
#38930=CARTESIAN_POINT('',(-0.0179406202137328,-0.00882826737024687,0.0414381154495285));
#38931=CARTESIAN_POINT('',(-0.019165091247219,-0.00569840984033663,0.0413592086996603));
#38932=CARTESIAN_POINT('',(-0.0199794247667977,0.000773270772147167,0.0412013976528512));
#38933=CARTESIAN_POINT('',(-0.0195684972398856,0.00410895666889318,0.0411224910179569));
#38934=CARTESIAN_POINT('',(-0.0172033186830933,0.0101906812348328,0.040964431232204));
#38935=CARTESIAN_POINT('',(-0.0152528290560035,0.0129276371826344,0.0408855244900124));
#38936=CARTESIAN_POINT('',(-0.0102803532064448,0.0171490436955882,0.0407277134421433));
#38937=CARTESIAN_POINT('',(-0.00726307273913791,0.018629476200455,0.0406488068074326));
#38938=CARTESIAN_POINT('',(-0.000878026746687795,0.019975816048429,0.0404907470217698));
#38939=CARTESIAN_POINT('',(0.00248007773407933,0.0198399045301169,0.0404118402794289));
#38940=CARTESIAN_POINT('',(0.00873378426508795,0.0179860049520613,0.0402540292316663));
#38941=CARTESIAN_POINT('',(0.0116234487256334,0.016269758721003,0.0401751225968814));
#38942=CARTESIAN_POINT('',(0.016242848459799,0.0116607903540324,0.0400170628112677));
#38943=CARTESIAN_POINT('',(0.0179657769533042,0.00877516129764991,0.039938156068967));
#38944=CARTESIAN_POINT('',(0.019834207640852,0.00252578086536967,0.0397803450210755));
#38945=CARTESIAN_POINT('',(0.0199779204821912,-0.000832047069362478,0.0397014383863677));
#38946=CARTESIAN_POINT('',(0.0186460188421592,-0.00722012043564429,0.0395433786007287));
#38947=CARTESIAN_POINT('',(0.0171726194934967,-0.0102407879122063,0.039464471858345));
#38948=CARTESIAN_POINT('',(0.0129627824089968,-0.0152230625677496,0.0393066608106448));
#38949=CARTESIAN_POINT('',(0.0102303248960628,-0.0171799319451898,0.0392277541758899));
#38950=CARTESIAN_POINT('',(0.00415396286427654,-0.019558853501359,0.0390696943901538));
#38951=CARTESIAN_POINT('',(0.00081928825096348,-0.0199775214705671,0.0389907876480876));
#38952=CARTESIAN_POINT('',(-0.00565426771542406,-0.0191782329298862,0.0388329765998498));
#38953=CARTESIAN_POINT('',(-0.00878700576444731,-0.0179610171988101,0.0387540699653644));
#38954=CARTESIAN_POINT('',(-0.0141020141670623,-0.0141752373594727,0.0385960101796268));
#38955=CARTESIAN_POINT('',(-0.0162764030938681,-0.0116125492318197,0.0385171034373905));
#38956=CARTESIAN_POINT('',(-0.0191479650339184,-0.00575593578666817,0.0383592923894944));
#38957=CARTESIAN_POINT('',(-0.0198423981325784,-0.00246755860460705,0.0382803857547962));
#38958=CARTESIAN_POINT('',(-0.019580104213294,0.00405261357194303,0.0381223259691423));
#38959=CARTESIAN_POINT('',(-0.0186239856370404,0.00727459664337587,0.0380434192268031));
#38960=CARTESIAN_POINT('',(-0.0152916206987856,0.0128818359766005,0.0378856081790289));
#38961=CARTESIAN_POINT('',(-0.0129185204582689,0.0152617639310929,0.0378067015442879));
#38962=CARTESIAN_POINT('',(-0.00731658970352529,0.0186083764170049,0.0376486417585979));
#38963=CARTESIAN_POINT('',(-0.00409630618835518,0.0195702037021567,0.0375697350162963));
#38964=CARTESIAN_POINT('',(0.00242051748217053,0.0198473287079597,0.037411923968483));
#38965=CARTESIAN_POINT('',(0.00571087619192717,0.0191623459481707,0.0373330173337259));
#38966=CARTESIAN_POINT('',(0.0115765136891496,0.0163030208419731,0.0371749575481073));
#38967=CARTESIAN_POINT('',(0.0141430513875155,0.0141331770946469,0.0370960508058741));
#38968=CARTESIAN_POINT('',(0.0179394158558112,0.00882908378426575,0.0369382397578527));
#38969=CARTESIAN_POINT('',(0.0191656268871714,0.00569985571227749,0.0368593331232383));
#38970=CARTESIAN_POINT('',(0.0199800953830214,-0.000774561974363728,0.0367012733375423));
#38971=CARTESIAN_POINT('',(0.0195673380013996,-0.0041099733415498,0.0366223665951662));
#38972=CARTESIAN_POINT('',(0.0172033434382891,-0.0101892264804572,0.0364645555475094));
#38973=CARTESIAN_POINT('',(0.0152543324585768,-0.0129272947815325,0.0363856489127126));
#38974=CARTESIAN_POINT('',(0.0102796390483894,-0.0171503113323094,0.0362275891269953));
#38975=CARTESIAN_POINT('',(0.00726158757166494,-0.0186290617929636,0.0361486823847811));
#38976=CARTESIAN_POINT('',(0.000879258158690037,-0.0199750410971762,0.035990871336678));
#38977=CARTESIAN_POINT('',(-0.00247896880992777,-0.0198409758490944,0.0359119647037807));
#38978=CARTESIAN_POINT('',(-0.00873523608853893,-0.0179861004206441,0.0357539049165843));
#38979=CARTESIAN_POINT('',(-0.0116239141146855,-0.0162682887157641,0.035674998171292));
#38980=CARTESIAN_POINT('',(-0.0162415262239483,-0.0116613973674352,0.0355171871399266));
#38981=CARTESIAN_POINT('',(-0.0179660669468812,-0.0087766758040901,0.0354382803995636));
#38982=CARTESIAN_POINT('',(-0.019835081866255,-0.00252461750601295,0.0352802207143626));
#38983=CARTESIAN_POINT('',(-0.0199769439065618,0.000833241001588936,0.0352013140439823));
#38984=CARTESIAN_POINT('',(-0.0186458014531443,0.00721867902972497,0.0350435023781893));
#38985=CARTESIAN_POINT('',(-0.0171740650283368,0.0102402163951023,0.0349645994515329));
#38986=CARTESIAN_POINT('',(-0.0129622644515052,0.015224425520243,0.0348065356824445));
#38987=CARTESIAN_POINT('',(-0.0102288601536968,0.0171797724257991,0.0347276300560009));
#38988=CARTESIAN_POINT('',(-0.00415512526945464,0.0195580042445408,0.0345698307327648));
#38989=CARTESIAN_POINT('',(-0.000819776313066147,0.0199776088263763,0.0344908525598553));
#38990=CARTESIAN_POINT('',(0.00457554999791865,0.0193123964644629,0.0343592181992749));
#38991=CARTESIAN_POINT('',(0.00668677785486926,0.0186876138390362,0.0343067695837959));
#38992=CARTESIAN_POINT('',(0.0106011348363567,0.0167775405869371,0.0342012224760503));
#38993=CARTESIAN_POINT('',(0.0123997205100048,0.0154952123480511,0.0341485415302033));
#38994=CARTESIAN_POINT('',(0.0139331382238583,0.0139652624610575,0.0340960799060637));
#38995=CARTESIAN_POINT('',(0.0144582022570879,0.0134413858610635,0.034078116299858));
#38996=CARTESIAN_POINT('',(0.0149832662903176,0.0129175092610696,0.0340601526936523));
#38997=CARTESIAN_POINT('',(0.0155083303235472,0.0123936326610756,0.0340421890874466));
#38998=CARTESIAN_POINT('',(0.0125376913185148,0.0157448176443322,0.0436067635510525));
#38999=CARTESIAN_POINT('',(0.013069857522132,0.01521323886892,0.0435887903654682));
#39000=CARTESIAN_POINT('',(0.0136020237257492,0.0146816600935077,0.0435708171798839));
#39001=CARTESIAN_POINT('',(0.0141341899293665,0.0141500813180954,0.0435528439942997));
#39002=CARTESIAN_POINT('',(0.015688289204474,0.0125976975253717,0.0435003564171141));
#39003=CARTESIAN_POINT('',(0.0169910078588997,0.0107772885016299,0.0434477228199255));
#39004=CARTESIAN_POINT('',(0.0194202296550407,0.00581999520554101,0.0433157157855861));
#39005=CARTESIAN_POINT('',(0.0201171636591806,0.00248850671300494,0.0432370143799227));
#39006=CARTESIAN_POINT('',(0.0198479246134623,-0.00411846085620159,0.0430792043811867));
#39007=CARTESIAN_POINT('',(0.0188787232202822,-0.00738525137746305,0.0430003046693479));
#39008=CARTESIAN_POINT('',(0.0154949070329289,-0.0130708753781158,0.0428421985013649));
#39009=CARTESIAN_POINT('',(0.0130863407397065,-0.015480768630216,0.0427632930662205));
#39010=CARTESIAN_POINT('',(0.00740774361997622,-0.0188688364441183,0.0426055158280661));
#39011=CARTESIAN_POINT('',(0.00414307297942253,-0.0198439056459545,0.0425266242112103));
#39012=CARTESIAN_POINT('',(-0.00246761697490749,-0.0201209799677763,0.0423685020300179));
#39013=CARTESIAN_POINT('',(-0.00580243147975463,-0.0194226134955046,0.0422896110657924));
#39014=CARTESIAN_POINT('',(-0.0117447007023978,-0.016521789522652,0.042131831338449));
#39015=CARTESIAN_POINT('',(-0.014346607338881,-0.0143220301077307,0.0420529399532225));
#39016=CARTESIAN_POINT('',(-0.0181942681687709,-0.00893932562358545,0.0418948182511038));
#39017=CARTESIAN_POINT('',(-0.0194335901567592,-0.00576556174660454,0.0418159267887342));
#39018=CARTESIAN_POINT('',(-0.0202552307852466,0.00079570735416269,0.0416581471419614));
#39019=CARTESIAN_POINT('',(-0.0198367739599844,0.0041770907819769,0.0415792557426705));
#39020=CARTESIAN_POINT('',(-0.0174350252151398,0.0103422836945221,0.0414211340314944));
#39021=CARTESIAN_POINT('',(-0.0154559013647298,0.0131156868572235,0.04134224257939));
#39022=CARTESIAN_POINT('',(-0.0104124216457013,0.0173922108962518,0.0411844629311661));
#39023=CARTESIAN_POINT('',(-0.00735276660167522,0.0188913343050469,0.0411055715321491));
#39024=CARTESIAN_POINT('',(-0.000877841710304256,0.0202527116759036,0.0409474498210928));
#39025=CARTESIAN_POINT('',(0.00252643659268623,0.0201127632828363,0.0408685583687824));
#39026=CARTESIAN_POINT('',(0.0088651211044794,0.0182295680747286,0.0407107787207111));
#39027=CARTESIAN_POINT('',(0.0117936096599621,0.0164880702240289,0.0406318873215896));
#39028=CARTESIAN_POINT('',(0.0164747574023958,0.0118120830012056,0.0404737656105987));
#39029=CARTESIAN_POINT('',(0.0182195610466526,0.00888559080746583,0.040394874158353));
#39030=CARTESIAN_POINT('',(0.0201099449649453,0.00254904646741491,0.0402370945100878));
#39031=CARTESIAN_POINT('',(0.020253752763945,-0.000855095025009617,0.0401582031110839));
#39032=CARTESIAN_POINT('',(0.0188995181437999,-0.00733151759369263,0.0400000814000518));
#39033=CARTESIAN_POINT('',(0.0174038741197876,-0.0103928482309152,0.039921189947697));
#39034=CARTESIAN_POINT('',(0.0131330736126197,-0.0154411755340625,0.0397634102996911));
#39035=CARTESIAN_POINT('',(0.0103618958786451,-0.0174234555219608,0.0396845189006242));
#39036=CARTESIAN_POINT('',(0.00419935587391573,-0.0198320030893957,0.0395263971894589));
#39037=CARTESIAN_POINT('',(0.000818472741390671,-0.0202542892027093,0.0394475057375415));
#39038=CARTESIAN_POINT('',(-0.00574372411914673,-0.0194400915024628,0.0392897260887942));
#39039=CARTESIAN_POINT('',(-0.00891891303299861,-0.0182043587867157,0.0392108346900979));
#39040=CARTESIAN_POINT('',(-0.0143058582227063,-0.0143626375295573,0.0390527129789325));
#39041=CARTESIAN_POINT('',(-0.0165085498030464,-0.011763244115922,0.0389738215267757));
#39042=CARTESIAN_POINT('',(-0.0194161122680683,-0.00582426894810843,0.0388160418785074));
#39043=CARTESIAN_POINT('',(-0.020118261990339,-0.00249022549443076,0.038737150479517));
#39044=CARTESIAN_POINT('',(-0.0198484814844665,0.0041207668042561,0.0385790287684607));
#39045=CARTESIAN_POINT('',(-0.018877114557488,0.00738651979706084,0.0385001373161633));
#39046=CARTESIAN_POINT('',(-0.0154954895666888,0.0130689451554609,0.038342357668067));
#39047=CARTESIAN_POINT('',(-0.013088379647488,0.0154803102917281,0.0382634662690125));
#39048=CARTESIAN_POINT('',(-0.00740632255619973,0.0188703291568485,0.0381053445579125));
#39049=CARTESIAN_POINT('',(-0.00414105627275388,0.0198433309117916,0.0380264531056587));
#39050=CARTESIAN_POINT('',(0.00246565331268841,0.020120339910877,0.0378686734575188));
#39051=CARTESIAN_POINT('',(0.00580093170832172,0.0194240798968512,0.0377897820584329));
#39052=CARTESIAN_POINT('',(0.0117467325233343,0.016521416746776,0.0376316603474395));
#39053=CARTESIAN_POINT('',(0.0143472283554195,0.0143200267894043,0.0375527688952839));
#39054=CARTESIAN_POINT('',(0.0181926586425167,0.00894062055461352,0.0373949892468412));
#39055=CARTESIAN_POINT('',(0.0194339974740309,0.00576761915391247,0.0373160978479599));
#39056=CARTESIAN_POINT('',(0.020256029991367,-0.000797612238432598,0.03715797613686));
#39057=CARTESIAN_POINT('',(0.0198354365189604,-0.00417870635836715,0.0370790846845077));
#39058=CARTESIAN_POINT('',(0.0174352289591533,-0.0103402280211969,0.0369213050365665));
#39059=CARTESIAN_POINT('',(0.0154578465385381,-0.0131149025509978,0.0368424136374416));
#39060=CARTESIAN_POINT('',(0.010411264065787,-0.017393921836124,0.0366842919262981));
#39061=CARTESIAN_POINT('',(0.00735068258450235,-0.0188910982815803,0.0366054004741736));
#39062=CARTESIAN_POINT('',(0.00087967408912319,-0.0202517578968002,0.0364476208256344));
#39063=CARTESIAN_POINT('',(-0.00252471609431332,-0.0201139627377015,0.0363687294290392));
#39064=CARTESIAN_POINT('',(-0.00886718657456291,-0.0182295347893614,0.0362106077159948));
#39065=CARTESIAN_POINT('',(-0.0117945519274473,-0.0164861964499937,0.036131716259469));
#39066=CARTESIAN_POINT('',(-0.016472956754427,-0.0118130953090526,0.0359739366335474));
#39067=CARTESIAN_POINT('',(-0.0182196238625896,-0.00888768738915584,0.0358950450932448));
#39068=CARTESIAN_POINT('',(-0.0201110470261814,-0.00254729901032419,0.0357369235135449));
#39069=CARTESIAN_POINT('',(-0.0202526988688433,0.000856909313547677,0.0356580321690692));
#39070=CARTESIAN_POINT('',(-0.0188993787123355,0.00732945390426337,0.035500251691036));
#39071=CARTESIAN_POINT('',(-0.0174056823841494,0.0103917663907847,0.0354213651815531));
#39072=CARTESIAN_POINT('',(-0.0131321880026628,0.015443052118062,0.0352632383541236));
#39073=CARTESIAN_POINT('',(-0.0103598867730791,0.0174235644042914,0.0351843479349766));
#39074=CARTESIAN_POINT('',(-0.00420107043822686,0.0198308773727001,0.0350265834252997));
#39075=CARTESIAN_POINT('',(-0.000819557590625485,0.0202544098310457,0.0349476046181466));
#39076=CARTESIAN_POINT('',(0.00465054363677044,0.0195767431377992,0.0348159334247739));
#39077=CARTESIAN_POINT('',(0.0067902080359049,0.0189421083623588,0.0347635357583031));
#39078=CARTESIAN_POINT('',(0.0107581630684882,0.0170030639864308,0.0346579301873415));
#39079=CARTESIAN_POINT('',(0.0125800788597369,0.0157024545619653,0.0346052965200256));
#39080=CARTESIAN_POINT('',(0.0141341782018793,0.0141500708378154,0.0345528089000304));
#39081=CARTESIAN_POINT('',(0.0146663239187657,0.013618512572929,0.0345348363924741));
#39082=CARTESIAN_POINT('',(0.0151984696356521,0.0130869543080425,0.0345168638849177));
#39083=CARTESIAN_POINT('',(0.0157306153525384,0.012555396043156,0.0344988913773613));
#39084=CARTESIAN_POINT('',(0.0125465175185849,0.0157377537294883,0.0440539195793887));
#39085=CARTESIAN_POINT('',(0.0130783902203003,0.0152058810275692,0.0440359463862592));
#39086=CARTESIAN_POINT('',(0.0136102629220156,0.0146740083256501,0.0440179731931296));
#39087=CARTESIAN_POINT('',(0.0141421356237309,0.014142135623731,0.044));
#39088=CARTESIAN_POINT('',(0.0156953777773417,0.0125888934695251,0.0439475124007797));
#39089=CARTESIAN_POINT('',(0.0169970423533304,0.0107677303981291,0.0438948787697366));
#39090=CARTESIAN_POINT('',(0.0194235570551383,0.0058091099397162,0.0437628717686972));
#39091=CARTESIAN_POINT('',(0.0201185695458997,0.00247720350148128,0.0436841704089366));
#39092=CARTESIAN_POINT('',(0.01984559628717,-0.00412961236453083,0.0435263603675614));
#39093=CARTESIAN_POINT('',(0.0188745457210623,-0.00739584186127215,0.0434474606693054));
#39094=CARTESIAN_POINT('',(0.0154875898783386,-0.0130795979874077,0.0432893544847642));
#39095=CARTESIAN_POINT('',(0.0130776532928583,-0.0154881380856146,0.0432104490779356));
#39096=CARTESIAN_POINT('',(0.00739713377664075,-0.0188729847428303,0.0430526718436316));
#39097=CARTESIAN_POINT('',(0.00413192193560115,-0.0198462007289697,0.0429737801981818));
#39098=CARTESIAN_POINT('',(-0.00247892142177586,-0.0201196295423519,0.0428156580158873));
#39099=CARTESIAN_POINT('',(-0.00581335213997824,-0.0194193705481011,0.0427367670786146));
#39100=CARTESIAN_POINT('',(-0.0117539766613564,-0.0165151764007151,0.0425789873520905));
#39101=CARTESIAN_POINT('',(-0.0143546277377461,-0.0143139501213873,0.0425000959407626));
#39102=CARTESIAN_POINT('',(-0.0181993204388129,-0.00892912321441055,0.0423419742368419));
#39103=CARTESIAN_POINT('',(-0.0194368483323084,-0.00575464561573629,0.0422630828015258));
#39104=CARTESIAN_POINT('',(-0.0202547679627867,0.00080708991130746,0.0421053031556577));
#39105=CARTESIAN_POINT('',(-0.019834396408894,0.00418822452499619,0.0420264117301959));
#39106=CARTESIAN_POINT('',(-0.0174292474333672,0.0103520934760813,0.0418682900172373));
#39107=CARTESIAN_POINT('',(-0.0154485447986849,0.0131243850498825,0.0417893985921814));
#39108=CARTESIAN_POINT('',(-0.0104026394106094,0.0173980491055669,0.0416316189448621));
#39109=CARTESIAN_POINT('',(-0.00734214540805515,0.0188954334792125,0.0415527275196745));
#39110=CARTESIAN_POINT('',(-0.000866469142916212,0.0202532401525842,0.0413946058068358));
#39111=CARTESIAN_POINT('',(0.00253774208826097,0.0201113620728414,0.0413157143815739));
#39112=CARTESIAN_POINT('',(0.00887535903306692,0.0182245719132231,0.0411579347344072));
#39113=CARTESIAN_POINT('',(0.01180285059346,0.0164814205525399,0.041079043309115));
#39114=CARTESIAN_POINT('',(0.0164814200301334,0.0118028513183548,0.0409209215963417));
#39115=CARTESIAN_POINT('',(0.0182245715205425,0.00887535983630872,0.0408420301711456));
#39116=CARTESIAN_POINT('',(0.0201113619622517,0.00253774297547744,0.0406842505237827));
#39117=CARTESIAN_POINT('',(0.0202532401934251,-0.000866468250329324,0.0406053590986105));
#39118=CARTESIAN_POINT('',(0.0188954338003623,-0.00734214457422893,0.0404472373857936));
#39119=CARTESIAN_POINT('',(0.0173980495632035,-0.0104026386425633,0.0403683459604884));
#39120=CARTESIAN_POINT('',(0.0131243857321058,-0.0154485442207657,0.0402105663133872));
#39121=CARTESIAN_POINT('',(0.0103520942461436,-0.0174292469797191,0.0401316748881496));
#39122=CARTESIAN_POINT('',(0.00418822539793767,-0.01983439622144,0.0399735531752019));
#39123=CARTESIAN_POINT('',(0.00080709080647619,-0.0202547679266353,0.039894661750333));
#39124=CARTESIAN_POINT('',(-0.00575464475690967,-0.0194368485899185,0.0397368821024903));
#39125=CARTESIAN_POINT('',(-0.00892912243213517,-0.0181993208157078,0.0396579906776233));
#39126=CARTESIAN_POINT('',(-0.0143139494659693,-0.0143546283873442,0.0394998689646755));
#39127=CARTESIAN_POINT('',(-0.0165151759031107,-0.0117539773787766,0.0394209775395684));
#39128=CARTESIAN_POINT('',(-0.0194193704330004,-0.00581335285115579,0.0392631978922023));
#39129=CARTESIAN_POINT('',(-0.0201196283819678,-0.00247892301874085,0.0391843064670424));
#39130=CARTESIAN_POINT('',(-0.019846201989664,0.00413192110745882,0.0390261847542038));
#39131=CARTESIAN_POINT('',(-0.0188729808890436,0.00739713537075163,0.0389472933289547));
#39132=CARTESIAN_POINT('',(-0.0154881330235243,0.0130776433210231,0.0387895136817632));
#39133=CARTESIAN_POINT('',(-0.0130796649391004,0.0154876360572498,0.0387106222565379));
#39134=CARTESIAN_POINT('',(-0.00739573778198963,0.0188745216658114,0.0385525005436556));
#39135=CARTESIAN_POINT('',(-0.00412990836797088,0.019845676511613,0.0384736091184501));
#39136=CARTESIAN_POINT('',(0.00247695877305382,0.0201189387051795,0.0383158294712149));
#39137=CARTESIAN_POINT('',(0.00581183108735372,0.019420791049107,0.0382369380459571));
#39138=CARTESIAN_POINT('',(0.0117560316740477,0.0165148486136556,0.0380788163331838));
#39139=CARTESIAN_POINT('',(0.0143552893388841,0.0143119770586781,0.0379999249080766));
#39140=CARTESIAN_POINT('',(0.0181976691008663,0.00893038961533982,0.0378421452605361));
#39141=CARTESIAN_POINT('',(0.0194372055562126,0.00575669572993267,0.0377632538354854));
#39142=CARTESIAN_POINT('',(0.0202556175238696,-0.000808989603994321,0.0376051321226031));
#39143=CARTESIAN_POINT('',(0.0198331064944038,-0.00418985752894618,0.0375262406973004));
#39144=CARTESIAN_POINT('',(0.0174294044206095,-0.0103500184023128,0.0373684610502614));
#39145=CARTESIAN_POINT('',(0.0154504564687845,-0.0131235627964765,0.0372895696249671));
#39146=CARTESIAN_POINT('',(0.0104015137184082,-0.0173997993613175,0.0371314479120412));
#39147=CARTESIAN_POINT('',(0.00734007279563755,-0.0188952467752599,0.0370525564869662));
#39148=CARTESIAN_POINT('',(0.000868292189651466,-0.0202522366194585,0.0368947768393292));
#39149=CARTESIAN_POINT('',(-0.00253600814635427,-0.0201125127235025,0.0368158854165646));
#39150=CARTESIAN_POINT('',(-0.0088774399761798,-0.018224586826797,0.0366577637017353));
#39151=CARTESIAN_POINT('',(-0.0118038279130671,-0.0164795833028888,0.0365788722722735));
#39152=CARTESIAN_POINT('',(-0.0164795828284599,-0.0118038285955315,0.0364210926472371));
#39153=CARTESIAN_POINT('',(-0.0182245861741416,-0.00887744099613647,0.0363422010807297));
#39154=CARTESIAN_POINT('',(-0.0201125128390728,-0.00253600893042723,0.0361840794994547));
#39155=CARTESIAN_POINT('',(-0.0202522359742467,0.000868291897198348,0.0361051881812469));
#39156=CARTESIAN_POINT('',(-0.0188952453448132,0.00734006951024311,0.0359474077050742));
#39157=CARTESIAN_POINT('',(-0.0173998172706736,0.0104015239313007,0.0358685211701349));
#39158=CARTESIAN_POINT('',(-0.013123538002664,0.0154504543843868,0.0357103943350004));
#39159=CARTESIAN_POINT('',(-0.0103501050287235,0.0174294035933487,0.03563150396077));
#39160=CARTESIAN_POINT('',(-0.00418992058649385,0.0198332176625935,0.0354737394315266));
#39161=CARTESIAN_POINT('',(-0.000808179644509043,0.0202548576790242,0.0353947606000568));
#39162=CARTESIAN_POINT('',(0.00466154596368762,0.0195741550782838,0.035263089448488));
#39163=CARTESIAN_POINT('',(0.00680083319771015,0.0189382544178338,0.035210691736618));
#39164=CARTESIAN_POINT('',(0.0107677296476345,0.0169970428264161,0.0351050861356576));
#39165=CARTESIAN_POINT('',(0.0125888927781881,0.0156953783332082,0.0350524525049133));
#39166=CARTESIAN_POINT('',(0.0141421349996867,0.0141421362469037,0.0349999649054552));
#39167=CARTESIAN_POINT('',(0.0146739872262749,0.013610284066608,0.034981992404931));
#39168=CARTESIAN_POINT('',(0.015205839452863,0.0130784318863123,0.0349640199044069));
#39169=CARTESIAN_POINT('',(0.0157376916794511,0.0125465797060166,0.0349460474038827));
#39170=CARTESIAN_POINT('',(0.0125553467792133,0.0157306873651733,0.0445012306627941));
#39171=CARTESIAN_POINT('',(0.0130869258772525,0.0151985206348258,0.0444832574621166));
#39172=CARTESIAN_POINT('',(0.0136185049752917,0.0146663539044784,0.0444652842614391));
#39173=CARTESIAN_POINT('',(0.0141500840733309,0.014134187174131,0.0444473110607616));
#39174=CARTESIAN_POINT('',(0.0157024688082309,0.012580086360799,0.0443948234394989));
#39175=CARTESIAN_POINT('',(0.0170030789402721,0.0107581689802764,0.0443421897745895));
#39176=CARTESIAN_POINT('',(0.0194268856090395,0.005798220899335,0.0442101828068617));
#39177=CARTESIAN_POINT('',(0.0201199759201218,0.00246589637047508,0.0441314814930198));
#39178=CARTESIAN_POINT('',(0.0198432671535113,-0.00414076773973825,0.0439736714089908));
#39179=CARTESIAN_POINT('',(0.0188703667732599,-0.00740643601741953,0.0438947717243222));
#39180=CARTESIAN_POINT('',(0.0154802701864641,-0.0130883236213368,0.043736665523217));
#39181=CARTESIAN_POINT('',(0.0130689628335657,-0.015495510096433,0.0436577601447141));
#39182=CARTESIAN_POINT('',(0.00738652025425392,-0.0188771344799994,0.0434999829142618));
#39183=CARTESIAN_POINT('',(0.00412076702506264,-0.019848496607824,0.0434210912402082));
#39184=CARTESIAN_POINT('',(-0.00249022978855514,-0.0201182786486563,0.0432629690568112));
#39185=CARTESIAN_POINT('',(-0.00582427658703155,-0.0194161264761786,0.0431840781465005));
#39186=CARTESIAN_POINT('',(-0.0117632558368309,-0.0165085609856232,0.0430262984207961));
#39187=CARTESIAN_POINT('',(-0.0143626509177512,-0.0143058673332415,0.0429474069833575));
#39188=CARTESIAN_POINT('',(-0.0182043744607715,-0.00891891726746548,0.0427892852776344));
#39189=CARTESIAN_POINT('',(-0.0194401076376572,-0.00574372569960893,0.0427103938693811));
#39190=CARTESIAN_POINT('',(-0.0202543049798394,0.00081847641544852,0.0425526142244181));
#39191=CARTESIAN_POINT('',(-0.019832018033368,0.00419936212873341,0.0424737227727762));
#39192=CARTESIAN_POINT('',(-0.0174234676481007,0.0103619066592638,0.0423156010580346));
#39193=CARTESIAN_POINT('',(-0.0154411856816897,0.013133086258712,0.0422367096600366));
#39194=CARTESIAN_POINT('',(-0.0103928537834461,0.0174038893393296,0.0420789300136223));
#39195=CARTESIAN_POINT('',(-0.00733152053144792,0.0188995340748007,0.0420000385622549));
#39196=CARTESIAN_POINT('',(-0.000855092631995909,0.0202537688125186,0.0418419168476332));
#39197=CARTESIAN_POINT('',(0.00254905150411026,0.0201099603769654,0.041763025449429));
#39198=CARTESIAN_POINT('',(0.00888560051174127,0.018219574019257,0.0416052458031673));
#39199=CARTESIAN_POINT('',(0.0118120947313283,0.0164747685752221,0.0415263543516954));
#39200=CARTESIAN_POINT('',(0.0164880849681926,0.0117936164343411,0.0413682326371391));
#39201=CARTESIAN_POINT('',(0.0182295837318557,0.00886512531747734,0.041289341239002));
#39202=CARTESIAN_POINT('',(0.0201127794509136,0.0025264355639602,0.0411315615925416));
#39203=CARTESIAN_POINT('',(0.0202527274451672,-0.000877845419409433,0.0410526701411921));
#39204=CARTESIAN_POINT('',(0.0188913480406447,-0.00735277523975905,0.0408945484265898));
#39205=CARTESIAN_POINT('',(0.0173922229869061,-0.010412432449118,0.0408156570283436));
#39206=CARTESIAN_POINT('',(0.013115694838997,-0.0154559154626221,0.0406578773821473));
#39207=CARTESIAN_POINT('',(0.0103422892148445,-0.0174350404457136,0.04057898593073));
#39208=CARTESIAN_POINT('',(0.00417709106237456,-0.0198367901833228,0.0404208642159993));
#39209=CARTESIAN_POINT('',(0.000795704924781183,-0.0202552468165628,0.0403419728181881));
#39210=CARTESIAN_POINT('',(-0.00576556918149452,-0.0194336045528674,0.0401841931712504));
#39211=CARTESIAN_POINT('',(-0.00893933537146573,-0.0181942810977416,0.0401053017202037));
#39212=CARTESIAN_POINT('',(-0.0143220435149382,-0.0143466164678946,0.0399471800054729));
#39213=CARTESIAN_POINT('',(-0.0165218043008303,-0.0117447074283131,0.0398682886074247));
#39214=CARTESIAN_POINT('',(-0.0194226297277284,-0.00580243296895581,0.0397105089609612));
#39215=CARTESIAN_POINT('',(-0.0201209952474043,-0.00246761662382356,0.0396316175096228));
#39216=CARTESIAN_POINT('',(-0.0198439217044277,0.00414307927850888,0.0394734957950011));
#39217=CARTESIAN_POINT('',(-0.0188688457872152,0.00740775462548082,0.0393946043968098));
#39218=CARTESIAN_POINT('',(-0.0154807739294173,0.0130863445027465,0.0392368247505233));
#39219=CARTESIAN_POINT('',(-0.0130709472088153,0.0154949643630416,0.0391579332991183));
#39220=CARTESIAN_POINT('',(-0.0073851493374211,0.0188787156285615,0.0389998115844529));
#39221=CARTESIAN_POINT('',(-0.00411875659755924,0.0198480229247906,0.0389209201863052));
#39222=CARTESIAN_POINT('',(0.00248826815368158,0.0201175370136022,0.038763140539975));
#39223=CARTESIAN_POINT('',(0.00582273424583599,0.0194175010609274,0.0386842490885363));
#39224=CARTESIAN_POINT('',(0.0117653340493188,0.0165082782029806,0.0385261273739824));
#39225=CARTESIAN_POINT('',(0.0143633531175618,0.0143039245366409,0.0384472359759329));
#39226=CARTESIAN_POINT('',(0.0182026812966341,0.0089201551284029,0.038289456329295));
#39227=CARTESIAN_POINT('',(0.0194404147508235,0.00574576851816482,0.0382105648780657));
#39228=CARTESIAN_POINT('',(0.0202552049133456,-0.00082037091475211,0.0380524431634004));
#39229=CARTESIAN_POINT('',(0.0198307756618918,-0.00420101256628627,0.0379735517651567));
#39230=CARTESIAN_POINT('',(0.0174235778623587,-0.0103598121783247,0.0378157721190203));
#39231=CARTESIAN_POINT('',(0.0154430638364627,-0.0131322260449673,0.0377368806675474));
#39232=CARTESIAN_POINT('',(0.0103917599900155,-0.0174056789245918,0.0375787589528385));
#39233=CARTESIAN_POINT('',(0.00732945932774028,-0.0188993967074641,0.0374998675548225));
#39234=CARTESIAN_POINT('',(0.000856906343411505,-0.0202527155081179,0.0373420879080881));
#39235=CARTESIAN_POINT('',(-0.00254730411400811,-0.020111062206499,0.037263196459145));
#39236=CARTESIAN_POINT('',(-0.00888769693324891,-0.0182196371484855,0.0371050747425303));
#39237=CARTESIAN_POINT('',(-0.0118131071152121,-0.0164729678626203,0.0370261833401418));
#39238=CARTESIAN_POINT('',(-0.0164862112001391,-0.0117945586687005,0.0368684037159908));
#39239=CARTESIAN_POINT('',(-0.0182295502064164,-0.00886719105009516,0.0367895121232697));
#39240=CARTESIAN_POINT('',(-0.0201139791602471,-0.00252471493560122,0.036631390540419));
#39241=CARTESIAN_POINT('',(-0.0202517729191377,0.0008796784278545,0.0365524992484881));
#39242=CARTESIAN_POINT('',(-0.0188911105440114,0.00735068879727244,0.0363947187741767));
#39243=CARTESIAN_POINT('',(-0.017393950123421,0.0104112848553249,0.036315832213772));
#39244=CARTESIAN_POINT('',(-0.0131148850032058,0.015457859217509,0.0361577053709299));
#39245=CARTESIAN_POINT('',(-0.0103403198924667,0.0174352448071932,0.0360788150416316));
#39246=CARTESIAN_POINT('',(-0.00417876686845709,0.0198355587640019,0.0359210504928149));
#39247=CARTESIAN_POINT('',(-0.000796797752995223,0.0202553056822977,0.0358420716370199));
#39248=CARTESIAN_POINT('',(0.0046725521057531,0.0195715661213371,0.0357104005272695));
#39249=CARTESIAN_POINT('',(0.00681146204387857,0.0189343991369214,0.0356580027699848));
#39250=CARTESIAN_POINT('',(0.0107772995440717,0.0169910195785142,0.035552397139015));
#39251=CARTESIAN_POINT('',(0.0125977097529387,0.01568829965071,0.0354997635448551));
#39252=CARTESIAN_POINT('',(0.0141500945565799,0.0141341989046066,0.0354472759659412));
#39253=CARTESIAN_POINT('',(0.0146816531910996,0.013602052706984,0.0354293034724516));
#39254=CARTESIAN_POINT('',(0.0152132118256192,0.0130699065093615,0.0354113309789621));
#39255=CARTESIAN_POINT('',(0.0157447704601389,0.0125377603117389,0.0353933584854725));
#39256=CARTESIAN_POINT('',(0.0123934894645848,0.0155082763123231,0.0449580753891009));
#39257=CARTESIAN_POINT('',(0.012917382287782,0.0149831956652547,0.0449401110951834));
#39258=CARTESIAN_POINT('',(0.0134412751109791,0.0144581150181862,0.0449221468012659));
#39259=CARTESIAN_POINT('',(0.0139651679341763,0.0139330343711178,0.0449041825073484));
#39260=CARTESIAN_POINT('',(0.0154951062339604,0.0123996272373401,0.0448517208967365));
#39261=CARTESIAN_POINT('',(0.016777425009008,0.010601053512311,0.0447990399263663));
#39262=CARTESIAN_POINT('',(0.0191649977879812,0.00570814164951054,0.0446671060793837));
#39263=CARTESIAN_POINT('',(0.0198468001189922,0.00242076902532767,0.0445883674334732));
#39264=CARTESIAN_POINT('',(0.0195699819612324,-0.0040960439270075,0.0444305316090981));
#39265=CARTESIAN_POINT('',(0.0186082730960355,-0.00731663434116805,0.0443516174767989));
#39266=CARTESIAN_POINT('',(0.015261595968773,-0.0129183666546227,0.0441935699927201));
#39267=CARTESIAN_POINT('',(0.0128817488018725,-0.0152915238210584,0.0441146526150789));
#39268=CARTESIAN_POINT('',(0.00727453700603762,-0.0186238589222907,0.0439568433608528));
#39269=CARTESIAN_POINT('',(0.00405257752468377,-0.0195799653309641,0.0438779364735199));
#39270=CARTESIAN_POINT('',(-0.00246754686692629,-0.0198422575935462,0.0437198763603395));
#39271=CARTESIAN_POINT('',(-0.00575590144654004,-0.01914782678123,0.0436409700833429));
#39272=CARTESIAN_POINT('',(-0.0116124723502935,-0.0162762833167919,0.0434831589606206));
#39273=CARTESIAN_POINT('',(-0.0141751414837983,-0.0141019088846481,0.0434042522201484));
#39274=CARTESIAN_POINT('',(-0.0179608924119463,-0.00878693729344424,0.0432461924731406));
#39275=CARTESIAN_POINT('',(-0.0191780984979996,-0.00565422105111067,0.0431672858230386));
#39276=CARTESIAN_POINT('',(-0.0199773791436797,0.000819289371129895,0.043009474760093));
#39277=CARTESIAN_POINT('',(-0.0195587129181748,0.0041539402136244,0.0429305680097516));
#39278=CARTESIAN_POINT('',(-0.0171798063834406,0.0102302578552052,0.0427725082558356));
#39279=CARTESIAN_POINT('',(-0.0152229499734908,0.0129626953923687,0.0426936016133913));
#39280=CARTESIAN_POINT('',(-0.0102407091285208,0.0171725009568401,0.0425357905493827));
#39281=CARTESIAN_POINT('',(-0.00722006250668779,0.0186458887612477,0.0424568837992276));
#39282=CARTESIAN_POINT('',(-0.000832034517765779,0.0199777786987247,0.0422988240454017));
#39283=CARTESIAN_POINT('',(0.00252576960124855,0.0198340657872349,0.0422199174028092));
#39284=CARTESIAN_POINT('',(0.00877510515323934,0.0179656461646544,0.0420621063389043));
#39285=CARTESIAN_POINT('',(0.0116607131388107,0.0162427288161061,0.0419831995886749));
#39286=CARTESIAN_POINT('',(0.0162696468896929,0.0116233606696467,0.041825139834901));
#39287=CARTESIAN_POINT('',(0.0179858800358563,0.00873371610839782,0.0417462331923493));
#39288=CARTESIAN_POINT('',(0.0198397643303848,0.00248005320174727,0.0415884221283116));
#39289=CARTESIAN_POINT('',(0.0199756736539967,-0.000878027543581936,0.0415095153781676));
#39290=CARTESIAN_POINT('',(0.0186293413170257,-0.00726302727977779,0.0413514556243556));
#39291=CARTESIAN_POINT('',(0.0171489183145194,-0.0102802859091026,0.0412725489817254));
#39292=CARTESIAN_POINT('',(0.0129275399628127,-0.0152527251032007,0.0411147379178828));
#39293=CARTESIAN_POINT('',(0.0101906026857989,-0.0172031999115253,0.0410358311676849));
#39294=CARTESIAN_POINT('',(0.00410892095107614,-0.019568359455848,0.0408777714137857));
#39295=CARTESIAN_POINT('',(0.000773258535901459,-0.0199792829940002,0.0407988647714664));
#39296=CARTESIAN_POINT('',(-0.005698375986877,-0.0191649530051426,0.0406410537070893));
#39297=CARTESIAN_POINT('',(-0.008828210915612,-0.0179404894672697,0.0405621469571608));
#39298=CARTESIAN_POINT('',(-0.0141346078249767,-0.0141427290439189,0.0404040872032571));
#39299=CARTESIAN_POINT('',(-0.0163030536505294,-0.0115749781595783,0.0403251805607742));
#39300=CARTESIAN_POINT('',(-0.019160972463498,-0.00571174638979979,0.0401673694967289));
#39301=CARTESIAN_POINT('',(-0.0198477500854794,-0.00242183542833849,0.0400884627465911));
#39302=CARTESIAN_POINT('',(-0.0195707163823238,0.00409768025304344,0.0399304029927742));
#39303=CARTESIAN_POINT('',(-0.0186071088678102,0.00731745702488812,0.0398514963501819));
#39304=CARTESIAN_POINT('',(-0.0152617412065595,0.0129168946697514,0.0396936852862684));
#39305=CARTESIAN_POINT('',(-0.0128831697885874,0.0152912526136711,0.0396147785360814));
#39306=CARTESIAN_POINT('',(-0.00727372673197496,0.0186251663778611,0.0394567187822312));
#39307=CARTESIAN_POINT('',(-0.00405119419586402,0.0195795174434124,0.0393778121396736));
#39308=CARTESIAN_POINT('',(0.00246620997808876,0.0198414898863339,0.0392200010757239));
#39309=CARTESIAN_POINT('',(0.00575489811217428,0.0191488803332586,0.0391410943255175));
#39310=CARTESIAN_POINT('',(0.011614013504857,0.0162763206370897,0.0389830345717425));
#39311=CARTESIAN_POINT('',(0.0141755224604208,0.0141005049802241,0.0389041279292564));
#39312=CARTESIAN_POINT('',(0.0179595192168192,0.00878763802580743,0.0387463168650887));
#39313=CARTESIAN_POINT('',(0.0191784316338705,0.00565563704304498,0.0386674101150348));
#39314=CARTESIAN_POINT('',(0.0199782533217446,-0.000820559190878668,0.0385093503611727));
#39315=CARTESIAN_POINT('',(0.0195577459963842,-0.00415502698829191,0.0384304437185515));
#39316=CARTESIAN_POINT('',(0.0171796419344795,-0.0102287250214563,0.0382726326547425));
#39317=CARTESIAN_POINT('',(0.0152243176035623,-0.0129621998058823,0.0381937259045076));
#39318=CARTESIAN_POINT('',(0.0102401242086823,-0.017173927313282,0.0380356661506272));
#39319=CARTESIAN_POINT('',(0.00721862383931954,-0.0186456736966964,0.0379567595081661));
#39320=CARTESIAN_POINT('',(0.000833227810519059,-0.0199768026475956,0.0377989484439109));
#39321=CARTESIAN_POINT('',(-0.00252460669506535,-0.0198349396539981,0.0377200416955754));
#39322=CARTESIAN_POINT('',(-0.00877661916499571,-0.0179659366380679,0.0375619819402062));
#39323=CARTESIAN_POINT('',(-0.0116613199831515,-0.0162414067754668,0.0374830752947276));
#39324=CARTESIAN_POINT('',(-0.016268177126898,-0.011623825758288,0.0373252642471344));
#39325=CARTESIAN_POINT('',(-0.0179859753970511,-0.00873516787953567,0.0372463573912147));
#39326=CARTESIAN_POINT('',(-0.019840835829584,-0.00247894445095143,0.0370882977386692));
#39327=CARTESIAN_POINT('',(-0.0199748980239041,0.000879258931138491,0.0370093911648565));
#39328=CARTESIAN_POINT('',(-0.0186289256182034,0.0072615402658288,0.0368515794869236));
#39329=CARTESIAN_POINT('',(-0.0171501996025803,0.0102795817780441,0.0367726764469661));
#39330=CARTESIAN_POINT('',(-0.0129271754315416,0.0152542235327993,0.0366146126864771));
#39331=CARTESIAN_POINT('',(-0.0101892187172689,0.0172032332553386,0.0365357072320943));
#39332=CARTESIAN_POINT('',(-0.00411000464968758,0.0195672966718648,0.0363779078077777));
#39333=CARTESIAN_POINT('',(-0.000773762353009196,0.0199792454619298,0.0362989295369263));
#39334=CARTESIAN_POINT('',(0.00461999775143137,0.0193017632934899,0.0361672953686332));
#39335=CARTESIAN_POINT('',(0.00672968236710639,0.0186718674536964,0.0361148465374304));
#39336=CARTESIAN_POINT('',(0.0106397244891325,0.0167530479282312,0.036009299345223));
#39337=CARTESIAN_POINT('',(0.0124352515814873,0.0154664643618175,0.0359566185174661));
#39338=CARTESIAN_POINT('',(0.0139651899324739,0.0139330572761716,0.0359041569927753));
#39339=CARTESIAN_POINT('',(0.014489062582375,0.0134079968821915,0.0358861934206222));
#39340=CARTESIAN_POINT('',(0.0150129352322761,0.0128829364882113,0.0358682298484692));
#39341=CARTESIAN_POINT('',(0.0155368078821772,0.0123578760942311,0.0358502662763162));
#39342=CARTESIAN_POINT('',(0.0120305257775094,0.015047717626688,0.0450430352084097));
#39343=CARTESIAN_POINT('',(0.0125386004906958,0.0145383434030553,0.0450250899362179));
#39344=CARTESIAN_POINT('',(0.0130466752038823,0.0140289691794226,0.0450071446640261));
#39345=CARTESIAN_POINT('',(0.0135547499170688,0.0135195949557899,0.0449891993918343));
#39346=CARTESIAN_POINT('',(0.015038494164818,0.0120320557127389,0.0449367933308794));
#39347=CARTESIAN_POINT('',(0.0162838776612131,0.0102847972275788,0.0448840114797136));
#39348=CARTESIAN_POINT('',(0.0185995162676072,0.0055375795976936,0.0447522336035345));
#39349=CARTESIAN_POINT('',(0.0192610546483522,0.00234696454026363,0.0446734152009566));
#39350=CARTESIAN_POINT('',(0.0189914348903327,-0.00397841114725085,0.0445155245324582));
#39351=CARTESIAN_POINT('',(0.0180572885482573,-0.00710392355101288,0.0444365795423942));
#39352=CARTESIAN_POINT('',(0.0148095155549984,-0.0125383247637423,0.0442786573913219));
#39353=CARTESIAN_POINT('',(0.0124995304672202,-0.0148415576411829,0.0441997143515908));
#39354=CARTESIAN_POINT('',(0.00705668445210766,-0.0180751219128047,0.0440418367521038));
#39355=CARTESIAN_POINT('',(0.00392925637374929,-0.0190023614305585,0.0439628974570812));
#39356=CARTESIAN_POINT('',(-0.00239664418868276,-0.0192559260685448,0.0438049698017331));
#39357=CARTESIAN_POINT('',(-0.00558825700628719,-0.0185817388652116,0.0437260306791333));
#39358=CARTESIAN_POINT('',(-0.0112722447088396,-0.015793772453778,0.0435681525546579));
#39359=CARTESIAN_POINT('',(-0.0137590407905356,-0.0136827495892477,0.0434892132100029));
#39360=CARTESIAN_POINT('',(-0.0174312553179828,-0.00852560155963431,0.0433312856842805));
#39361=CARTESIAN_POINT('',(-0.0186124958588404,-0.00548494660580613,0.0432523464547741));
#39362=CARTESIAN_POINT('',(-0.0193873503391936,0.000798370606699635,0.0430944683451649));
#39363=CARTESIAN_POINT('',(-0.0189802212997522,0.0040348530646949,0.0430155290000279));
#39364=CARTESIAN_POINT('',(-0.0166713408352946,0.00992980053306335,0.0428576014718638));
#39365=CARTESIAN_POINT('',(-0.0147718837601594,0.0125817761690868,0.0427786622444798));
#39366=CARTESIAN_POINT('',(-0.00993550644959224,0.0166671071404195,0.0426207841346389));
#39367=CARTESIAN_POINT('',(-0.00700335335034363,0.0180964604736507,0.0425418447894979));
#39368=CARTESIAN_POINT('',(-0.000805463021044599,0.0193877738074862,0.0423839172613603));
#39369=CARTESIAN_POINT('',(0.00245358663115674,0.0192481052063996,0.0423049780339514));
#39370=CARTESIAN_POINT('',(0.00851893643492141,0.0174337164957497,0.0421470999241113));
#39371=CARTESIAN_POINT('',(0.0113192788681312,0.0157607983849654,0.0420681605789608));
#39372=CARTESIAN_POINT('',(0.01579024780393,0.0112784138147657,0.0419102330508445));
#39373=CARTESIAN_POINT('',(0.0174558531374492,0.00847365521083588,0.0418312938234208));
#39374=CARTESIAN_POINT('',(0.019254339634141,0.00240357111284854,0.0416734157135893));
#39375=CARTESIAN_POINT('',(0.0193854708067216,-0.000855781179293895,0.0415944763684416));
#39376=CARTESIAN_POINT('',(0.0180783569263752,-0.00705035848239528,0.0414365488403111));
#39377=CARTESIAN_POINT('',(0.0166413068129427,-0.0099788049861067,0.0413576096128707));
#39378=CARTESIAN_POINT('',(0.0125433147624612,-0.014804458909604,0.0411997315030867));
#39379=CARTESIAN_POINT('',(0.0098864162360075,-0.0166969342644347,0.0411207921579174));
#39380=CARTESIAN_POINT('',(0.00398560024159757,-0.0189907749869355,0.0409628646297827));
#39381=CARTESIAN_POINT('',(0.00074801108265274,-0.019389433225327,0.040883925402392));
#39382=CARTESIAN_POINT('',(-0.00553325382190865,-0.0185981141783993,0.0407260472925128));
#39383=CARTESIAN_POINT('',(-0.00857075650521062,-0.0174089337051664,0.040647107947397));
#39384=CARTESIAN_POINT('',(-0.0137185235041463,-0.0137235803184355,0.0404891804192505));
#39385=CARTESIAN_POINT('',(-0.015823060245059,-0.0112312245935179,0.0404102411918493));
#39386=CARTESIAN_POINT('',(-0.0185961207351541,-0.00553994967888425,0.0402523630820029));
#39387=CARTESIAN_POINT('',(-0.0192619352045528,-0.00234663418538221,0.0401734237368522));
#39388=CARTESIAN_POINT('',(-0.0189922425670375,0.0039786010308927,0.0400154962087426));
#39389=CARTESIAN_POINT('',(-0.0180567983964916,0.00710363801585321,0.0399365569813077));
#39390=CARTESIAN_POINT('',(-0.014808974146672,0.0125379836321928,0.0397786788714918));
#39391=CARTESIAN_POINT('',(-0.0124998034587373,0.0148419592142143,0.0396997395263325));
#39392=CARTESIAN_POINT('',(-0.00705702067722423,0.018075757329926,0.0395418119982097));
#39393=CARTESIAN_POINT('',(-0.00392920500396389,0.0190018680510246,0.0394628727707926));
#39394=CARTESIAN_POINT('',(0.00239663846866875,0.0192552037872495,0.0393049946609543));
#39395=CARTESIAN_POINT('',(0.00558844624724444,0.0185821986957283,0.0392260553158074));
#39396=CARTESIAN_POINT('',(0.0112725936445692,0.0157944033255879,0.0390681277876822));
#39397=CARTESIAN_POINT('',(0.0137586555167324,0.0136824354468426,0.0389891885602771));
#39398=CARTESIAN_POINT('',(0.0174306481390726,0.00852521285931437,0.0388313104504172));
#39399=CARTESIAN_POINT('',(0.0186129842221382,0.00548503948671966,0.0387523711052963));
#39400=CARTESIAN_POINT('',(0.0193880693395357,-0.000798317714726632,0.0385944435771406));
#39401=CARTESIAN_POINT('',(0.0189797475904416,-0.00403470231839642,0.0385155043497221));
#39402=CARTESIAN_POINT('',(0.0166706833201622,-0.00992950484529438,0.0383576262399204));
#39403=CARTESIAN_POINT('',(0.0147722286277553,-0.012582134206778,0.0382786868947513));
#39404=CARTESIAN_POINT('',(0.00993594398497793,-0.0166676801329163,0.0381207593666291));
#39405=CARTESIAN_POINT('',(0.00700322045568562,-0.0180959814502239,0.0380418201392278));
#39406=CARTESIAN_POINT('',(0.000805350935101188,-0.0193870616326328,0.0378839420293038));
#39407=CARTESIAN_POINT('',(-0.00245369774827242,-0.0192485897388964,0.0378050026846886));
#39408=CARTESIAN_POINT('',(-0.00851917681047392,-0.0174343961879857,0.0376470751559724));
#39409=CARTESIAN_POINT('',(-0.0113189505446799,-0.0157604251224328,0.0375681359284152));
#39410=CARTESIAN_POINT('',(-0.0157897129232712,-0.0112779304094601,0.0374102578225529));
#39411=CARTESIAN_POINT('',(-0.0174563193909108,-0.00847382750256133,0.0373313184476594));
#39412=CARTESIAN_POINT('',(-0.019255040384606,-0.0024037413944109,0.0371733909553239));
#39413=CARTESIAN_POINT('',(-0.0193849780691145,0.00085571010424288,0.0370944517182392));
#39414=CARTESIAN_POINT('',(-0.0180776585182107,0.0070501732653501,0.0369365734491815));
#39415=CARTESIAN_POINT('',(-0.0166417173926014,0.00997911260897645,0.0368576352931063));
#39416=CARTESIAN_POINT('',(-0.0125438251053851,0.0148049402006138,0.0366997061634564));
#39417=CARTESIAN_POINT('',(-0.00988624181041278,0.0166965076677071,0.0366207683432865));
#39418=CARTESIAN_POINT('',(-0.00398545896551984,0.018990177231314,0.0364628945348312));
#39419=CARTESIAN_POINT('',(-0.00074725003243382,0.019389251433117,0.0363839175606247));
#39420=CARTESIAN_POINT('',(0.0044859517746727,0.0187311643862688,0.0362523621408917));
#39421=CARTESIAN_POINT('',(0.00653402122317466,0.0181193042775869,0.0361998044101114));
#39422=CARTESIAN_POINT('',(0.0103271047795814,0.0162572081871673,0.0360943819838573));
#39423=CARTESIAN_POINT('',(0.0120710301301553,0.0150071588432212,0.0360416002884952));
#39424=CARTESIAN_POINT('',(0.0135547743899825,0.0135196196088883,0.0359891943217175));
#39425=CARTESIAN_POINT('',(0.0140628295261061,0.0130102650195225,0.0359712497733841));
#39426=CARTESIAN_POINT('',(0.0145708846622297,0.0125009104301567,0.0359533052250506));
#39427=CARTESIAN_POINT('',(0.0150789397983533,0.0119915558407908,0.0359353606767172));
#39428=CARTESIAN_POINT('',(0.,0.,0.034));
#39429=CARTESIAN_POINT('',(0.,0.,0.0458));
#39430=CARTESIAN_POINT('',(0.,0.,0.0442));
#39431=CARTESIAN_POINT('',(0.,0.,0.0440005108565096));
#39432=CARTESIAN_POINT('',(0.0122857142857138,0.,0.0440005108565096));
#39433=CARTESIAN_POINT('',(0.,0.,0.0458));
#39434=CARTESIAN_POINT('',(-0.0175,0.0303108891324553,-0.0157695526217005));
#39435=CARTESIAN_POINT('',(-0.0283297125253659,0.0375023651018189,0.03));
#39436=CARTESIAN_POINT('',(-0.0277718804811134,0.0383424097188667,0.03));
#39437=CARTESIAN_POINT('',(-0.0264885007929982,0.0398605778598196,0.0298963633816331));
#39438=CARTESIAN_POINT('',(-0.0240577626239275,0.0416704416785127,0.0297946825337269));
#39439=CARTESIAN_POINT('',(-0.0212962525642577,0.0428638448919929,0.0298954697823391));
#39440=CARTESIAN_POINT('',(-0.0193192917538977,0.0432223757172947,0.03));
#39441=CARTESIAN_POINT('',(-0.0183131446174913,0.0432854332797865,0.03));
#39442=CARTESIAN_POINT('',(-0.0175,0.0303108891324553,0.022));
#39443=CARTESIAN_POINT('',(-0.0305,0.0303108891324553,0.022));
#39444=CARTESIAN_POINT('',(-0.0175,0.0303108891324553,0.022));
#39445=CARTESIAN_POINT('',(0.,0.,0.0400107279868694));
#39446=CARTESIAN_POINT('',(0.,0.,0.033));
#39447=CARTESIAN_POINT('',(0.,0.,0.027));
#39448=CARTESIAN_POINT('',(0.,0.,-0.033));
#39449=CARTESIAN_POINT('',(0.,0.,-0.033));
#39450=CARTESIAN_POINT('',(-0.053,0.,-0.033));
#39451=CARTESIAN_POINT('',(4.33053857950996E-16,-0.043,0.083));
#39452=CARTESIAN_POINT('',(-0.043,1.7347234759768E-17,0.083));
#39453=CARTESIAN_POINT('',(-1.32786462810487E-16,0.043,0.083));
#39454=CARTESIAN_POINT('',(0.043,-1.7347234759768E-17,0.083));
#39455=CARTESIAN_POINT('',(0.,0.,0.));
#39456=CARTESIAN_POINT('',(-0.04368363807983,-0.0108046177216235,0.083));
#39457=CARTESIAN_POINT('',(-0.0485373756442556,-0.0120051308018038,0.083));
#39458=CARTESIAN_POINT('',(-0.04368363807983,0.0108046177216235,0.083));
#39459=CARTESIAN_POINT('',(-0.0485373756442556,0.0120051308018039,0.083));
#39460=CARTESIAN_POINT('',(0.,0.,0.));
#39461=CARTESIAN_POINT('',(0.,0.,0.));
#39462=CARTESIAN_POINT('',(-0.0129886987188641,-0.0420408263325861,0.0107004836836099));
#39463=CARTESIAN_POINT('',(0.,0.,0.081));
#39464=CARTESIAN_POINT('',(0.00350000000000027,-0.038,0.081));
#39465=CARTESIAN_POINT('',(0.00350000000000026,-0.037,0.081));
#39466=CARTESIAN_POINT('',(0.00350000000000028,-0.039,0.081));
#39467=CARTESIAN_POINT('',(0.00350000000000027,-0.039,0.081));
#39468=CARTESIAN_POINT('',(-0.00349999999999973,-0.039,0.081));
#39469=CARTESIAN_POINT('',(-0.00349999999999973,-0.038,0.081));
#39470=CARTESIAN_POINT('',(-0.00349999999999974,-0.037,0.081));
#39471=CARTESIAN_POINT('',(0.00350000000000026,-0.037,0.081));
#39472=CARTESIAN_POINT('',(0.00350000000000026,-0.037,0.0712404553740472));
#39473=CARTESIAN_POINT('',(2.393918396848E-16,-0.037,0.083));
#39474=CARTESIAN_POINT('',(0.00350000000000026,-0.037,0.083));
#39475=CARTESIAN_POINT('',(-0.00349999999999974,-0.037,0.083));
#39476=CARTESIAN_POINT('',(0.00350000000000026,-0.037,0.0712404553740472));
#39477=CARTESIAN_POINT('',(-0.00349999999999974,-0.037,0.0712404553740472));
#39478=CARTESIAN_POINT('',(0.00350000000000027,-0.039,0.0712404553740472));
#39479=CARTESIAN_POINT('',(2.74086309204335E-16,-0.039,0.083));
#39480=CARTESIAN_POINT('',(-0.00349999999999973,-0.039,0.083));
#39481=CARTESIAN_POINT('',(0.00350000000000028,-0.039,0.083));
#39482=CARTESIAN_POINT('',(-0.00349999999999972,-0.039,0.0712404553740472));
#39483=CARTESIAN_POINT('',(0.00350000000000027,-0.039,0.0712404553740472));
#39484=CARTESIAN_POINT('',(0.00350000000000027,-0.038,0.0712404553740472));
#39485=CARTESIAN_POINT('',(0.00350000000000027,-0.038,0.083));
#39486=CARTESIAN_POINT('',(0.,0.,0.081));
#39487=CARTESIAN_POINT('',(-0.0346589653438087,0.0159689110867544,0.081));
#39488=CARTESIAN_POINT('',(-0.0337929399400243,0.0154689110867544,0.081));
#39489=CARTESIAN_POINT('',(-0.0355249907475932,0.0164689110867544,0.081));
#39490=CARTESIAN_POINT('',(-0.0355249907475932,0.0164689110867544,0.081));
#39491=CARTESIAN_POINT('',(-0.0320249907475932,0.0225310889132454,0.081));
#39492=CARTESIAN_POINT('',(-0.0311589653438087,0.0220310889132454,0.081));
#39493=CARTESIAN_POINT('',(-0.0302929399400243,0.0215310889132454,0.081));
#39494=CARTESIAN_POINT('',(-0.0337929399400243,0.0154689110867544,0.081));
#39495=CARTESIAN_POINT('',(-0.0337929399400243,0.0154689110867544,0.0712404553740472));
#39496=CARTESIAN_POINT('',(-0.0320429399400243,0.0185,0.083));
#39497=CARTESIAN_POINT('',(-0.0337929399400243,0.0154689110867544,0.083));
#39498=CARTESIAN_POINT('',(-0.0302929399400243,0.0215310889132454,0.083));
#39499=CARTESIAN_POINT('',(-0.0337929399400243,0.0154689110867544,0.0712404553740472));
#39500=CARTESIAN_POINT('',(-0.0302929399400243,0.0215310889132454,0.0712404553740472));
#39501=CARTESIAN_POINT('',(-0.0355249907475932,0.0164689110867544,0.0712404553740472));
#39502=CARTESIAN_POINT('',(-0.0337749907475932,0.0195,0.083));
#39503=CARTESIAN_POINT('',(-0.0320249907475932,0.0225310889132454,0.083));
#39504=CARTESIAN_POINT('',(-0.0355249907475932,0.0164689110867544,0.083));
#39505=CARTESIAN_POINT('',(-0.0320249907475932,0.0225310889132454,0.0712404553740472));
#39506=CARTESIAN_POINT('',(-0.0355249907475932,0.0164689110867544,0.0712404553740472));
#39507=CARTESIAN_POINT('',(-0.0346589653438087,0.0159689110867544,0.0712404553740472));
#39508=CARTESIAN_POINT('',(-0.0346589653438087,0.0159689110867544,0.083));
#39509=CARTESIAN_POINT('',(0.,0.,0.081));
#39510=CARTESIAN_POINT('',(0.0311589653438087,0.0220310889132454,0.081));
#39511=CARTESIAN_POINT('',(0.0302929399400243,0.0215310889132454,0.081));
#39512=CARTESIAN_POINT('',(0.0320249907475932,0.0225310889132454,0.081));
#39513=CARTESIAN_POINT('',(0.0320249907475932,0.0225310889132454,0.081));
#39514=CARTESIAN_POINT('',(0.0355249907475932,0.0164689110867544,0.081));
#39515=CARTESIAN_POINT('',(0.0346589653438087,0.0159689110867544,0.081));
#39516=CARTESIAN_POINT('',(0.0337929399400242,0.0154689110867544,0.081));
#39517=CARTESIAN_POINT('',(0.0302929399400243,0.0215310889132454,0.081));
#39518=CARTESIAN_POINT('',(0.0302929399400243,0.0215310889132454,0.0712404553740472));
#39519=CARTESIAN_POINT('',(0.0320429399400243,0.0185,0.083));
#39520=CARTESIAN_POINT('',(0.0302929399400243,0.0215310889132454,0.083));
#39521=CARTESIAN_POINT('',(0.0337929399400242,0.0154689110867544,0.083));
#39522=CARTESIAN_POINT('',(0.0302929399400243,0.0215310889132454,0.0712404553740472));
#39523=CARTESIAN_POINT('',(0.0337929399400242,0.0154689110867544,0.0712404553740472));
#39524=CARTESIAN_POINT('',(0.0320249907475932,0.0225310889132454,0.0712404553740472));
#39525=CARTESIAN_POINT('',(0.0337749907475932,0.0195,0.083));
#39526=CARTESIAN_POINT('',(0.0355249907475932,0.0164689110867544,0.083));
#39527=CARTESIAN_POINT('',(0.0320249907475932,0.0225310889132454,0.083));
#39528=CARTESIAN_POINT('',(0.0355249907475932,0.0164689110867544,0.0712404553740472));
#39529=CARTESIAN_POINT('',(0.0320249907475932,0.0225310889132454,0.0712404553740472));
#39530=CARTESIAN_POINT('',(0.0311589653438087,0.0220310889132454,0.0712404553740472));
#39531=CARTESIAN_POINT('',(0.0311589653438087,0.0220310889132454,0.083));
#39532=CARTESIAN_POINT('',(0.,0.,0.083));
#39533=CARTESIAN_POINT('',(0.0259807621135363,-0.0149999999999982,0.083));
#39534=CARTESIAN_POINT('',(0.029980762113539,-0.0149999999999982,0.083));
#39535=CARTESIAN_POINT('',(0.,0.,0.083));
#39536=CARTESIAN_POINT('',(0.05,0.,0.083));
#39537=CARTESIAN_POINT('',(-0.02598076211353,-0.0150000000000018,0.083));
#39538=CARTESIAN_POINT('',(-0.0219807621135261,-0.0150000000000018,0.083));
#39539=CARTESIAN_POINT('',(0.,0.03,0.083));
#39540=CARTESIAN_POINT('',(0.004,0.03,0.083));
#39541=CARTESIAN_POINT('',(0.,0.,0.083));
#39542=CARTESIAN_POINT('',(0.00755,0.,0.083));
#39543=CARTESIAN_POINT('',(0.0346589653438087,0.0159689110867544,0.083));
#39544=CARTESIAN_POINT('',(-0.0311589653438087,0.0220310889132454,0.083));
#39545=CARTESIAN_POINT('',(-0.00349999999999973,-0.038,0.083));
#39546=CARTESIAN_POINT('',(-0.0175,0.0303108891324553,0.083));
#39547=CARTESIAN_POINT('',(-0.0075,0.0303108891324553,0.083));
#39548=CARTESIAN_POINT('',(0.,0.,0.084));
#39549=CARTESIAN_POINT('',(0.0259807621135363,-0.0149999999999982,0.084));
#39550=CARTESIAN_POINT('',(0.029980762113539,-0.0149999999999982,0.084));
#39551=CARTESIAN_POINT('',(0.,0.,0.084));
#39552=CARTESIAN_POINT('',(0.05,0.,0.084));
#39553=CARTESIAN_POINT('',(-0.02598076211353,-0.0150000000000018,0.084));
#39554=CARTESIAN_POINT('',(-0.0219807621135261,-0.0150000000000018,0.084));
#39555=CARTESIAN_POINT('',(0.,0.03,0.084));
#39556=CARTESIAN_POINT('',(0.004,0.03,0.084));
#39557=CARTESIAN_POINT('',(0.,0.,0.084));
#39558=CARTESIAN_POINT('',(0.00755,0.,0.084));
#39559=CARTESIAN_POINT('',(-0.0175,0.0303108891324553,0.084));
#39560=CARTESIAN_POINT('',(-0.0075,0.0303108891324553,0.084));
#39561=CARTESIAN_POINT('',(0.,0.,0.084));
#39562=CARTESIAN_POINT('',(-0.02598076211353,-0.0150000000000018,0.084));
#39563=CARTESIAN_POINT('',(0.,0.03,0.084));
#39564=CARTESIAN_POINT('',(0.,0.,0.084));
#39565=CARTESIAN_POINT('',(0.0259807621135363,-0.0149999999999982,0.084));
#39566=CARTESIAN_POINT('',(0.0346589653438087,0.0159689110867544,0.0712404553740472));
#39567=CARTESIAN_POINT('',(-0.0311589653438087,0.0220310889132454,0.0712404553740472));
#39568=CARTESIAN_POINT('',(-0.00349999999999973,-0.038,0.0712404553740472));
#39569=CARTESIAN_POINT('',(-0.0175,0.0303108891324553,0.074));
#39570=CARTESIAN_POINT('',(0.,0.,0.));
#39571=CARTESIAN_POINT('',(-0.00598201094464286,0.0522062499024776,0.0466759019477942));
#39572=CARTESIAN_POINT('',(-0.00598201094464285,0.0521155356167633,0.0447322287687989));
#39573=CARTESIAN_POINT('',(-0.004839548514753,0.052024821331049,0.0431597641354809));
#39574=CARTESIAN_POINT('',(-0.00369708608486315,0.0519341070453347,0.041587299502163));
#39575=CARTESIAN_POINT('',(-0.00184854304243157,0.0518433927596204,0.0409866714583427));
#39576=CARTESIAN_POINT('',(-3.8514275599305E-19,0.0517526784739062,0.0403860434145223));
#39577=CARTESIAN_POINT('',(0.00184854304243157,0.0516619641881919,0.0409866714583427));
#39578=CARTESIAN_POINT('',(0.00369708608486315,0.0515712499024776,0.041587299502163));
#39579=CARTESIAN_POINT('',(0.004839548514753,0.0514805356167633,0.0431597641354809));
#39580=CARTESIAN_POINT('',(0.00598201094464285,0.0513898213310489,0.0447322287687989));
#39581=CARTESIAN_POINT('',(0.00598201094464286,0.0512991070453347,0.0466759019477942));
#39582=CARTESIAN_POINT('',(0.00598201094464286,0.0512083927596204,0.0486195751267895));
#39583=CARTESIAN_POINT('',(0.004839548514753,0.0511176784739062,0.0501920397601074));
#39584=CARTESIAN_POINT('',(0.00369708608486315,0.0510269641881918,0.0517645043934253));
#39585=CARTESIAN_POINT('',(0.00184854304243157,0.0509362499024776,0.0523651324372457));
#39586=CARTESIAN_POINT('',(1.15542826797915E-18,0.0508455356167633,0.052965760481066));
#39587=CARTESIAN_POINT('',(-0.00184854304243157,0.050754821331049,0.0523651324372457));
#39588=CARTESIAN_POINT('',(-0.00369708608486315,0.0506641070453347,0.0517645043934253));
#39589=CARTESIAN_POINT('',(-0.004839548514753,0.0505733927596204,0.0501920397601074));
#39590=CARTESIAN_POINT('',(-0.00598201094464285,0.0504826784739061,0.0486195751267895));
#39591=CARTESIAN_POINT('',(-0.00598201094464286,0.0503919641881919,0.0466759019477942));
#39592=CARTESIAN_POINT('',(-0.00598201094464285,0.0503012499024776,0.0447322287687989));
#39593=CARTESIAN_POINT('',(-0.004839548514753,0.0502105356167633,0.0431597641354809));
#39594=CARTESIAN_POINT('',(-0.00369708608486315,0.050119821331049,0.041587299502163));
#39595=CARTESIAN_POINT('',(-0.00184854304243157,0.0500291070453347,0.0409866714583427));
#39596=CARTESIAN_POINT('',(-3.8514275599305E-19,0.0499383927596204,0.0403860434145223));
#39597=CARTESIAN_POINT('',(0.00184854304243157,0.0498476784739062,0.0409866714583427));
#39598=CARTESIAN_POINT('',(0.00369708608486315,0.0497569641881919,0.041587299502163));
#39599=CARTESIAN_POINT('',(0.004839548514753,0.0496662499024776,0.0431597641354809));
#39600=CARTESIAN_POINT('',(0.00598201094464285,0.0495755356167633,0.0447322287687989));
#39601=CARTESIAN_POINT('',(0.00598201094464286,0.049484821331049,0.0466759019477942));
#39602=CARTESIAN_POINT('',(0.00598201094464286,0.0493941070453347,0.0486195751267895));
#39603=CARTESIAN_POINT('',(0.004839548514753,0.0493033927596204,0.0501920397601074));
#39604=CARTESIAN_POINT('',(0.00369708608486315,0.0492126784739062,0.0517645043934253));
#39605=CARTESIAN_POINT('',(0.00184854304243157,0.0491219641881919,0.0523651324372457));
#39606=CARTESIAN_POINT('',(1.15542826797915E-18,0.0490312499024775,0.052965760481066));
#39607=CARTESIAN_POINT('',(-0.00184854304243157,0.0489405356167633,0.0523651324372457));
#39608=CARTESIAN_POINT('',(-0.00369708608486315,0.048849821331049,0.0517645043934253));
#39609=CARTESIAN_POINT('',(-0.004839548514753,0.0487591070453347,0.0501920397601074));
#39610=CARTESIAN_POINT('',(-0.00598201094464285,0.0486683927596204,0.0486195751267895));
#39611=CARTESIAN_POINT('',(-0.00598201094464286,0.0485776784739062,0.0466759019477942));
#39612=CARTESIAN_POINT('',(-0.00598201094464285,0.0484869641881918,0.0447322287687989));
#39613=CARTESIAN_POINT('',(-0.004839548514753,0.0483962499024776,0.0431597641354809));
#39614=CARTESIAN_POINT('',(-0.00369708608486315,0.0483055356167633,0.041587299502163));
#39615=CARTESIAN_POINT('',(-0.00184854304243157,0.048214821331049,0.0409866714583427));
#39616=CARTESIAN_POINT('',(-3.8514275599305E-19,0.0481241070453347,0.0403860434145223));
#39617=CARTESIAN_POINT('',(0.00184854304243157,0.0480333927596204,0.0409866714583427));
#39618=CARTESIAN_POINT('',(0.00369708608486315,0.0479426784739061,0.041587299502163));
#39619=CARTESIAN_POINT('',(0.004839548514753,0.0478519641881919,0.0431597641354809));
#39620=CARTESIAN_POINT('',(0.00598201094464285,0.0477612499024776,0.0447322287687989));
#39621=CARTESIAN_POINT('',(0.00598201094464286,0.0476705356167633,0.0466759019477942));
#39622=CARTESIAN_POINT('',(0.00598201094464286,0.047579821331049,0.0486195751267895));
#39623=CARTESIAN_POINT('',(0.004839548514753,0.0474891070453347,0.0501920397601074));
#39624=CARTESIAN_POINT('',(0.00369708608486315,0.0473983927596204,0.0517645043934253));
#39625=CARTESIAN_POINT('',(0.00184854304243157,0.0473076784739062,0.0523651324372457));
#39626=CARTESIAN_POINT('',(1.15542826797915E-18,0.0472169641881919,0.052965760481066));
#39627=CARTESIAN_POINT('',(-0.00184854304243157,0.0471262499024776,0.0523651324372457));
#39628=CARTESIAN_POINT('',(-0.00369708608486315,0.0470355356167633,0.0517645043934253));
#39629=CARTESIAN_POINT('',(-0.004839548514753,0.046944821331049,0.0501920397601074));
#39630=CARTESIAN_POINT('',(-0.00598201094464285,0.0468541070453347,0.0486195751267895));
#39631=CARTESIAN_POINT('',(-0.00598201094464286,0.0467633927596204,0.0466759019477942));
#39632=CARTESIAN_POINT('',(-0.00598201094464285,0.0466726784739061,0.0447322287687989));
#39633=CARTESIAN_POINT('',(-0.004839548514753,0.0465819641881919,0.0431597641354809));
#39634=CARTESIAN_POINT('',(-0.00369708608486315,0.0464912499024775,0.041587299502163));
#39635=CARTESIAN_POINT('',(-0.00184854304243157,0.0464005356167633,0.0409866714583427));
#39636=CARTESIAN_POINT('',(-3.8514275599305E-19,0.046309821331049,0.0403860434145223));
#39637=CARTESIAN_POINT('',(0.00184854304243157,0.0462191070453347,0.0409866714583427));
#39638=CARTESIAN_POINT('',(0.00369708608486315,0.0461283927596204,0.041587299502163));
#39639=CARTESIAN_POINT('',(0.004839548514753,0.0460376784739062,0.0431597641354809));
#39640=CARTESIAN_POINT('',(0.00598201094464285,0.0459469641881919,0.0447322287687989));
#39641=CARTESIAN_POINT('',(0.00598201094464286,0.0458562499024776,0.0466759019477942));
#39642=CARTESIAN_POINT('',(0.00598201094464286,0.0457655356167633,0.0486195751267895));
#39643=CARTESIAN_POINT('',(0.004839548514753,0.045674821331049,0.0501920397601074));
#39644=CARTESIAN_POINT('',(0.00369708608486315,0.0455841070453347,0.0517645043934253));
#39645=CARTESIAN_POINT('',(0.00184854304243157,0.0454933927596204,0.0523651324372457));
#39646=CARTESIAN_POINT('',(1.15542826797915E-18,0.0454026784739061,0.052965760481066));
#39647=CARTESIAN_POINT('',(-0.00184854304243157,0.0453119641881919,0.0523651324372457));
#39648=CARTESIAN_POINT('',(-0.00290176072609688,0.0452602792191745,0.052022921267402));
#39649=CARTESIAN_POINT('',(-0.00376267526235443,0.0452060077307469,0.0513263567440365));
#39650=CARTESIAN_POINT('',(-0.005,0.0516392856192409,0.0466759019477942));
#39651=CARTESIAN_POINT('',(-0.005,0.0515485713335265,0.0450513034666296));
#39652=CARTESIAN_POINT('',(-0.00404508497187473,0.0514578570478123,0.0437369756863318));
#39653=CARTESIAN_POINT('',(-0.00309016994374947,0.0513671427620979,0.042422647906034));
#39654=CARTESIAN_POINT('',(-0.00154508497187473,0.0512764284763837,0.0419206193663185));
#39655=CARTESIAN_POINT('',(-3.21917461834437E-19,0.0511857141906694,0.0414185908266028));
#39656=CARTESIAN_POINT('',(0.00154508497187473,0.0510949999049552,0.0419206193663185));
#39657=CARTESIAN_POINT('',(0.00309016994374947,0.0510042856192408,0.042422647906034));
#39658=CARTESIAN_POINT('',(0.00404508497187473,0.0509135713335266,0.0437369756863318));
#39659=CARTESIAN_POINT('',(0.005,0.0508228570478123,0.0450513034666296));
#39660=CARTESIAN_POINT('',(0.005,0.050732142762098,0.0466759019477942));
#39661=CARTESIAN_POINT('',(0.005,0.0506414284763837,0.0483005004289586));
#39662=CARTESIAN_POINT('',(0.00404508497187473,0.0505507141906694,0.0496148282092566));
#39663=CARTESIAN_POINT('',(0.00309016994374947,0.0504599999049551,0.0509291559895544));
#39664=CARTESIAN_POINT('',(0.00154508497187473,0.0503692856192409,0.05143118452927));
#39665=CARTESIAN_POINT('',(9.65752385503311E-19,0.0502785713335266,0.0519332130689855));
#39666=CARTESIAN_POINT('',(-0.00154508497187473,0.0501878570478123,0.05143118452927));
#39667=CARTESIAN_POINT('',(-0.00309016994374947,0.050097142762098,0.0509291559895544));
#39668=CARTESIAN_POINT('',(-0.00404508497187473,0.0500064284763837,0.0496148282092566));
#39669=CARTESIAN_POINT('',(-0.005,0.0499157141906694,0.0483005004289586));
#39670=CARTESIAN_POINT('',(-0.005,0.0498249999049552,0.0466759019477942));
#39671=CARTESIAN_POINT('',(-0.005,0.0497342856192409,0.0450513034666296));
#39672=CARTESIAN_POINT('',(-0.00404508497187473,0.0496435713335266,0.0437369756863318));
#39673=CARTESIAN_POINT('',(-0.00309016994374947,0.0495528570478123,0.042422647906034));
#39674=CARTESIAN_POINT('',(-0.00154508497187473,0.049462142762098,0.0419206193663185));
#39675=CARTESIAN_POINT('',(-3.21917461834437E-19,0.0493714284763836,0.0414185908266028));
#39676=CARTESIAN_POINT('',(0.00154508497187473,0.0492807141906694,0.0419206193663185));
#39677=CARTESIAN_POINT('',(0.00309016994374947,0.0491899999049551,0.042422647906034));
#39678=CARTESIAN_POINT('',(0.00404508497187473,0.0490992856192409,0.0437369756863318));
#39679=CARTESIAN_POINT('',(0.005,0.0490085713335265,0.0450513034666296));
#39680=CARTESIAN_POINT('',(0.005,0.0489178570478123,0.0466759019477942));
#39681=CARTESIAN_POINT('',(0.005,0.048827142762098,0.0483005004289586));
#39682=CARTESIAN_POINT('',(0.00404508497187473,0.0487364284763837,0.0496148282092566));
#39683=CARTESIAN_POINT('',(0.00309016994374947,0.0486457141906694,0.0509291559895544));
#39684=CARTESIAN_POINT('',(0.00154508497187473,0.0485549999049552,0.05143118452927));
#39685=CARTESIAN_POINT('',(9.65752385503311E-19,0.0484642856192408,0.0519332130689855));
#39686=CARTESIAN_POINT('',(-0.00154508497187473,0.0483735713335266,0.05143118452927));
#39687=CARTESIAN_POINT('',(-0.00309016994374947,0.0482828570478123,0.0509291559895544));
#39688=CARTESIAN_POINT('',(-0.00404508497187473,0.048192142762098,0.0496148282092566));
#39689=CARTESIAN_POINT('',(-0.005,0.0481014284763837,0.0483005004289586));
#39690=CARTESIAN_POINT('',(-0.005,0.0480107141906694,0.0466759019477942));
#39691=CARTESIAN_POINT('',(-0.005,0.0479199999049551,0.0450513034666296));
#39692=CARTESIAN_POINT('',(-0.00404508497187473,0.0478292856192409,0.0437369756863318));
#39693=CARTESIAN_POINT('',(-0.00309016994374947,0.0477385713335266,0.042422647906034));
#39694=CARTESIAN_POINT('',(-0.00154508497187473,0.0476478570478123,0.0419206193663185));
#39695=CARTESIAN_POINT('',(-3.21917461834437E-19,0.047557142762098,0.0414185908266028));
#39696=CARTESIAN_POINT('',(0.00154508497187473,0.0474664284763837,0.0419206193663185));
#39697=CARTESIAN_POINT('',(0.00309016994374947,0.0473757141906694,0.042422647906034));
#39698=CARTESIAN_POINT('',(0.00404508497187473,0.0472849999049552,0.0437369756863318));
#39699=CARTESIAN_POINT('',(0.005,0.0471942856192409,0.0450513034666296));
#39700=CARTESIAN_POINT('',(0.005,0.0471035713335266,0.0466759019477942));
#39701=CARTESIAN_POINT('',(0.005,0.0470128570478123,0.0483005004289586));
#39702=CARTESIAN_POINT('',(0.00404508497187473,0.046922142762098,0.0496148282092566));
#39703=CARTESIAN_POINT('',(0.00309016994374947,0.0468314284763837,0.0509291559895544));
#39704=CARTESIAN_POINT('',(0.00154508497187473,0.0467407141906694,0.05143118452927));
#39705=CARTESIAN_POINT('',(9.65752385503311E-19,0.0466499999049551,0.0519332130689855));
#39706=CARTESIAN_POINT('',(-0.00154508497187473,0.0465592856192409,0.05143118452927));
#39707=CARTESIAN_POINT('',(-0.00309016994374947,0.0464685713335266,0.0509291559895544));
#39708=CARTESIAN_POINT('',(-0.00404508497187473,0.0463778570478123,0.0496148282092566));
#39709=CARTESIAN_POINT('',(-0.005,0.046287142762098,0.0483005004289586));
#39710=CARTESIAN_POINT('',(-0.005,0.0461964284763837,0.0466759019477942));
#39711=CARTESIAN_POINT('',(-0.005,0.0461057141906694,0.0450513034666296));
#39712=CARTESIAN_POINT('',(-0.00404508497187473,0.0460149999049552,0.0437369756863318));
#39713=CARTESIAN_POINT('',(-0.00309016994374947,0.0459242856192409,0.042422647906034));
#39714=CARTESIAN_POINT('',(-0.00154508497187473,0.0458335713335266,0.0419206193663185));
#39715=CARTESIAN_POINT('',(-3.21917461834437E-19,0.0457428570478123,0.0414185908266028));
#39716=CARTESIAN_POINT('',(0.00154508497187473,0.045652142762098,0.0419206193663185));
#39717=CARTESIAN_POINT('',(0.00309016994374947,0.0455614284763837,0.042422647906034));
#39718=CARTESIAN_POINT('',(0.00404508497187473,0.0454707141906694,0.0437369756863318));
#39719=CARTESIAN_POINT('',(0.005,0.0453799999049551,0.0450513034666296));
#39720=CARTESIAN_POINT('',(0.005,0.0452892856192409,0.0466759019477942));
#39721=CARTESIAN_POINT('',(0.005,0.0451985713335266,0.0483005004289586));
#39722=CARTESIAN_POINT('',(0.00404508497187473,0.0451078570478123,0.0496148282092566));
#39723=CARTESIAN_POINT('',(0.00309016994374947,0.045017142762098,0.0509291559895544));
#39724=CARTESIAN_POINT('',(0.00154508497187473,0.0449264284763837,0.05143118452927));
#39725=CARTESIAN_POINT('',(9.65752385503311E-19,0.0448357141906694,0.0519332130689855));
#39726=CARTESIAN_POINT('',(-0.00154508497187473,0.0447449999049551,0.05143118452927));
#39727=CARTESIAN_POINT('',(-0.00242540573140837,0.0446933149359378,0.0511451509754948));
#39728=CARTESIAN_POINT('',(-0.0031449919576995,0.0446390434475102,0.0505629349533147));
#39729=CARTESIAN_POINT('',(-0.00549100547232143,0.0519227677608592,0.0466759019477942));
#39730=CARTESIAN_POINT('',(-0.00598201094464286,0.0522062499024776,0.0466759019477942));
#39731=CARTESIAN_POINT('',(-0.005,0.0516392856192409,0.0466759019477942));
#39732=CARTESIAN_POINT('',(-0.00598201094464286,0.0522062499024776,0.0466759019477942));
#39733=CARTESIAN_POINT('',(-0.00598201094464285,0.0521155356167633,0.0447322287687989));
#39734=CARTESIAN_POINT('',(-0.004839548514753,0.052024821331049,0.0431597641354809));
#39735=CARTESIAN_POINT('',(-0.00369708608486315,0.0519341070453347,0.041587299502163));
#39736=CARTESIAN_POINT('',(-0.00184854304243157,0.0518433927596204,0.0409866714583427));
#39737=CARTESIAN_POINT('',(-3.8514275599305E-19,0.0517526784739062,0.0403860434145223));
#39738=CARTESIAN_POINT('',(0.00184854304243157,0.0516619641881919,0.0409866714583427));
#39739=CARTESIAN_POINT('',(0.00369708608486315,0.0515712499024776,0.041587299502163));
#39740=CARTESIAN_POINT('',(0.004839548514753,0.0514805356167633,0.0431597641354809));
#39741=CARTESIAN_POINT('',(0.00598201094464285,0.0513898213310489,0.0447322287687989));
#39742=CARTESIAN_POINT('',(0.00598201094464286,0.0512991070453347,0.0466759019477942));
#39743=CARTESIAN_POINT('',(0.00598201094464286,0.0512083927596204,0.0486195751267895));
#39744=CARTESIAN_POINT('',(0.004839548514753,0.0511176784739062,0.0501920397601074));
#39745=CARTESIAN_POINT('',(0.00369708608486315,0.0510269641881918,0.0517645043934253));
#39746=CARTESIAN_POINT('',(0.00184854304243157,0.0509362499024776,0.0523651324372457));
#39747=CARTESIAN_POINT('',(1.15542826797915E-18,0.0508455356167633,0.052965760481066));
#39748=CARTESIAN_POINT('',(-0.00184854304243157,0.050754821331049,0.0523651324372457));
#39749=CARTESIAN_POINT('',(-0.00369708608486315,0.0506641070453347,0.0517645043934253));
#39750=CARTESIAN_POINT('',(-0.004839548514753,0.0505733927596204,0.0501920397601074));
#39751=CARTESIAN_POINT('',(-0.00598201094464285,0.0504826784739061,0.0486195751267895));
#39752=CARTESIAN_POINT('',(-0.00598201094464286,0.0503919641881919,0.0466759019477942));
#39753=CARTESIAN_POINT('',(-0.00598201094464285,0.0503012499024776,0.0447322287687989));
#39754=CARTESIAN_POINT('',(-0.004839548514753,0.0502105356167633,0.0431597641354809));
#39755=CARTESIAN_POINT('',(-0.00369708608486315,0.050119821331049,0.041587299502163));
#39756=CARTESIAN_POINT('',(-0.00184854304243157,0.0500291070453347,0.0409866714583427));
#39757=CARTESIAN_POINT('',(-3.8514275599305E-19,0.0499383927596204,0.0403860434145223));
#39758=CARTESIAN_POINT('',(0.00184854304243157,0.0498476784739062,0.0409866714583427));
#39759=CARTESIAN_POINT('',(0.00369708608486315,0.0497569641881919,0.041587299502163));
#39760=CARTESIAN_POINT('',(0.004839548514753,0.0496662499024776,0.0431597641354809));
#39761=CARTESIAN_POINT('',(0.00598201094464285,0.0495755356167633,0.0447322287687989));
#39762=CARTESIAN_POINT('',(0.00598201094464286,0.049484821331049,0.0466759019477942));
#39763=CARTESIAN_POINT('',(0.00598201094464286,0.0493941070453347,0.0486195751267895));
#39764=CARTESIAN_POINT('',(0.004839548514753,0.0493033927596204,0.0501920397601074));
#39765=CARTESIAN_POINT('',(0.00369708608486315,0.0492126784739062,0.0517645043934253));
#39766=CARTESIAN_POINT('',(0.00184854304243157,0.0491219641881919,0.0523651324372457));
#39767=CARTESIAN_POINT('',(1.15542826797915E-18,0.0490312499024775,0.052965760481066));
#39768=CARTESIAN_POINT('',(-0.00184854304243157,0.0489405356167633,0.0523651324372457));
#39769=CARTESIAN_POINT('',(-0.00369708608486315,0.0488498213310489,0.0517645043934253));
#39770=CARTESIAN_POINT('',(-0.004839548514753,0.0487591070453347,0.0501920397601074));
#39771=CARTESIAN_POINT('',(-0.00598201094464285,0.0486683927596204,0.0486195751267895));
#39772=CARTESIAN_POINT('',(-0.00598201094464286,0.0485776784739062,0.0466759019477942));
#39773=CARTESIAN_POINT('',(-0.00598201094464285,0.0484869641881918,0.0447322287687989));
#39774=CARTESIAN_POINT('',(-0.004839548514753,0.0483962499024776,0.0431597641354809));
#39775=CARTESIAN_POINT('',(-0.00369708608486315,0.0483055356167633,0.041587299502163));
#39776=CARTESIAN_POINT('',(-0.00184854304243157,0.048214821331049,0.0409866714583427));
#39777=CARTESIAN_POINT('',(-3.8514275599305E-19,0.0481241070453347,0.0403860434145223));
#39778=CARTESIAN_POINT('',(0.00184854304243157,0.0480333927596204,0.0409866714583427));
#39779=CARTESIAN_POINT('',(0.00369708608486315,0.0479426784739061,0.041587299502163));
#39780=CARTESIAN_POINT('',(0.004839548514753,0.0478519641881919,0.0431597641354809));
#39781=CARTESIAN_POINT('',(0.00598201094464285,0.0477612499024776,0.0447322287687989));
#39782=CARTESIAN_POINT('',(0.00598201094464286,0.0476705356167633,0.0466759019477942));
#39783=CARTESIAN_POINT('',(0.00598201094464286,0.047579821331049,0.0486195751267895));
#39784=CARTESIAN_POINT('',(0.004839548514753,0.0474891070453347,0.0501920397601074));
#39785=CARTESIAN_POINT('',(0.00369708608486315,0.0473983927596204,0.0517645043934253));
#39786=CARTESIAN_POINT('',(0.00184854304243157,0.0473076784739062,0.0523651324372457));
#39787=CARTESIAN_POINT('',(1.15542826797915E-18,0.0472169641881919,0.052965760481066));
#39788=CARTESIAN_POINT('',(-0.00184854304243157,0.0471262499024776,0.0523651324372457));
#39789=CARTESIAN_POINT('',(-0.00369708608486315,0.0470355356167633,0.0517645043934253));
#39790=CARTESIAN_POINT('',(-0.004839548514753,0.046944821331049,0.0501920397601074));
#39791=CARTESIAN_POINT('',(-0.00598201094464285,0.0468541070453347,0.0486195751267895));
#39792=CARTESIAN_POINT('',(-0.00598201094464286,0.0467633927596204,0.0466759019477942));
#39793=CARTESIAN_POINT('',(-0.00598201094464285,0.0466726784739061,0.0447322287687989));
#39794=CARTESIAN_POINT('',(-0.004839548514753,0.0465819641881919,0.0431597641354809));
#39795=CARTESIAN_POINT('',(-0.00369708608486315,0.0464912499024775,0.041587299502163));
#39796=CARTESIAN_POINT('',(-0.00184854304243157,0.0464005356167633,0.0409866714583427));
#39797=CARTESIAN_POINT('',(-3.8514275599305E-19,0.046309821331049,0.0403860434145223));
#39798=CARTESIAN_POINT('',(0.00184854304243157,0.0462191070453347,0.0409866714583427));
#39799=CARTESIAN_POINT('',(0.00369708608486315,0.0461283927596204,0.041587299502163));
#39800=CARTESIAN_POINT('',(0.004839548514753,0.0460376784739062,0.0431597641354809));
#39801=CARTESIAN_POINT('',(0.00598201094464285,0.0459469641881919,0.0447322287687989));
#39802=CARTESIAN_POINT('',(0.00598201094464286,0.0458562499024776,0.0466759019477942));
#39803=CARTESIAN_POINT('',(0.00598201094464286,0.0457655356167633,0.0486195751267895));
#39804=CARTESIAN_POINT('',(0.004839548514753,0.045674821331049,0.0501920397601074));
#39805=CARTESIAN_POINT('',(0.00369708608486315,0.0455841070453347,0.0517645043934253));
#39806=CARTESIAN_POINT('',(0.00184854304243157,0.0454933927596204,0.0523651324372457));
#39807=CARTESIAN_POINT('',(1.15542826797915E-18,0.0454026784739061,0.052965760481066));
#39808=CARTESIAN_POINT('',(-0.00184854304243157,0.0453119641881919,0.0523651324372457));
#39809=CARTESIAN_POINT('',(-0.00290176072609409,0.0452602792191746,0.052022921267403));
#39810=CARTESIAN_POINT('',(-0.00376267526235003,0.0452060077307472,0.05132635674404));
#39811=CARTESIAN_POINT('',(-0.00376267526235003,0.0452060077307471,0.0513263567440401));
#39812=CARTESIAN_POINT('',(-0.00345383361002476,0.0449225255891286,0.0509446458486774));
#39813=CARTESIAN_POINT('',(-0.0031449919576995,0.0446390434475102,0.0505629349533147));
#39814=CARTESIAN_POINT('',(8.89120054436383E-19,0.0448357141906694,0.0516759019477941));
#39815=CARTESIAN_POINT('',(-0.00079192220162268,0.0447892192352662,0.0516759019477941));
#39816=CARTESIAN_POINT('',(-0.00154508497187473,0.0447449999049551,0.05143118452927));
#39817=CARTESIAN_POINT('',(-0.00242540573140837,0.0446933149359378,0.0511451509754948));
#39818=CARTESIAN_POINT('',(-0.0031449919576995,0.0446390434475102,0.0505629349533147));
#39819=CARTESIAN_POINT('',(8.89120054436383E-19,0.0448357141906695,0.0516759019477942));
#39820=CARTESIAN_POINT('',(-2.22280013609096E-19,0.0457428570478123,0.0416759019477942));
#39821=CARTESIAN_POINT('',(0.000791922201622681,0.0456963620924091,0.0416759019477942));
#39822=CARTESIAN_POINT('',(0.00154508497187473,0.045652142762098,0.0419206193663185));
#39823=CARTESIAN_POINT('',(0.00309016994374947,0.0455614284763837,0.042422647906034));
#39824=CARTESIAN_POINT('',(0.00404508497187473,0.0454707141906694,0.0437369756863318));
#39825=CARTESIAN_POINT('',(0.005,0.0453799999049551,0.0450513034666297));
#39826=CARTESIAN_POINT('',(0.005,0.0452892856192409,0.0466759019477942));
#39827=CARTESIAN_POINT('',(0.005,0.0451985713335266,0.0483005004289586));
#39828=CARTESIAN_POINT('',(0.00404508497187473,0.0451078570478123,0.0496148282092566));
#39829=CARTESIAN_POINT('',(0.00309016994374947,0.045017142762098,0.0509291559895544));
#39830=CARTESIAN_POINT('',(0.00154508497187473,0.0449264284763837,0.05143118452927));
#39831=CARTESIAN_POINT('',(0.000791922201622682,0.0448822091460727,0.0516759019477941));
#39832=CARTESIAN_POINT('',(8.89120054436383E-19,0.0448357141906694,0.0516759019477941));
#39833=CARTESIAN_POINT('',(-2.22280013609096E-19,0.0457428570478123,0.0416759019477942));
#39834=CARTESIAN_POINT('',(8.89120054436383E-19,0.0466499999049551,0.0516759019477941));
#39835=CARTESIAN_POINT('',(-0.00079192220162268,0.046603504949552,0.0516759019477941));
#39836=CARTESIAN_POINT('',(-0.00154508497187473,0.0465592856192409,0.05143118452927));
#39837=CARTESIAN_POINT('',(-0.00309016994374947,0.0464685713335266,0.0509291559895544));
#39838=CARTESIAN_POINT('',(-0.00404508497187473,0.0463778570478123,0.0496148282092566));
#39839=CARTESIAN_POINT('',(-0.005,0.046287142762098,0.0483005004289586));
#39840=CARTESIAN_POINT('',(-0.005,0.0461964284763837,0.0466759019477942));
#39841=CARTESIAN_POINT('',(-0.005,0.0461057141906694,0.0450513034666297));
#39842=CARTESIAN_POINT('',(-0.00404508497187473,0.0460149999049552,0.0437369756863318));
#39843=CARTESIAN_POINT('',(-0.00309016994374947,0.0459242856192409,0.042422647906034));
#39844=CARTESIAN_POINT('',(-0.00154508497187473,0.0458335713335266,0.0419206193663185));
#39845=CARTESIAN_POINT('',(-0.000791922201622681,0.0457893520032155,0.0416759019477942));
#39846=CARTESIAN_POINT('',(-2.22280013609096E-19,0.0457428570478123,0.0416759019477942));
#39847=CARTESIAN_POINT('',(8.89120054436383E-19,0.0466499999049552,0.0516759019477942));
#39848=CARTESIAN_POINT('',(-2.22280013609096E-19,0.047557142762098,0.0416759019477942));
#39849=CARTESIAN_POINT('',(0.000791922201622681,0.0475106478066948,0.0416759019477942));
#39850=CARTESIAN_POINT('',(0.00154508497187473,0.0474664284763837,0.0419206193663185));
#39851=CARTESIAN_POINT('',(0.00309016994374947,0.0473757141906694,0.042422647906034));
#39852=CARTESIAN_POINT('',(0.00404508497187473,0.0472849999049552,0.0437369756863318));
#39853=CARTESIAN_POINT('',(0.005,0.0471942856192409,0.0450513034666297));
#39854=CARTESIAN_POINT('',(0.005,0.0471035713335266,0.0466759019477942));
#39855=CARTESIAN_POINT('',(0.005,0.0470128570478123,0.0483005004289586));
#39856=CARTESIAN_POINT('',(0.00404508497187473,0.046922142762098,0.0496148282092566));
#39857=CARTESIAN_POINT('',(0.00309016994374947,0.0468314284763837,0.0509291559895544));
#39858=CARTESIAN_POINT('',(0.00154508497187473,0.0467407141906694,0.05143118452927));
#39859=CARTESIAN_POINT('',(0.000791922201622682,0.0466964948603584,0.0516759019477941));
#39860=CARTESIAN_POINT('',(8.89120054436383E-19,0.0466499999049551,0.0516759019477941));
#39861=CARTESIAN_POINT('',(-2.22280013609096E-19,0.047557142762098,0.0416759019477942));
#39862=CARTESIAN_POINT('',(8.89120054436383E-19,0.0484642856192409,0.0516759019477941));
#39863=CARTESIAN_POINT('',(-0.00079192220162268,0.0484177906638377,0.0516759019477941));
#39864=CARTESIAN_POINT('',(-0.00154508497187473,0.0483735713335266,0.05143118452927));
#39865=CARTESIAN_POINT('',(-0.00309016994374947,0.0482828570478123,0.0509291559895544));
#39866=CARTESIAN_POINT('',(-0.00404508497187473,0.048192142762098,0.0496148282092566));
#39867=CARTESIAN_POINT('',(-0.005,0.0481014284763837,0.0483005004289586));
#39868=CARTESIAN_POINT('',(-0.005,0.0480107141906694,0.0466759019477942));
#39869=CARTESIAN_POINT('',(-0.005,0.0479199999049551,0.0450513034666297));
#39870=CARTESIAN_POINT('',(-0.00404508497187473,0.0478292856192409,0.0437369756863318));
#39871=CARTESIAN_POINT('',(-0.00309016994374947,0.0477385713335266,0.042422647906034));
#39872=CARTESIAN_POINT('',(-0.00154508497187473,0.0476478570478123,0.0419206193663185));
#39873=CARTESIAN_POINT('',(-0.000791922201622681,0.0476036377175013,0.0416759019477942));
#39874=CARTESIAN_POINT('',(-2.22280013609096E-19,0.047557142762098,0.0416759019477942));
#39875=CARTESIAN_POINT('',(8.89120054436383E-19,0.0484642856192409,0.0516759019477942));
#39876=CARTESIAN_POINT('',(-2.22280013609096E-19,0.0493714284763837,0.0416759019477942));
#39877=CARTESIAN_POINT('',(0.000791922201622681,0.0493249335209805,0.0416759019477942));
#39878=CARTESIAN_POINT('',(0.00154508497187473,0.0492807141906694,0.0419206193663185));
#39879=CARTESIAN_POINT('',(0.00309016994374947,0.0491899999049551,0.042422647906034));
#39880=CARTESIAN_POINT('',(0.00404508497187473,0.0490992856192409,0.0437369756863318));
#39881=CARTESIAN_POINT('',(0.005,0.0490085713335265,0.0450513034666297));
#39882=CARTESIAN_POINT('',(0.005,0.0489178570478123,0.0466759019477942));
#39883=CARTESIAN_POINT('',(0.005,0.048827142762098,0.0483005004289586));
#39884=CARTESIAN_POINT('',(0.00404508497187473,0.0487364284763837,0.0496148282092566));
#39885=CARTESIAN_POINT('',(0.00309016994374947,0.0486457141906694,0.0509291559895544));
#39886=CARTESIAN_POINT('',(0.00154508497187473,0.0485549999049552,0.05143118452927));
#39887=CARTESIAN_POINT('',(0.000791922201622682,0.0485107805746441,0.0516759019477941));
#39888=CARTESIAN_POINT('',(8.89120054436383E-19,0.0484642856192409,0.0516759019477941));
#39889=CARTESIAN_POINT('',(-2.22280013609096E-19,0.0493714284763837,0.0416759019477942));
#39890=CARTESIAN_POINT('',(8.89120054436383E-19,0.0502785713335266,0.0516759019477941));
#39891=CARTESIAN_POINT('',(-0.00079192220162268,0.0502320763781233,0.0516759019477941));
#39892=CARTESIAN_POINT('',(-0.00154508497187473,0.0501878570478123,0.05143118452927));
#39893=CARTESIAN_POINT('',(-0.00309016994374947,0.050097142762098,0.0509291559895544));
#39894=CARTESIAN_POINT('',(-0.00404508497187473,0.0500064284763837,0.0496148282092566));
#39895=CARTESIAN_POINT('',(-0.005,0.0499157141906694,0.0483005004289586));
#39896=CARTESIAN_POINT('',(-0.005,0.0498249999049552,0.0466759019477942));
#39897=CARTESIAN_POINT('',(-0.005,0.0497342856192409,0.0450513034666297));
#39898=CARTESIAN_POINT('',(-0.00404508497187473,0.0496435713335266,0.0437369756863318));
#39899=CARTESIAN_POINT('',(-0.00309016994374947,0.0495528570478123,0.042422647906034));
#39900=CARTESIAN_POINT('',(-0.00154508497187473,0.049462142762098,0.0419206193663185));
#39901=CARTESIAN_POINT('',(-0.000791922201622681,0.0494179234317869,0.0416759019477942));
#39902=CARTESIAN_POINT('',(-2.22280013609096E-19,0.0493714284763837,0.0416759019477942));
#39903=CARTESIAN_POINT('',(8.89120054436383E-19,0.0502785713335266,0.0516759019477942));
#39904=CARTESIAN_POINT('',(-2.22280013609096E-19,0.0511857141906695,0.0416759019477942));
#39905=CARTESIAN_POINT('',(0.000791922201622681,0.0511392192352662,0.0416759019477942));
#39906=CARTESIAN_POINT('',(0.00154508497187473,0.0510949999049552,0.0419206193663185));
#39907=CARTESIAN_POINT('',(0.00309016994374947,0.0510042856192408,0.042422647906034));
#39908=CARTESIAN_POINT('',(0.00404508497187473,0.0509135713335266,0.0437369756863318));
#39909=CARTESIAN_POINT('',(0.005,0.0508228570478122,0.0450513034666297));
#39910=CARTESIAN_POINT('',(0.005,0.050732142762098,0.0466759019477942));
#39911=CARTESIAN_POINT('',(0.005,0.0506414284763837,0.0483005004289586));
#39912=CARTESIAN_POINT('',(0.00404508497187473,0.0505507141906694,0.0496148282092566));
#39913=CARTESIAN_POINT('',(0.00309016994374947,0.0504599999049551,0.0509291559895544));
#39914=CARTESIAN_POINT('',(0.00154508497187473,0.0503692856192409,0.05143118452927));
#39915=CARTESIAN_POINT('',(0.000791922201622682,0.0503250662889298,0.0516759019477941));
#39916=CARTESIAN_POINT('',(8.89120054436383E-19,0.0502785713335266,0.0516759019477941));
#39917=CARTESIAN_POINT('',(-2.22280013609096E-19,0.0511857141906694,0.0416759019477942));
#39918=CARTESIAN_POINT('',(-0.005,0.0516392856192409,0.0466759019477942));
#39919=CARTESIAN_POINT('',(-0.005,0.0515485713335265,0.0450513034666297));
#39920=CARTESIAN_POINT('',(-0.00404508497187473,0.0514578570478123,0.0437369756863318));
#39921=CARTESIAN_POINT('',(-0.00309016994374947,0.0513671427620979,0.042422647906034));
#39922=CARTESIAN_POINT('',(-0.00154508497187473,0.0512764284763837,0.0419206193663185));
#39923=CARTESIAN_POINT('',(-0.000791922201622681,0.0512322091460726,0.0416759019477942));
#39924=CARTESIAN_POINT('',(-2.22280013609096E-19,0.0511857141906695,0.0416759019477942));
#39925=CARTESIAN_POINT('',(-0.005,0.0529999999,0.0466759019477942));
#39926=CARTESIAN_POINT('',(-0.005,0.0529092856142857,0.0450513034666296));
#39927=CARTESIAN_POINT('',(-0.00404508497187473,0.0528185713285714,0.0437369756863318));
#39928=CARTESIAN_POINT('',(-0.00309016994374947,0.0527278570428571,0.042422647906034));
#39929=CARTESIAN_POINT('',(-0.00154508497187473,0.0526371427571429,0.0419206193663185));
#39930=CARTESIAN_POINT('',(-3.21917461834437E-19,0.0525464284714285,0.0414185908266028));
#39931=CARTESIAN_POINT('',(0.00154508497187473,0.0524557141857143,0.0419206193663185));
#39932=CARTESIAN_POINT('',(0.00309016994374947,0.0523649999,0.042422647906034));
#39933=CARTESIAN_POINT('',(0.00404508497187473,0.0522742856142857,0.0437369756863318));
#39934=CARTESIAN_POINT('',(0.005,0.0521835713285714,0.0450513034666296));
#39935=CARTESIAN_POINT('',(0.005,0.0520928570428571,0.0466759019477942));
#39936=CARTESIAN_POINT('',(0.005,0.0520021427571428,0.0483005004289586));
#39937=CARTESIAN_POINT('',(0.00404508497187473,0.0519114284714286,0.0496148282092566));
#39938=CARTESIAN_POINT('',(0.00309016994374947,0.0518207141857143,0.0509291559895544));
#39939=CARTESIAN_POINT('',(0.00154508497187473,0.0517299999,0.05143118452927));
#39940=CARTESIAN_POINT('',(9.65752385503311E-19,0.0516392856142857,0.0519332130689855));
#39941=CARTESIAN_POINT('',(-0.00154508497187473,0.0515485713285714,0.05143118452927));
#39942=CARTESIAN_POINT('',(-0.00309016994374947,0.0514578570428571,0.0509291559895544));
#39943=CARTESIAN_POINT('',(-0.00404508497187473,0.0513671427571429,0.0496148282092566));
#39944=CARTESIAN_POINT('',(-0.005,0.0512764284714286,0.0483005004289586));
#39945=CARTESIAN_POINT('',(-0.005,0.0511857141857143,0.0466759019477942));
#39946=CARTESIAN_POINT('',(-0.005,0.0510949999,0.0450513034666296));
#39947=CARTESIAN_POINT('',(-0.00404508497187473,0.0510042856142857,0.0437369756863318));
#39948=CARTESIAN_POINT('',(-0.00309016994374947,0.0509135713285715,0.042422647906034));
#39949=CARTESIAN_POINT('',(-0.00154508497187473,0.0508228570428571,0.0419206193663185));
#39950=CARTESIAN_POINT('',(-3.21917461834437E-19,0.0507321427571428,0.0414185908266028));
#39951=CARTESIAN_POINT('',(0.00154508497187473,0.0506414284714286,0.0419206193663185));
#39952=CARTESIAN_POINT('',(0.00309016994374947,0.0505507141857142,0.042422647906034));
#39953=CARTESIAN_POINT('',(0.00404508497187473,0.0504599999,0.0437369756863318));
#39954=CARTESIAN_POINT('',(0.005,0.0503692856142857,0.0450513034666296));
#39955=CARTESIAN_POINT('',(0.005,0.0502785713285714,0.0466759019477942));
#39956=CARTESIAN_POINT('',(0.005,0.0501878570428571,0.0483005004289586));
#39957=CARTESIAN_POINT('',(0.00404508497187473,0.0500971427571429,0.0496148282092566));
#39958=CARTESIAN_POINT('',(0.00309016994374947,0.0500064284714285,0.0509291559895544));
#39959=CARTESIAN_POINT('',(0.00154508497187473,0.0499157141857143,0.05143118452927));
#39960=CARTESIAN_POINT('',(9.65752385503311E-19,0.0498249999,0.0519332130689855));
#39961=CARTESIAN_POINT('',(-0.00154508497187473,0.0497342856142857,0.05143118452927));
#39962=CARTESIAN_POINT('',(-0.00309016994374947,0.0496435713285714,0.0509291559895544));
#39963=CARTESIAN_POINT('',(-0.00404508497187473,0.0495528570428571,0.0496148282092566));
#39964=CARTESIAN_POINT('',(-0.005,0.0494621427571428,0.0483005004289586));
#39965=CARTESIAN_POINT('',(-0.005,0.0493714284714286,0.0466759019477942));
#39966=CARTESIAN_POINT('',(-0.005,0.0492807141857143,0.0450513034666296));
#39967=CARTESIAN_POINT('',(-0.00404508497187473,0.0491899999,0.0437369756863318));
#39968=CARTESIAN_POINT('',(-0.00309016994374947,0.0490992856142857,0.042422647906034));
#39969=CARTESIAN_POINT('',(-0.00154508497187473,0.0490085713285714,0.0419206193663185));
#39970=CARTESIAN_POINT('',(-3.21917461834437E-19,0.0489178570428572,0.0414185908266028));
#39971=CARTESIAN_POINT('',(0.00154508497187473,0.0488271427571429,0.0419206193663185));
#39972=CARTESIAN_POINT('',(0.00309016994374947,0.0487364284714286,0.042422647906034));
#39973=CARTESIAN_POINT('',(0.00404508497187473,0.0486457141857143,0.0437369756863318));
#39974=CARTESIAN_POINT('',(0.005,0.0485549999,0.0450513034666296));
#39975=CARTESIAN_POINT('',(0.005,0.0484642856142857,0.0466759019477942));
#39976=CARTESIAN_POINT('',(0.005,0.0483735713285714,0.0483005004289586));
#39977=CARTESIAN_POINT('',(0.00404508497187473,0.0482828570428571,0.0496148282092566));
#39978=CARTESIAN_POINT('',(0.00309016994374947,0.0481921427571428,0.0509291559895544));
#39979=CARTESIAN_POINT('',(0.00154508497187473,0.0481014284714286,0.05143118452927));
#39980=CARTESIAN_POINT('',(9.65752385503311E-19,0.0480107141857142,0.0519332130689855));
#39981=CARTESIAN_POINT('',(-0.00154508497187473,0.0479199999,0.05143118452927));
#39982=CARTESIAN_POINT('',(-0.00309016994374947,0.0478292856142857,0.0509291559895544));
#39983=CARTESIAN_POINT('',(-0.00404508497187473,0.0477385713285714,0.0496148282092566));
#39984=CARTESIAN_POINT('',(-0.005,0.0476478570428571,0.0483005004289586));
#39985=CARTESIAN_POINT('',(-0.005,0.0475571427571429,0.0466759019477942));
#39986=CARTESIAN_POINT('',(-0.005,0.0474664284714285,0.0450513034666296));
#39987=CARTESIAN_POINT('',(-0.00404508497187473,0.0473757141857143,0.0437369756863318));
#39988=CARTESIAN_POINT('',(-0.00309016994374947,0.0472849999,0.042422647906034));
#39989=CARTESIAN_POINT('',(-0.00154508497187473,0.0471942856142857,0.0419206193663185));
#39990=CARTESIAN_POINT('',(-3.21917461834437E-19,0.0471035713285714,0.0414185908266028));
#39991=CARTESIAN_POINT('',(0.00154508497187473,0.0470128570428571,0.0419206193663185));
#39992=CARTESIAN_POINT('',(0.00309016994374947,0.0469221427571428,0.042422647906034));
#39993=CARTESIAN_POINT('',(0.00404508497187473,0.0468314284714286,0.0437369756863318));
#39994=CARTESIAN_POINT('',(0.005,0.0467407141857143,0.0450513034666296));
#39995=CARTESIAN_POINT('',(0.005,0.0466499999,0.0466759019477942));
#39996=CARTESIAN_POINT('',(0.005,0.0465592856142857,0.0483005004289586));
#39997=CARTESIAN_POINT('',(0.00404508497187473,0.0464685713285714,0.0496148282092566));
#39998=CARTESIAN_POINT('',(0.00309016994374947,0.0463778570428571,0.0509291559895544));
#39999=CARTESIAN_POINT('',(0.00154508497187473,0.0462871427571429,0.05143118452927));
#40000=CARTESIAN_POINT('',(9.65752385503311E-19,0.0461964284714286,0.0519332130689855));
#40001=CARTESIAN_POINT('',(-0.00154508497187473,0.0461057141857143,0.05143118452927));
#40002=CARTESIAN_POINT('',(-0.00242540363398948,0.0460540293398396,0.0511451516569875));
#40003=CARTESIAN_POINT('',(-0.00314498864239956,0.0459997579783105,0.050562937635716));
#40004=CARTESIAN_POINT('',(-0.00342983626690057,0.0459782746674725,0.0503324682971777));
#40005=CARTESIAN_POINT('',(-0.00371468389140158,0.0459567913566346,0.0501019989586393));
#40006=CARTESIAN_POINT('',(-0.00598201094464286,0.0524330356167633,0.0466759019477942));
#40007=CARTESIAN_POINT('',(-0.00598201094464285,0.052342321331049,0.0447322287687989));
#40008=CARTESIAN_POINT('',(-0.004839548514753,0.0522516070453347,0.0431597641354809));
#40009=CARTESIAN_POINT('',(-0.00369708608486315,0.0521608927596204,0.041587299502163));
#40010=CARTESIAN_POINT('',(-0.00184854304243157,0.0520701784739062,0.0409866714583427));
#40011=CARTESIAN_POINT('',(-3.8514275599305E-19,0.0519794641881918,0.0403860434145223));
#40012=CARTESIAN_POINT('',(0.00184854304243157,0.0518887499024776,0.0409866714583427));
#40013=CARTESIAN_POINT('',(0.00369708608486315,0.0517980356167633,0.041587299502163));
#40014=CARTESIAN_POINT('',(0.004839548514753,0.051707321331049,0.0431597641354809));
#40015=CARTESIAN_POINT('',(0.00598201094464285,0.0516166070453347,0.0447322287687989));
#40016=CARTESIAN_POINT('',(0.00598201094464286,0.0515258927596204,0.0466759019477942));
#40017=CARTESIAN_POINT('',(0.00598201094464286,0.0514351784739062,0.0486195751267895));
#40018=CARTESIAN_POINT('',(0.004839548514753,0.0513444641881919,0.0501920397601074));
#40019=CARTESIAN_POINT('',(0.00369708608486315,0.0512537499024776,0.0517645043934253));
#40020=CARTESIAN_POINT('',(0.00184854304243157,0.0511630356167633,0.0523651324372457));
#40021=CARTESIAN_POINT('',(1.15542826797915E-18,0.051072321331049,0.052965760481066));
#40022=CARTESIAN_POINT('',(-0.00184854304243157,0.0509816070453347,0.0523651324372457));
#40023=CARTESIAN_POINT('',(-0.00369708608486315,0.0508908927596205,0.0517645043934253));
#40024=CARTESIAN_POINT('',(-0.004839548514753,0.0508001784739061,0.0501920397601074));
#40025=CARTESIAN_POINT('',(-0.00598201094464285,0.0507094641881918,0.0486195751267895));
#40026=CARTESIAN_POINT('',(-0.00598201094464286,0.0506187499024776,0.0466759019477942));
#40027=CARTESIAN_POINT('',(-0.00598201094464285,0.0505280356167632,0.0447322287687989));
#40028=CARTESIAN_POINT('',(-0.004839548514753,0.050437321331049,0.0431597641354809));
#40029=CARTESIAN_POINT('',(-0.00369708608486315,0.0503466070453347,0.041587299502163));
#40030=CARTESIAN_POINT('',(-0.00184854304243157,0.0502558927596204,0.0409866714583427));
#40031=CARTESIAN_POINT('',(-3.8514275599305E-19,0.0501651784739061,0.0403860434145223));
#40032=CARTESIAN_POINT('',(0.00184854304243157,0.0500744641881919,0.0409866714583427));
#40033=CARTESIAN_POINT('',(0.00369708608486315,0.0499837499024775,0.041587299502163));
#40034=CARTESIAN_POINT('',(0.004839548514753,0.0498930356167633,0.0431597641354809));
#40035=CARTESIAN_POINT('',(0.00598201094464285,0.049802321331049,0.0447322287687989));
#40036=CARTESIAN_POINT('',(0.00598201094464286,0.0497116070453347,0.0466759019477942));
#40037=CARTESIAN_POINT('',(0.00598201094464286,0.0496208927596204,0.0486195751267895));
#40038=CARTESIAN_POINT('',(0.004839548514753,0.0495301784739061,0.0501920397601074));
#40039=CARTESIAN_POINT('',(0.00369708608486315,0.0494394641881919,0.0517645043934253));
#40040=CARTESIAN_POINT('',(0.00184854304243157,0.0493487499024776,0.0523651324372457));
#40041=CARTESIAN_POINT('',(1.15542826797915E-18,0.0492580356167633,0.052965760481066));
#40042=CARTESIAN_POINT('',(-0.00184854304243157,0.049167321331049,0.0523651324372457));
#40043=CARTESIAN_POINT('',(-0.00369708608486315,0.0490766070453347,0.0517645043934253));
#40044=CARTESIAN_POINT('',(-0.004839548514753,0.0489858927596204,0.0501920397601074));
#40045=CARTESIAN_POINT('',(-0.00598201094464285,0.0488951784739062,0.0486195751267895));
#40046=CARTESIAN_POINT('',(-0.00598201094464286,0.0488044641881919,0.0466759019477942));
#40047=CARTESIAN_POINT('',(-0.00598201094464285,0.0487137499024776,0.0447322287687989));
#40048=CARTESIAN_POINT('',(-0.004839548514753,0.0486230356167633,0.0431597641354809));
#40049=CARTESIAN_POINT('',(-0.00369708608486315,0.0485323213310489,0.041587299502163));
#40050=CARTESIAN_POINT('',(-0.00184854304243157,0.0484416070453347,0.0409866714583427));
#40051=CARTESIAN_POINT('',(-3.8514275599305E-19,0.0483508927596204,0.0403860434145223));
#40052=CARTESIAN_POINT('',(0.00184854304243157,0.0482601784739061,0.0409866714583427));
#40053=CARTESIAN_POINT('',(0.00369708608486315,0.0481694641881918,0.041587299502163));
#40054=CARTESIAN_POINT('',(0.004839548514753,0.0480787499024776,0.0431597641354809));
#40055=CARTESIAN_POINT('',(0.00598201094464285,0.0479880356167633,0.0447322287687989));
#40056=CARTESIAN_POINT('',(0.00598201094464286,0.047897321331049,0.0466759019477942));
#40057=CARTESIAN_POINT('',(0.00598201094464286,0.0478066070453347,0.0486195751267895));
#40058=CARTESIAN_POINT('',(0.004839548514753,0.0477158927596204,0.0501920397601074));
#40059=CARTESIAN_POINT('',(0.00369708608486315,0.0476251784739061,0.0517645043934253));
#40060=CARTESIAN_POINT('',(0.00184854304243157,0.0475344641881919,0.0523651324372457));
#40061=CARTESIAN_POINT('',(1.15542826797915E-18,0.0474437499024775,0.052965760481066));
#40062=CARTESIAN_POINT('',(-0.00184854304243157,0.0473530356167633,0.0523651324372457));
#40063=CARTESIAN_POINT('',(-0.00369708608486315,0.047262321331049,0.0517645043934253));
#40064=CARTESIAN_POINT('',(-0.004839548514753,0.0471716070453347,0.0501920397601074));
#40065=CARTESIAN_POINT('',(-0.00598201094464285,0.0470808927596204,0.0486195751267895));
#40066=CARTESIAN_POINT('',(-0.00598201094464286,0.0469901784739061,0.0466759019477942));
#40067=CARTESIAN_POINT('',(-0.00598201094464285,0.0468994641881918,0.0447322287687989));
#40068=CARTESIAN_POINT('',(-0.004839548514753,0.0468087499024776,0.0431597641354809));
#40069=CARTESIAN_POINT('',(-0.00369708608486315,0.0467180356167633,0.041587299502163));
#40070=CARTESIAN_POINT('',(-0.00184854304243157,0.046627321331049,0.0409866714583427));
#40071=CARTESIAN_POINT('',(-3.8514275599305E-19,0.0465366070453347,0.0403860434145223));
#40072=CARTESIAN_POINT('',(0.00184854304243157,0.0464458927596204,0.0409866714583427));
#40073=CARTESIAN_POINT('',(0.00369708608486315,0.0463551784739062,0.041587299502163));
#40074=CARTESIAN_POINT('',(0.004839548514753,0.0462644641881919,0.0431597641354809));
#40075=CARTESIAN_POINT('',(0.00598201094464285,0.0461737499024775,0.0447322287687989));
#40076=CARTESIAN_POINT('',(0.00598201094464286,0.0460830356167633,0.0466759019477942));
#40077=CARTESIAN_POINT('',(0.00598201094464286,0.045992321331049,0.0486195751267895));
#40078=CARTESIAN_POINT('',(0.004839548514753,0.0459016070453347,0.0501920397601074));
#40079=CARTESIAN_POINT('',(0.00369708608486315,0.0458108927596204,0.0517645043934253));
#40080=CARTESIAN_POINT('',(0.00184854304243157,0.0457201784739062,0.0523651324372457));
#40081=CARTESIAN_POINT('',(1.15542826797915E-18,0.0456294641881918,0.052965760481066));
#40082=CARTESIAN_POINT('',(-0.00184854304243157,0.0455387499024776,0.0523651324372457));
#40083=CARTESIAN_POINT('',(-0.00290175821674032,0.0454870650566028,0.0520229220827414));
#40084=CARTESIAN_POINT('',(-0.00376267129592233,0.0454327936950738,0.0513263599532673));
#40085=CARTESIAN_POINT('',(-0.00410346361738644,0.0454113103842358,0.0510506259321592));
#40086=CARTESIAN_POINT('',(-0.00444425593885055,0.0453898270733979,0.050774891911051));
#40087=CARTESIAN_POINT('',(-0.00598790325387306,0.0524296336904431,0.0466759019477942));
#40088=CARTESIAN_POINT('',(-0.00598790325387306,0.0523389194047288,0.0447303142414737));
#40089=CARTESIAN_POINT('',(-0.00484431549305635,0.0522482051190145,0.0431563007230135));
#40090=CARTESIAN_POINT('',(-0.00370072773223964,0.0521574908333002,0.0415822872045532));
#40091=CARTESIAN_POINT('',(-0.00185036386611982,0.052066776547586,0.0409810675392532));
#40092=CARTESIAN_POINT('',(-3.85522123439397E-19,0.0519760622618717,0.0403798478739532));
#40093=CARTESIAN_POINT('',(0.00185036386611982,0.0518853479761574,0.0409810675392532));
#40094=CARTESIAN_POINT('',(0.00370072773223964,0.0517946336904431,0.0415822872045532));
#40095=CARTESIAN_POINT('',(0.00484431549305635,0.0517039194047288,0.0431563007230135));
#40096=CARTESIAN_POINT('',(0.00598790325387306,0.0516132051190145,0.0447303142414737));
#40097=CARTESIAN_POINT('',(0.00598790325387306,0.0515224908333002,0.0466759019477942));
#40098=CARTESIAN_POINT('',(0.00598790325387306,0.051431776547586,0.0486214896541146));
#40099=CARTESIAN_POINT('',(0.00484431549305635,0.0513410622618717,0.0501955031725749));
#40100=CARTESIAN_POINT('',(0.00370072773223964,0.0512503479761574,0.0517695166910351));
#40101=CARTESIAN_POINT('',(0.00185036386611982,0.0511596336904431,0.0523707363563351));
#40102=CARTESIAN_POINT('',(1.15656637031819E-18,0.0510689194047287,0.0529719560216351));
#40103=CARTESIAN_POINT('',(-0.00185036386611982,0.0509782051190145,0.0523707363563351));
#40104=CARTESIAN_POINT('',(-0.00370072773223964,0.0508874908333002,0.0517695166910351));
#40105=CARTESIAN_POINT('',(-0.00484431549305635,0.0507967765475859,0.0501955031725749));
#40106=CARTESIAN_POINT('',(-0.00598790325387306,0.0507060622618716,0.0486214896541146));
#40107=CARTESIAN_POINT('',(-0.00598790325387306,0.0506153479761574,0.0466759019477942));
#40108=CARTESIAN_POINT('',(-0.00598790325387306,0.050524633690443,0.0447303142414737));
#40109=CARTESIAN_POINT('',(-0.00484431549305635,0.0504339194047288,0.0431563007230135));
#40110=CARTESIAN_POINT('',(-0.00370072773223964,0.0503432051190145,0.0415822872045532));
#40111=CARTESIAN_POINT('',(-0.00185036386611982,0.0502524908333002,0.0409810675392532));
#40112=CARTESIAN_POINT('',(-3.85522123439397E-19,0.0501617765475859,0.0403798478739532));
#40113=CARTESIAN_POINT('',(0.00185036386611982,0.0500710622618717,0.0409810675392532));
#40114=CARTESIAN_POINT('',(0.00370072773223964,0.0499803479761574,0.0415822872045532));
#40115=CARTESIAN_POINT('',(0.00484431549305635,0.0498896336904431,0.0431563007230135));
#40116=CARTESIAN_POINT('',(0.00598790325387306,0.0497989194047288,0.0447303142414737));
#40117=CARTESIAN_POINT('',(0.00598790325387306,0.0497082051190145,0.0466759019477942));
#40118=CARTESIAN_POINT('',(0.00598790325387306,0.0496174908333002,0.0486214896541146));
#40119=CARTESIAN_POINT('',(0.00484431549305635,0.0495267765475859,0.0501955031725749));
#40120=CARTESIAN_POINT('',(0.00370072773223964,0.0494360622618717,0.0517695166910351));
#40121=CARTESIAN_POINT('',(0.00185036386611982,0.0493453479761574,0.0523707363563351));
#40122=CARTESIAN_POINT('',(1.15656637031819E-18,0.0492546336904431,0.0529719560216351));
#40123=CARTESIAN_POINT('',(-0.00185036386611982,0.0491639194047288,0.0523707363563351));
#40124=CARTESIAN_POINT('',(-0.00370072773223964,0.0490732051190145,0.0517695166910351));
#40125=CARTESIAN_POINT('',(-0.00484431549305635,0.0489824908333002,0.0501955031725749));
#40126=CARTESIAN_POINT('',(-0.00598790325387306,0.048891776547586,0.0486214896541146));
#40127=CARTESIAN_POINT('',(-0.00598790325387306,0.0488010622618717,0.0466759019477942));
#40128=CARTESIAN_POINT('',(-0.00598790325387306,0.0487103479761573,0.0447303142414737));
#40129=CARTESIAN_POINT('',(-0.00484431549305635,0.0486196336904431,0.0431563007230135));
#40130=CARTESIAN_POINT('',(-0.00370072773223964,0.0485289194047288,0.0415822872045532));
#40131=CARTESIAN_POINT('',(-0.00185036386611982,0.0484382051190145,0.0409810675392532));
#40132=CARTESIAN_POINT('',(-3.85522123439397E-19,0.0483474908333002,0.0403798478739532));
#40133=CARTESIAN_POINT('',(0.00185036386611982,0.0482567765475859,0.0409810675392532));
#40134=CARTESIAN_POINT('',(0.00370072773223964,0.0481660622618716,0.0415822872045532));
#40135=CARTESIAN_POINT('',(0.00484431549305635,0.0480753479761574,0.0431563007230135));
#40136=CARTESIAN_POINT('',(0.00598790325387306,0.0479846336904431,0.0447303142414737));
#40137=CARTESIAN_POINT('',(0.00598790325387306,0.0478939194047288,0.0466759019477942));
#40138=CARTESIAN_POINT('',(0.00598790325387306,0.0478032051190145,0.0486214896541146));
#40139=CARTESIAN_POINT('',(0.00484431549305635,0.0477124908333002,0.0501955031725749));
#40140=CARTESIAN_POINT('',(0.00370072773223964,0.0476217765475859,0.0517695166910351));
#40141=CARTESIAN_POINT('',(0.00185036386611982,0.0475310622618717,0.0523707363563351));
#40142=CARTESIAN_POINT('',(1.15656637031819E-18,0.0474403479761574,0.0529719560216351));
#40143=CARTESIAN_POINT('',(-0.00185036386611982,0.0473496336904431,0.0523707363563351));
#40144=CARTESIAN_POINT('',(-0.00370072773223964,0.0472589194047288,0.0517695166910351));
#40145=CARTESIAN_POINT('',(-0.00484431549305635,0.0471682051190145,0.0501955031725749));
#40146=CARTESIAN_POINT('',(-0.00598790325387306,0.0470774908333002,0.0486214896541146));
#40147=CARTESIAN_POINT('',(-0.00598790325387306,0.0469867765475859,0.0466759019477942));
#40148=CARTESIAN_POINT('',(-0.00598790325387306,0.0468960622618716,0.0447303142414737));
#40149=CARTESIAN_POINT('',(-0.00484431549305635,0.0468053479761574,0.0431563007230135));
#40150=CARTESIAN_POINT('',(-0.00370072773223964,0.0467146336904431,0.0415822872045532));
#40151=CARTESIAN_POINT('',(-0.00185036386611982,0.0466239194047288,0.0409810675392532));
#40152=CARTESIAN_POINT('',(-3.85522123439397E-19,0.0465332051190145,0.0403798478739532));
#40153=CARTESIAN_POINT('',(0.00185036386611982,0.0464424908333002,0.0409810675392532));
#40154=CARTESIAN_POINT('',(0.00370072773223964,0.046351776547586,0.0415822872045532));
#40155=CARTESIAN_POINT('',(0.00484431549305635,0.0462610622618717,0.0431563007230135));
#40156=CARTESIAN_POINT('',(0.00598790325387306,0.0461703479761574,0.0447303142414737));
#40157=CARTESIAN_POINT('',(0.00598790325387306,0.0460796336904431,0.0466759019477942));
#40158=CARTESIAN_POINT('',(0.00598790325387306,0.0459889194047288,0.0486214896541146));
#40159=CARTESIAN_POINT('',(0.00484431549305635,0.0458982051190145,0.0501955031725749));
#40160=CARTESIAN_POINT('',(0.00370072773223964,0.0458074908333002,0.0517695166910351));
#40161=CARTESIAN_POINT('',(0.00185036386611982,0.045716776547586,0.0523707363563351));
#40162=CARTESIAN_POINT('',(1.15656637031819E-18,0.0456260622618716,0.0529719560216351));
#40163=CARTESIAN_POINT('',(-0.00185036386611982,0.0455353479761574,0.0523707363563351));
#40164=CARTESIAN_POINT('',(-0.00290461646238423,0.0454836631302826,0.0520281889230041));
#40165=CARTESIAN_POINT('',(-0.00376637754504363,0.0454293917687536,0.0513309406765197));
#40166=CARTESIAN_POINT('',(-0.00410750554856515,0.0454079084579156,0.0510549350560894));
#40167=CARTESIAN_POINT('',(-0.00444863355208667,0.0453864251470777,0.0507789294356591));
#40168=CARTESIAN_POINT('',(-0.00549100547232143,0.0527165177583816,0.0466759019477942));
#40169=CARTESIAN_POINT('',(-0.005,0.0529999999,0.0466759019477942));
#40170=CARTESIAN_POINT('',(-0.00598201094464286,0.0524330356167633,0.0466759019477942));
#40171=CARTESIAN_POINT('',(-0.005,0.0529999999,0.0466759019477942));
#40172=CARTESIAN_POINT('',(-0.005,0.0529092856142857,0.0450513034666297));
#40173=CARTESIAN_POINT('',(-0.00404508497187473,0.0528185713285714,0.0437369756863318));
#40174=CARTESIAN_POINT('',(-0.00309016994374947,0.0527278570428571,0.042422647906034));
#40175=CARTESIAN_POINT('',(-0.00154508497187473,0.0526371427571429,0.0419206193663185));
#40176=CARTESIAN_POINT('',(-0.000791922201622684,0.0525929234268318,0.0416759019477942));
#40177=CARTESIAN_POINT('',(-2.05609012588414E-18,0.0525464284714286,0.0416759019477942));
#40178=CARTESIAN_POINT('',(-2.05609012588413E-18,0.0525464284714286,0.0416759019477942));
#40179=CARTESIAN_POINT('',(-2.05609012588414E-18,0.0525464284714286,0.0416759019477942));
#40180=CARTESIAN_POINT('',(0.000791922201622679,0.0524999335160253,0.0416759019477942));
#40181=CARTESIAN_POINT('',(0.00154508497187473,0.0524557141857143,0.0419206193663185));
#40182=CARTESIAN_POINT('',(0.00309016994374947,0.0523649999,0.042422647906034));
#40183=CARTESIAN_POINT('',(0.00404508497187473,0.0522742856142857,0.0437369756863318));
#40184=CARTESIAN_POINT('',(0.005,0.0521835713285714,0.0450513034666296));
#40185=CARTESIAN_POINT('',(0.005,0.0520928570428571,0.0466759019477942));
#40186=CARTESIAN_POINT('',(0.005,0.0520021427571428,0.0483005004289586));
#40187=CARTESIAN_POINT('',(0.00404508497187473,0.0519114284714286,0.0496148282092566));
#40188=CARTESIAN_POINT('',(0.00309016994374947,0.0518207141857143,0.0509291559895544));
#40189=CARTESIAN_POINT('',(0.00154508497187474,0.0517299999,0.05143118452927));
#40190=CARTESIAN_POINT('',(0.000791922201622684,0.0516857805696889,0.0516759019477941));
#40191=CARTESIAN_POINT('',(4.44560027218191E-18,0.0516392856142857,0.0516759019477941));
#40192=CARTESIAN_POINT('',(4.44560027218192E-18,0.0516392856142857,0.0516759019477942));
#40193=CARTESIAN_POINT('',(4.44560027218191E-18,0.0516392856142857,0.0516759019477941));
#40194=CARTESIAN_POINT('',(-0.000791922201622684,0.0515927906588825,0.0516759019477942));
#40195=CARTESIAN_POINT('',(-0.00154508497187474,0.0515485713285714,0.05143118452927));
#40196=CARTESIAN_POINT('',(-0.00309016994374949,0.0514578570428571,0.0509291559895544));
#40197=CARTESIAN_POINT('',(-0.00404508497187476,0.0513671427571428,0.0496148282092566));
#40198=CARTESIAN_POINT('',(-0.00500000000000003,0.0512764284714286,0.0483005004289587));
#40199=CARTESIAN_POINT('',(-0.005,0.0511857141857143,0.0466759019477942));
#40200=CARTESIAN_POINT('',(-0.00500000000000003,0.0510949999,0.0450513034666296));
#40201=CARTESIAN_POINT('',(-0.00404508497187476,0.0510042856142857,0.0437369756863318));
#40202=CARTESIAN_POINT('',(-0.00309016994374949,0.0509135713285715,0.0424226479060339));
#40203=CARTESIAN_POINT('',(-0.00154508497187475,0.0508228570428571,0.0419206193663184));
#40204=CARTESIAN_POINT('',(-0.000791922201629948,0.0507786377125465,0.0416759019477965));
#40205=CARTESIAN_POINT('',(-1.49045973225341E-14,0.0507321427571437,0.0416759019477942));
#40206=CARTESIAN_POINT('',(-1.49045973225341E-14,0.0507321427571437,0.0416759019477942));
#40207=CARTESIAN_POINT('',(-1.49045973225341E-14,0.0507321427571437,0.0416759019477942));
#40208=CARTESIAN_POINT('',(0.000791922201615424,0.0506856478017401,0.0416759019477918));
#40209=CARTESIAN_POINT('',(0.00154508497187474,0.0506414284714286,0.0419206193663184));
#40210=CARTESIAN_POINT('',(0.00309016994374949,0.0505507141857142,0.0424226479060339));
#40211=CARTESIAN_POINT('',(0.00404508497187476,0.0504599999,0.0437369756863318));
#40212=CARTESIAN_POINT('',(0.00500000000000003,0.0503692856142857,0.0450513034666296));
#40213=CARTESIAN_POINT('',(0.005,0.0502785713285714,0.0466759019477942));
#40214=CARTESIAN_POINT('',(0.00500000000000003,0.0501878570428571,0.0483005004289587));
#40215=CARTESIAN_POINT('',(0.00404508497187476,0.0500971427571428,0.0496148282092566));
#40216=CARTESIAN_POINT('',(0.00309016994374949,0.0500064284714285,0.0509291559895544));
#40217=CARTESIAN_POINT('',(0.00154508497187475,0.0499157141857143,0.05143118452927));
#40218=CARTESIAN_POINT('',(0.000791922201622684,0.0498714948554032,0.0516759019477942));
#40219=CARTESIAN_POINT('',(-6.11270037425013E-18,0.0498249999,0.0516759019477941));
#40220=CARTESIAN_POINT('',(-6.11270037425013E-18,0.0498249999,0.0516759019477942));
#40221=CARTESIAN_POINT('',(-6.11270037425013E-18,0.0498249999,0.0516759019477941));
#40222=CARTESIAN_POINT('',(-0.000791922201622682,0.0497785049445967,0.0516759019477941));
#40223=CARTESIAN_POINT('',(-0.00154508497187473,0.0497342856142857,0.0514311845292699));
#40224=CARTESIAN_POINT('',(-0.00309016994374947,0.0496435713285714,0.0509291559895543));
#40225=CARTESIAN_POINT('',(-0.00404508497187473,0.0495528570428571,0.0496148282092566));
#40226=CARTESIAN_POINT('',(-0.00499999999999999,0.0494621427571428,0.0483005004289586));
#40227=CARTESIAN_POINT('',(-0.005,0.0493714284714286,0.0466759019477942));
#40228=CARTESIAN_POINT('',(-0.00499999999999999,0.0492807141857143,0.0450513034666297));
#40229=CARTESIAN_POINT('',(-0.00404508497187473,0.0491899999,0.0437369756863318));
#40230=CARTESIAN_POINT('',(-0.00309016994374947,0.0490992856142857,0.042422647906034));
#40231=CARTESIAN_POINT('',(-0.00154508497187473,0.0490085713285714,0.0419206193663185));
#40232=CARTESIAN_POINT('',(-0.00079192220162268,0.0489643519982604,0.0416759019477942));
#40233=CARTESIAN_POINT('',(-2.7785001701137E-19,0.0489178570428571,0.0416759019477942));
#40234=CARTESIAN_POINT('',(-2.77850017011369E-19,0.0489178570428571,0.0416759019477942));
#40235=CARTESIAN_POINT('',(-2.7785001701137E-19,0.0489178570428571,0.0416759019477942));
#40236=CARTESIAN_POINT('',(0.000791922201622679,0.048871362087454,0.0416759019477942));
#40237=CARTESIAN_POINT('',(0.00154508497187473,0.0488271427571429,0.0419206193663185));
#40238=CARTESIAN_POINT('',(0.00309016994374946,0.0487364284714286,0.042422647906034));
#40239=CARTESIAN_POINT('',(0.00404508497187472,0.0486457141857143,0.0437369756863318));
#40240=CARTESIAN_POINT('',(0.00499999999999998,0.0485549999,0.0450513034666297));
#40241=CARTESIAN_POINT('',(0.005,0.0484642856142857,0.0466759019477942));
#40242=CARTESIAN_POINT('',(0.00499999999999998,0.0483735713285714,0.0483005004289586));
#40243=CARTESIAN_POINT('',(0.00404508497187472,0.0482828570428572,0.0496148282092566));
#40244=CARTESIAN_POINT('',(0.00309016994374946,0.0481921427571428,0.0509291559895543));
#40245=CARTESIAN_POINT('',(0.00154508497187473,0.0481014284714286,0.0514311845292699));
#40246=CARTESIAN_POINT('',(0.000791922201633343,0.0480572091411181,0.0516759019477907));
#40247=CARTESIAN_POINT('',(2.18756875393391E-14,0.0480107141857156,0.0516759019477941));
#40248=CARTESIAN_POINT('',(2.18756875393391E-14,0.0480107141857156,0.0516759019477942));
#40249=CARTESIAN_POINT('',(2.18756875393391E-14,0.0480107141857156,0.0516759019477941));
#40250=CARTESIAN_POINT('',(-0.000791922201612015,0.0479642192303117,0.0516759019477976));
#40251=CARTESIAN_POINT('',(-0.00154508497187473,0.0479199999,0.0514311845292699));
#40252=CARTESIAN_POINT('',(-0.00309016994374946,0.0478292856142857,0.0509291559895543));
#40253=CARTESIAN_POINT('',(-0.00404508497187472,0.0477385713285714,0.0496148282092566));
#40254=CARTESIAN_POINT('',(-0.00499999999999998,0.0476478570428571,0.0483005004289586));
#40255=CARTESIAN_POINT('',(-0.005,0.0475571427571429,0.0466759019477942));
#40256=CARTESIAN_POINT('',(-0.00499999999999998,0.0474664284714286,0.0450513034666297));
#40257=CARTESIAN_POINT('',(-0.00404508497187472,0.0473757141857143,0.0437369756863318));
#40258=CARTESIAN_POINT('',(-0.00309016994374946,0.0472849999,0.042422647906034));
#40259=CARTESIAN_POINT('',(-0.00154508497187473,0.0471942856142857,0.0419206193663185));
#40260=CARTESIAN_POINT('',(-0.000791922201622666,0.0471500662839747,0.0416759019477942));
#40261=CARTESIAN_POINT('',(2.78405717045393E-17,0.0471035713285714,0.0416759019477942));
#40262=CARTESIAN_POINT('',(2.78405717045392E-17,0.0471035713285714,0.0416759019477942));
#40263=CARTESIAN_POINT('',(2.78405717045393E-17,0.0471035713285714,0.0416759019477942));
#40264=CARTESIAN_POINT('',(0.00079192220162271,0.0470570763731681,0.0416759019477941));
#40265=CARTESIAN_POINT('',(0.00154508497187477,0.0470128570428571,0.0419206193663183));
#40266=CARTESIAN_POINT('',(0.00309016994374953,0.0469221427571428,0.0424226479060339));
#40267=CARTESIAN_POINT('',(0.00404508497187482,0.0468314284714285,0.0437369756863317));
#40268=CARTESIAN_POINT('',(0.00500000000000009,0.0467407141857142,0.0450513034666296));
#40269=CARTESIAN_POINT('',(0.0050000000000001,0.0466499998999999,0.0466759019477942));
#40270=CARTESIAN_POINT('',(0.00500000000000009,0.0465592856142856,0.0483005004289587));
#40271=CARTESIAN_POINT('',(0.00404508497187482,0.0464685713285714,0.0496148282092566));
#40272=CARTESIAN_POINT('',(0.00309016994374953,0.0463778570428571,0.0509291559895544));
#40273=CARTESIAN_POINT('',(0.00154508497187477,0.0462871427571428,0.05143118452927));
#40274=CARTESIAN_POINT('',(0.000791922201622793,0.0462429234268318,0.0516759019477943));
#40275=CARTESIAN_POINT('',(1.83714431247917E-16,0.0461964284714285,0.0516759019477941));
#40276=CARTESIAN_POINT('',(1.83714431247917E-16,0.0461964284714286,0.0516759019477942));
#40277=CARTESIAN_POINT('',(1.83714431247918E-16,0.0461964284714286,0.0516759019477942));
#40278=CARTESIAN_POINT('',(-0.00114474007368374,0.0461292190428191,0.0516759019477942));
#40279=CARTESIAN_POINT('',(-0.00225506927301393,0.046066874298055,0.0512829728428846));
#40280=CARTESIAN_POINT('',(-0.0031449996694696,0.0459997571466553,0.0505629287137221));
#40281=CARTESIAN_POINT('',(-0.00314499966946895,0.045999757146644,0.0505629287137221));
#40282=CARTESIAN_POINT('',(-0.00345383548269564,0.0457162754208589,0.0509446443334947));
#40283=CARTESIAN_POINT('',(-0.00376267129592233,0.0454327936950738,0.0513263599532673));
#40284=CARTESIAN_POINT('',(-0.00598201094464286,0.0524330356167633,0.0466759019477942));
#40285=CARTESIAN_POINT('',(-0.00598201094464285,0.052342321331049,0.0447322287687989));
#40286=CARTESIAN_POINT('',(-0.004839548514753,0.0522516070453347,0.0431597641354809));
#40287=CARTESIAN_POINT('',(-0.00369708608486315,0.0521608927596204,0.041587299502163));
#40288=CARTESIAN_POINT('',(-0.00184854304243157,0.0520701784739062,0.0409866714583427));
#40289=CARTESIAN_POINT('',(-3.8514275599305E-19,0.0519794641881918,0.0403860434145223));
#40290=CARTESIAN_POINT('',(0.00184854304243157,0.0518887499024776,0.0409866714583427));
#40291=CARTESIAN_POINT('',(0.00369708608486315,0.0517980356167633,0.041587299502163));
#40292=CARTESIAN_POINT('',(0.004839548514753,0.051707321331049,0.0431597641354809));
#40293=CARTESIAN_POINT('',(0.00598201094464285,0.0516166070453347,0.0447322287687989));
#40294=CARTESIAN_POINT('',(0.00598201094464286,0.0515258927596204,0.0466759019477942));
#40295=CARTESIAN_POINT('',(0.00598201094464286,0.0514351784739062,0.0486195751267895));
#40296=CARTESIAN_POINT('',(0.004839548514753,0.0513444641881919,0.0501920397601074));
#40297=CARTESIAN_POINT('',(0.00369708608486315,0.0512537499024776,0.0517645043934253));
#40298=CARTESIAN_POINT('',(0.00184854304243157,0.0511630356167633,0.0523651324372457));
#40299=CARTESIAN_POINT('',(1.15542826797915E-18,0.051072321331049,0.052965760481066));
#40300=CARTESIAN_POINT('',(-0.00184854304243157,0.0509816070453347,0.0523651324372457));
#40301=CARTESIAN_POINT('',(-0.00369708608486315,0.0508908927596205,0.0517645043934253));
#40302=CARTESIAN_POINT('',(-0.004839548514753,0.0508001784739061,0.0501920397601074));
#40303=CARTESIAN_POINT('',(-0.00598201094464285,0.0507094641881918,0.0486195751267895));
#40304=CARTESIAN_POINT('',(-0.00598201094464286,0.0506187499024776,0.0466759019477942));
#40305=CARTESIAN_POINT('',(-0.00598201094464285,0.0505280356167632,0.0447322287687989));
#40306=CARTESIAN_POINT('',(-0.004839548514753,0.050437321331049,0.0431597641354809));
#40307=CARTESIAN_POINT('',(-0.00369708608486315,0.0503466070453347,0.041587299502163));
#40308=CARTESIAN_POINT('',(-0.00184854304243157,0.0502558927596204,0.0409866714583427));
#40309=CARTESIAN_POINT('',(-3.8514275599305E-19,0.0501651784739061,0.0403860434145223));
#40310=CARTESIAN_POINT('',(0.00184854304243157,0.0500744641881919,0.0409866714583427));
#40311=CARTESIAN_POINT('',(0.00369708608486315,0.0499837499024775,0.041587299502163));
#40312=CARTESIAN_POINT('',(0.004839548514753,0.0498930356167633,0.0431597641354809));
#40313=CARTESIAN_POINT('',(0.00598201094464285,0.049802321331049,0.0447322287687989));
#40314=CARTESIAN_POINT('',(0.00598201094464286,0.0497116070453347,0.0466759019477942));
#40315=CARTESIAN_POINT('',(0.00598201094464286,0.0496208927596204,0.0486195751267895));
#40316=CARTESIAN_POINT('',(0.004839548514753,0.0495301784739061,0.0501920397601074));
#40317=CARTESIAN_POINT('',(0.00369708608486315,0.0494394641881919,0.0517645043934253));
#40318=CARTESIAN_POINT('',(0.00184854304243157,0.0493487499024776,0.0523651324372457));
#40319=CARTESIAN_POINT('',(1.15542826797915E-18,0.0492580356167633,0.052965760481066));
#40320=CARTESIAN_POINT('',(-0.00184854304243157,0.049167321331049,0.0523651324372457));
#40321=CARTESIAN_POINT('',(-0.00369708608486315,0.0490766070453347,0.0517645043934253));
#40322=CARTESIAN_POINT('',(-0.004839548514753,0.0489858927596204,0.0501920397601074));
#40323=CARTESIAN_POINT('',(-0.00598201094464285,0.0488951784739062,0.0486195751267895));
#40324=CARTESIAN_POINT('',(-0.00598201094464286,0.0488044641881919,0.0466759019477942));
#40325=CARTESIAN_POINT('',(-0.00598201094464285,0.0487137499024776,0.0447322287687989));
#40326=CARTESIAN_POINT('',(-0.004839548514753,0.0486230356167633,0.0431597641354809));
#40327=CARTESIAN_POINT('',(-0.00369708608486315,0.0485323213310489,0.041587299502163));
#40328=CARTESIAN_POINT('',(-0.00184854304243157,0.0484416070453347,0.0409866714583427));
#40329=CARTESIAN_POINT('',(-3.8514275599305E-19,0.0483508927596204,0.0403860434145223));
#40330=CARTESIAN_POINT('',(0.00184854304243157,0.0482601784739061,0.0409866714583427));
#40331=CARTESIAN_POINT('',(0.00369708608486315,0.0481694641881918,0.041587299502163));
#40332=CARTESIAN_POINT('',(0.004839548514753,0.0480787499024776,0.0431597641354809));
#40333=CARTESIAN_POINT('',(0.00598201094464285,0.0479880356167633,0.0447322287687989));
#40334=CARTESIAN_POINT('',(0.00598201094464286,0.047897321331049,0.0466759019477942));
#40335=CARTESIAN_POINT('',(0.00598201094464286,0.0478066070453347,0.0486195751267895));
#40336=CARTESIAN_POINT('',(0.004839548514753,0.0477158927596204,0.0501920397601074));
#40337=CARTESIAN_POINT('',(0.00369708608486315,0.0476251784739061,0.0517645043934253));
#40338=CARTESIAN_POINT('',(0.00184854304243157,0.0475344641881919,0.0523651324372457));
#40339=CARTESIAN_POINT('',(1.15542826797915E-18,0.0474437499024775,0.052965760481066));
#40340=CARTESIAN_POINT('',(-0.00184854304243157,0.0473530356167633,0.0523651324372457));
#40341=CARTESIAN_POINT('',(-0.00369708608486315,0.047262321331049,0.0517645043934253));
#40342=CARTESIAN_POINT('',(-0.004839548514753,0.0471716070453347,0.0501920397601074));
#40343=CARTESIAN_POINT('',(-0.00598201094464285,0.0470808927596204,0.0486195751267895));
#40344=CARTESIAN_POINT('',(-0.00598201094464286,0.0469901784739061,0.0466759019477942));
#40345=CARTESIAN_POINT('',(-0.00598201094464285,0.0468994641881918,0.0447322287687989));
#40346=CARTESIAN_POINT('',(-0.004839548514753,0.0468087499024776,0.0431597641354809));
#40347=CARTESIAN_POINT('',(-0.00369708608486315,0.0467180356167633,0.041587299502163));
#40348=CARTESIAN_POINT('',(-0.00184854304243157,0.046627321331049,0.0409866714583427));
#40349=CARTESIAN_POINT('',(-3.8514275599305E-19,0.0465366070453347,0.0403860434145223));
#40350=CARTESIAN_POINT('',(0.00184854304243157,0.0464458927596204,0.0409866714583427));
#40351=CARTESIAN_POINT('',(0.00369708608486315,0.0463551784739062,0.041587299502163));
#40352=CARTESIAN_POINT('',(0.004839548514753,0.0462644641881919,0.0431597641354809));
#40353=CARTESIAN_POINT('',(0.00598201094464285,0.0461737499024775,0.0447322287687989));
#40354=CARTESIAN_POINT('',(0.00598201094464286,0.0460830356167633,0.0466759019477942));
#40355=CARTESIAN_POINT('',(0.00598201094464286,0.045992321331049,0.0486195751267895));
#40356=CARTESIAN_POINT('',(0.004839548514753,0.0459016070453347,0.0501920397601074));
#40357=CARTESIAN_POINT('',(0.00369708608486315,0.0458108927596204,0.0517645043934253));
#40358=CARTESIAN_POINT('',(0.00184854304243157,0.0457201784739062,0.0523651324372457));
#40359=CARTESIAN_POINT('',(1.15542826797915E-18,0.0456294641881918,0.052965760481066));
#40360=CARTESIAN_POINT('',(-0.00184854304243157,0.0455387499024776,0.0523651324372457));
#40361=CARTESIAN_POINT('',(-0.00290176072609409,0.0454870649334603,0.052022921267403));
#40362=CARTESIAN_POINT('',(-0.00376267129592233,0.0454327936950738,0.0513263599532673));
#40363=CARTESIAN_POINT('',(-0.00598201094464286,0.0524330356167633,0.0466759019477942));
#40364=CARTESIAN_POINT('',(-0.00598201094464285,0.0523981542391963,0.0459285224420255));
#40365=CARTESIAN_POINT('',(-0.00583674035853046,0.0523600126982779,0.0451584909126088));
#40366=CARTESIAN_POINT('',(-0.00526679477720715,0.0522850757530042,0.043738054600265));
#40367=CARTESIAN_POINT('',(-0.00485551285147822,0.0522505220626225,0.0431001763752942));
#40368=CARTESIAN_POINT('',(-0.00380735353003082,0.0521771690905066,0.0419998055503637));
#40369=CARTESIAN_POINT('',(-0.00316594922103819,0.0521385572455577,0.0415440076504345));
#40370=CARTESIAN_POINT('',(-0.00178519030427026,0.0520656343206208,0.0409163299908685));
#40371=CARTESIAN_POINT('',(-0.00104574457906955,0.0520307824265841,0.0407364425364496));
#40372=CARTESIAN_POINT('',(0.00124883818411648,0.0519181794567874,0.0406285820737455));
#40373=CARTESIAN_POINT('',(0.0027736318720953,0.0518470362547518,0.041159545998454));
#40374=CARTESIAN_POINT('',(0.00450401018390079,0.0517348984409267,0.0426655356739834));
#40375=CARTESIAN_POINT('',(0.00497090043471929,0.0517005528598357,0.0432621087295777));
#40376=CARTESIAN_POINT('',(0.00566742120758123,0.0516268132822675,0.0446157630873064));
#40377=CARTESIAN_POINT('',(0.00588684376001165,0.0515882271308646,0.0453712275482034));
#40378=CARTESIAN_POINT('',(0.0060262886549628,0.0515157768245541,0.0468782624943499));
#40379=CARTESIAN_POINT('',(0.00595354459638783,0.0514805372365184,0.0476384545546751));
#40380=CARTESIAN_POINT('',(0.00551892559300571,0.0514053838650747,0.049107498353668));
#40381=CARTESIAN_POINT('',(0.00516078841230873,0.0513687295160337,0.0497929457474596));
#40382=CARTESIAN_POINT('',(0.0042289612539199,0.0512976948409907,0.050973062149427));
#40383=CARTESIAN_POINT('',(0.00363547045728982,0.0512592942121183,0.0514874847945174));
#40384=CARTESIAN_POINT('',(0.00230967647504479,0.0511847604023482,0.0522466621757463));
#40385=CARTESIAN_POINT('',(0.00159375727545667,0.0511505324137917,0.052491876340922));
#40386=CARTESIAN_POINT('',(8.41419074369142E-5,0.051076450460237,0.0527057063006735));
#40387=CARTESIAN_POINT('',(-0.00070110682816806,0.0510379156376641,0.0526644631841532));
#40388=CARTESIAN_POINT('',(-0.0021669940603479,0.0509659795722588,0.0523024953406513));
#40389=CARTESIAN_POINT('',(-0.00286428837585678,0.050930263582991,0.0519831845300897));
#40390=CARTESIAN_POINT('',(-0.00473183918614788,0.0508174771686901,0.0506435105883454));
#40391=CARTESIAN_POINT('',(-0.00559797051942237,0.0507460599078541,0.049278904374021));
#40392=CARTESIAN_POINT('',(-0.00602010683490445,0.0506346650879708,0.0470292838863863));
#40393=CARTESIAN_POINT('',(-0.00601702730980891,0.0506004639362058,0.0462727235034844));
#40394=CARTESIAN_POINT('',(-0.00572295460377424,0.0505260845379958,0.0447745968412735));
#40395=CARTESIAN_POINT('',(-0.00542594286454709,0.0504876265632931,0.0440470889901856));
#40396=CARTESIAN_POINT('',(-0.00419473858185236,0.0503805547237801,0.0421529761750096));
#40397=CARTESIAN_POINT('',(-0.00285634696512304,0.0503053491211378,0.0412068905161621));
#40398=CARTESIAN_POINT('',(-0.000650935336709183,0.0501971220817964,0.0406815858567029));
#40399=CARTESIAN_POINT('',(0.000134804213528367,0.0501585631732825,0.040647075667539));
#40400=CARTESIAN_POINT('',(0.00164167590883445,0.0500846158610668,0.0408733319392693));
#40401=CARTESIAN_POINT('',(0.00235581443537718,0.0500503507357777,0.0411244497890724));
#40402=CARTESIAN_POINT('',(0.00433579048496438,0.0499384037879682,0.0422802806102534));
#40403=CARTESIAN_POINT('',(0.00532798133591556,0.0498672080706738,0.0435544519204082));
#40404=CARTESIAN_POINT('',(0.00596136440889945,0.0497545214563175,0.0457631125755893));
#40405=CARTESIAN_POINT('',(0.00602782510225254,0.0497194512071264,0.0465227163609867));
#40406=CARTESIAN_POINT('',(0.00587578144387195,0.0496468025108145,0.0480299084881039));
#40407=CARTESIAN_POINT('',(0.00564985425987283,0.0496082027476912,0.0487835511151446));
#40408=CARTESIAN_POINT('',(0.00494259057665489,0.0495346159913582,0.0501304404932439));
#40409=CARTESIAN_POINT('',(0.00447054501904416,0.0495001962123006,0.0507235904043108));
#40410=CARTESIAN_POINT('',(0.00330820369998183,0.0494253590792445,0.0517182568428551));
#40411=CARTESIAN_POINT('',(0.00262492815279643,0.0493871306061523,0.0521031329958861));
#40412=CARTESIAN_POINT('',(0.00120628154563118,0.0493169764065971,0.0525826751353633));
#40413=CARTESIAN_POINT('',(0.000433509776971783,0.049279309413946,0.0526910975554302));
#40414=CARTESIAN_POINT('',(-0.00109522981267062,0.0492042889698804,0.0526064146222846));
#40415=CARTESIAN_POINT('',(-0.00183230736936312,0.049169569897136,0.052420740389839));
#40416=CARTESIAN_POINT('',(-0.00320894594061515,0.0490964658838563,0.0517811134978896));
#40417=CARTESIAN_POINT('',(-0.00384643009871131,0.0490578509322671,0.0513198122705482));
#40418=CARTESIAN_POINT('',(-0.0048846195327673,0.0489846686492892,0.0502116366112216));
#40419=CARTESIAN_POINT('',(-0.00529110431748674,0.0489500038503849,0.0495697919341571));
#40420=CARTESIAN_POINT('',(-0.00612839681505211,0.0488375091393325,0.0474314972485811));
#40421=CARTESIAN_POINT('',(-0.00611457685600949,0.0487663945071744,0.0458171355611411));
#40422=CARTESIAN_POINT('',(-0.00524213722913385,0.0486540901028407,0.0436943384425134));
#40423=CARTESIAN_POINT('',(-0.00482603837135703,0.048619632447345,0.0430603764341383));
#40424=CARTESIAN_POINT('',(-0.00376799594300458,0.0485461160542431,0.0419679429765193));
#40425=CARTESIAN_POINT('',(-0.00312274344804228,0.048507511614782,0.0415176983874283));
#40426=CARTESIAN_POINT('',(-0.00173801800845273,0.0484347769007118,0.040902005168776));
#40427=CARTESIAN_POINT('',(-0.000996149780969905,0.04839977721282,0.0407279060321564));
#40428=CARTESIAN_POINT('',(0.000534394153117021,0.048324668223444,0.0406687901053457));
#40429=CARTESIAN_POINT('',(0.00130116707099782,0.0482876096687883,0.0407890711511285));
#40430=CARTESIAN_POINT('',(0.00271519543873335,0.0482169351067155,0.04129300994584));
#40431=CARTESIAN_POINT('',(0.00339241327145998,0.0481786006320457,0.0416898987444526));
#40432=CARTESIAN_POINT('',(0.00453713172897902,0.0481039284314745,0.0427031030072484));
#40433=CARTESIAN_POINT('',(0.00499890489099844,0.0480696419040328,0.0433031369857737));
#40434=CARTESIAN_POINT('',(0.00568458829322409,0.0479957569051978,0.0446634284610569));
#40435=CARTESIAN_POINT('',(0.00589748451337995,0.0479571886546133,0.0454206299072185));
#40436=CARTESIAN_POINT('',(0.00602435095420808,0.0478849437019996,0.0469273518671414));
#40437=CARTESIAN_POINT('',(0.00594530062534477,0.0478495199335978,0.0476881820089443));
#40438=CARTESIAN_POINT('',(0.00527488903437779,0.0477367582675181,0.0498864194514419));
#40439=CARTESIAN_POINT('',(0.00426061021221676,0.0476654504264648,0.0511439601596007));
#40440=CARTESIAN_POINT('',(0.00226342439943811,0.0475538074551243,0.0522655653621272));
#40441=CARTESIAN_POINT('',(0.00154567488468326,0.047519601418992,0.0525048960399918));
#40442=CARTESIAN_POINT('',(3.34690311347955E-5,0.0474453923415137,0.0527062554034359));
#40443=CARTESIAN_POINT('',(-0.000751201884539185,0.0474068858745274,0.0526582886400806));
#40444=CARTESIAN_POINT('',(-0.00294324433531448,0.0472993149061416,0.0520977989577606));
#40445=CARTESIAN_POINT('',(-0.00426698861795472,0.0472241498935822,0.0511318035742654));
#40446=CARTESIAN_POINT('',(-0.00546935161541402,0.0471163927702915,0.0492136365489639));
#40447=CARTESIAN_POINT('',(-0.00575400166720846,0.0470778700379339,0.0484807246240088));
#40448=CARTESIAN_POINT('',(-0.00602276831052684,0.047003730589497,0.0469795167638521));
#40449=CARTESIAN_POINT('',(-0.00601352874026243,0.0469695142442917,0.0462229028297622));
#40450=CARTESIAN_POINT('',(-0.00555346454973278,0.0468577822995324,0.0439783825107965));
#40451=CARTESIAN_POINT('',(-0.00466460616883524,0.0467865101593862,0.0426295328261682));
#40452=CARTESIAN_POINT('',(-0.00277511890321976,0.046673764575738,0.0413214673628862));
#40453=CARTESIAN_POINT('',(-0.00207521442244891,0.0466384448655614,0.0410146196892824));
#40454=CARTESIAN_POINT('',(-0.000600692686594825,0.0465660850757335,0.0406762519575071));
#40455=CARTESIAN_POINT('',(0.000185450487053797,0.0465275063600478,0.0406484824662403));
#40456=CARTESIAN_POINT('',(0.00168942626526117,0.0464537011603202,0.0408871182772802));
#40457=CARTESIAN_POINT('',(0.00240183301928324,0.0464193837266238,0.0411441618553943));
#40458=CARTESIAN_POINT('',(0.00371586134380875,0.0463446626465699,0.0419260256571976));
#40459=CARTESIAN_POINT('',(0.00429996898030531,0.0463063559145797,0.0424501078491));
#40460=CARTESIAN_POINT('',(0.00521018041629069,0.0462358232364466,0.0436425722548912));
#40461=CARTESIAN_POINT('',(0.00555890724136474,0.0461986014990264,0.0443372252724397));
#40462=CARTESIAN_POINT('',(0.00596876005678161,0.0461235139304544,0.0458129061804159));
#40463=CARTESIAN_POINT('',(0.00602895839985307,0.0460885981214,0.0465719721046274));
#40464=CARTESIAN_POINT('',(0.00586429821692855,0.0460157580652985,0.0480791650102269));
#40465=CARTESIAN_POINT('',(0.00563188957955514,0.0459771489847168,0.048830901324237));
#40466=CARTESIAN_POINT('',(0.00491397942628084,0.0459037223973798,0.0501708996225944));
#40467=CARTESIAN_POINT('',(0.0044367389074107,0.0458692133012517,0.0507606627917028));
#40468=CARTESIAN_POINT('',(0.0026802632123916,0.0457568513841524,0.052238501827766));
#40469=CARTESIAN_POINT('',(0.00114679585513747,0.0456857413559239,0.0527432212211965));
#40470=CARTESIAN_POINT('',(-0.00114460042476067,0.0455732947576852,0.0525970595245437));
#40471=CARTESIAN_POINT('',(-0.00187936400588002,0.0455386934886813,0.052405598071758));
#40472=CARTESIAN_POINT('',(-0.00290863757287697,0.045483735050253,0.0519169443403826));
#40473=CARTESIAN_POINT('',(-0.00323913157385276,0.0454649226491852,0.0517196323634921));
#40474=CARTESIAN_POINT('',(-0.00385599157597277,0.0454273273408982,0.0512652939363906));
#40475=CARTESIAN_POINT('',(-0.00414665186685566,0.045408587811407,0.0510156819102021));
#40476=CARTESIAN_POINT('',(-0.00444424750172291,0.0453898275775236,0.0507748977756262));
#40477=CARTESIAN_POINT('',(-0.00598201094464286,0.0523574403786681,0.0466759019477942));
#40478=CARTESIAN_POINT('',(-0.00598201094464285,0.0523225590011011,0.0459285224420255));
#40479=CARTESIAN_POINT('',(-0.00583674035853046,0.0522844174601826,0.0451584909126088));
#40480=CARTESIAN_POINT('',(-0.00526679477720715,0.0522094805149089,0.043738054600265));
#40481=CARTESIAN_POINT('',(-0.00485551285147822,0.0521749268245272,0.0431001763752942));
#40482=CARTESIAN_POINT('',(-0.00380735353003082,0.0521015738524114,0.0419998055503637));
#40483=CARTESIAN_POINT('',(-0.00316594922103819,0.0520629620074624,0.0415440076504345));
#40484=CARTESIAN_POINT('',(-0.00178519030427026,0.0519900390825255,0.0409163299908685));
#40485=CARTESIAN_POINT('',(-0.00104574457906955,0.0519551871884889,0.0407364425364496));
#40486=CARTESIAN_POINT('',(0.00124883818411648,0.0518425842186922,0.0406285820737455));
#40487=CARTESIAN_POINT('',(0.0027736318720953,0.0517714410166565,0.041159545998454));
#40488=CARTESIAN_POINT('',(0.00450401018390079,0.0516593032028314,0.0426655356739834));
#40489=CARTESIAN_POINT('',(0.00497090043471929,0.0516249576217405,0.0432621087295777));
#40490=CARTESIAN_POINT('',(0.00566742120758123,0.0515512180441723,0.0446157630873064));
#40491=CARTESIAN_POINT('',(0.00588684376001165,0.0515126318927694,0.0453712275482034));
#40492=CARTESIAN_POINT('',(0.0060262886549628,0.0514401815864589,0.0468782624943499));
#40493=CARTESIAN_POINT('',(0.00595354459638783,0.0514049419984231,0.0476384545546751));
#40494=CARTESIAN_POINT('',(0.00551892559300571,0.0513297886269795,0.049107498353668));
#40495=CARTESIAN_POINT('',(0.00516078841230873,0.0512931342779384,0.0497929457474596));
#40496=CARTESIAN_POINT('',(0.0042289612539199,0.0512220996028955,0.050973062149427));
#40497=CARTESIAN_POINT('',(0.00363547045728982,0.0511836989740231,0.0514874847945174));
#40498=CARTESIAN_POINT('',(0.00230967647504479,0.051109165164253,0.0522466621757463));
#40499=CARTESIAN_POINT('',(0.00159375727545667,0.0510749371756964,0.052491876340922));
#40500=CARTESIAN_POINT('',(8.41419074369142E-5,0.0510008552221417,0.0527057063006735));
#40501=CARTESIAN_POINT('',(-0.00070110682816806,0.0509623203995689,0.0526644631841532));
#40502=CARTESIAN_POINT('',(-0.0021669940603479,0.0508903843341635,0.0523024953406513));
#40503=CARTESIAN_POINT('',(-0.00286428837585678,0.0508546683448957,0.0519831845300897));
#40504=CARTESIAN_POINT('',(-0.00473183918614788,0.0507418819305949,0.0506435105883454));
#40505=CARTESIAN_POINT('',(-0.00559797051942237,0.0506704646697589,0.049278904374021));
#40506=CARTESIAN_POINT('',(-0.00602010683490445,0.0505590698498755,0.0470292838863863));
#40507=CARTESIAN_POINT('',(-0.00601702730980891,0.0505248686981106,0.0462727235034844));
#40508=CARTESIAN_POINT('',(-0.00572295460377424,0.0504504892999005,0.0447745968412735));
#40509=CARTESIAN_POINT('',(-0.00542594286454709,0.0504120313251979,0.0440470889901856));
#40510=CARTESIAN_POINT('',(-0.00419473858185236,0.0503049594856848,0.0421529761750096));
#40511=CARTESIAN_POINT('',(-0.00285634696512304,0.0502297538830426,0.0412068905161621));
#40512=CARTESIAN_POINT('',(-0.000650935336709183,0.0501215268437012,0.0406815858567029));
#40513=CARTESIAN_POINT('',(0.000134804213528367,0.0500829679351872,0.040647075667539));
#40514=CARTESIAN_POINT('',(0.00164167590883445,0.0500090206229716,0.0408733319392693));
#40515=CARTESIAN_POINT('',(0.00235581443537718,0.0499747554976825,0.0411244497890724));
#40516=CARTESIAN_POINT('',(0.00433579048496438,0.049862808549873,0.0422802806102534));
#40517=CARTESIAN_POINT('',(0.00532798133591556,0.0497916128325786,0.0435544519204082));
#40518=CARTESIAN_POINT('',(0.00596136440889945,0.0496789262182223,0.0457631125755893));
#40519=CARTESIAN_POINT('',(0.00602782510225254,0.0496438559690311,0.0465227163609867));
#40520=CARTESIAN_POINT('',(0.00587578144387195,0.0495712072727193,0.0480299084881039));
#40521=CARTESIAN_POINT('',(0.00564985425987283,0.049532607509596,0.0487835511151446));
#40522=CARTESIAN_POINT('',(0.00494259057665489,0.0494590207532629,0.0501304404932439));
#40523=CARTESIAN_POINT('',(0.00447054501904416,0.0494246009742053,0.0507235904043108));
#40524=CARTESIAN_POINT('',(0.00330820369998183,0.0493497638411493,0.0517182568428551));
#40525=CARTESIAN_POINT('',(0.00262492815279643,0.049311535368057,0.0521031329958861));
#40526=CARTESIAN_POINT('',(0.00120628154563118,0.0492413811685019,0.0525826751353633));
#40527=CARTESIAN_POINT('',(0.000433509776971783,0.0492037141758507,0.0526910975554302));
#40528=CARTESIAN_POINT('',(-0.00109522981267062,0.0491286937317851,0.0526064146222846));
#40529=CARTESIAN_POINT('',(-0.00183230736936312,0.0490939746590407,0.052420740389839));
#40530=CARTESIAN_POINT('',(-0.00320894594061515,0.0490208706457611,0.0517811134978896));
#40531=CARTESIAN_POINT('',(-0.00384643009871131,0.0489822556941719,0.0513198122705482));
#40532=CARTESIAN_POINT('',(-0.0048846195327673,0.048909073411194,0.0502116366112216));
#40533=CARTESIAN_POINT('',(-0.00529110431748674,0.0488744086122897,0.0495697919341571));
#40534=CARTESIAN_POINT('',(-0.00612839681505211,0.0487619139012373,0.0474314972485811));
#40535=CARTESIAN_POINT('',(-0.00611457685600949,0.0486907992690792,0.0458171355611411));
#40536=CARTESIAN_POINT('',(-0.00524213722913385,0.0485784948647455,0.0436943384425134));
#40537=CARTESIAN_POINT('',(-0.00482603837135703,0.0485440372092498,0.0430603764341383));
#40538=CARTESIAN_POINT('',(-0.00376799594300458,0.0484705208161479,0.0419679429765193));
#40539=CARTESIAN_POINT('',(-0.00312274344804228,0.0484319163766868,0.0415176983874283));
#40540=CARTESIAN_POINT('',(-0.00173801800845273,0.0483591816626165,0.040902005168776));
#40541=CARTESIAN_POINT('',(-0.000996149780969905,0.0483241819747248,0.0407279060321564));
#40542=CARTESIAN_POINT('',(0.000534394153117021,0.0482490729853488,0.0406687901053457));
#40543=CARTESIAN_POINT('',(0.00130116707099782,0.0482120144306931,0.0407890711511285));
#40544=CARTESIAN_POINT('',(0.00271519543873335,0.0481413398686203,0.04129300994584));
#40545=CARTESIAN_POINT('',(0.00339241327145998,0.0481030053939505,0.0416898987444526));
#40546=CARTESIAN_POINT('',(0.00453713172897902,0.0480283331933793,0.0427031030072484));
#40547=CARTESIAN_POINT('',(0.00499890489099844,0.0479940466659375,0.0433031369857737));
#40548=CARTESIAN_POINT('',(0.00568458829322409,0.0479201616671026,0.0446634284610569));
#40549=CARTESIAN_POINT('',(0.00589748451337995,0.047881593416518,0.0454206299072185));
#40550=CARTESIAN_POINT('',(0.00602435095420808,0.0478093484639044,0.0469273518671414));
#40551=CARTESIAN_POINT('',(0.00594530062534477,0.0477739246955026,0.0476881820089443));
#40552=CARTESIAN_POINT('',(0.00527488903437779,0.0476611630294229,0.0498864194514419));
#40553=CARTESIAN_POINT('',(0.00426061021221676,0.0475898551883695,0.0511439601596007));
#40554=CARTESIAN_POINT('',(0.00226342439943811,0.0474782122170291,0.0522655653621272));
#40555=CARTESIAN_POINT('',(0.00154567488468326,0.0474440061808968,0.0525048960399918));
#40556=CARTESIAN_POINT('',(3.34690311347955E-5,0.0473697971034185,0.0527062554034359));
#40557=CARTESIAN_POINT('',(-0.000751201884539185,0.0473312906364322,0.0526582886400806));
#40558=CARTESIAN_POINT('',(-0.00294324433531448,0.0472237196680463,0.0520977989577606));
#40559=CARTESIAN_POINT('',(-0.00426698861795472,0.047148554655487,0.0511318035742654));
#40560=CARTESIAN_POINT('',(-0.00546935161541402,0.0470407975321963,0.0492136365489639));
#40561=CARTESIAN_POINT('',(-0.00575400166720846,0.0470022747998386,0.0484807246240088));
#40562=CARTESIAN_POINT('',(-0.00602276831052684,0.0469281353514017,0.0469795167638521));
#40563=CARTESIAN_POINT('',(-0.00601352874026243,0.0468939190061965,0.0462229028297622));
#40564=CARTESIAN_POINT('',(-0.00555346454973278,0.0467821870614371,0.0439783825107965));
#40565=CARTESIAN_POINT('',(-0.00466460616883524,0.046710914921291,0.0426295328261682));
#40566=CARTESIAN_POINT('',(-0.00277511890321976,0.0465981693376428,0.0413214673628862));
#40567=CARTESIAN_POINT('',(-0.00207521442244891,0.0465628496274662,0.0410146196892824));
#40568=CARTESIAN_POINT('',(-0.000600692686594825,0.0464904898376383,0.0406762519575071));
#40569=CARTESIAN_POINT('',(0.000185450487053797,0.0464519111219526,0.0406484824662403));
#40570=CARTESIAN_POINT('',(0.00168942626526117,0.046378105922225,0.0408871182772802));
#40571=CARTESIAN_POINT('',(0.00240183301928324,0.0463437884885285,0.0411441618553943));
#40572=CARTESIAN_POINT('',(0.00371586134380875,0.0462690674084746,0.0419260256571976));
#40573=CARTESIAN_POINT('',(0.00429996898030531,0.0462307606764845,0.0424501078491));
#40574=CARTESIAN_POINT('',(0.00521018041629069,0.0461602279983514,0.0436425722548912));
#40575=CARTESIAN_POINT('',(0.00555890724136474,0.0461230062609312,0.0443372252724397));
#40576=CARTESIAN_POINT('',(0.00596876005678161,0.0460479186923591,0.0458129061804159));
#40577=CARTESIAN_POINT('',(0.00602895839985307,0.0460130028833048,0.0465719721046274));
#40578=CARTESIAN_POINT('',(0.00586429821692855,0.0459401628272032,0.0480791650102269));
#40579=CARTESIAN_POINT('',(0.00563188957955514,0.0459015537466216,0.048830901324237));
#40580=CARTESIAN_POINT('',(0.00491397942628084,0.0458281271592846,0.0501708996225944));
#40581=CARTESIAN_POINT('',(0.0044367389074107,0.0457936180631564,0.0507606627917028));
#40582=CARTESIAN_POINT('',(0.0026802632123916,0.0456812561460572,0.052238501827766));
#40583=CARTESIAN_POINT('',(0.00114679585513747,0.0456101461178287,0.0527432212211965));
#40584=CARTESIAN_POINT('',(-0.00114460042476067,0.04549769951959,0.0525970595245437));
#40585=CARTESIAN_POINT('',(-0.00187936400588002,0.0454630982505861,0.052405598071758));
#40586=CARTESIAN_POINT('',(-0.00290863757287697,0.0454081398121578,0.0519169443403826));
#40587=CARTESIAN_POINT('',(-0.00323913157385276,0.04538932741109,0.0517196323634921));
#40588=CARTESIAN_POINT('',(-0.00385599157597277,0.0453517321028029,0.0512652939363906));
#40589=CARTESIAN_POINT('',(-0.00414665186685566,0.0453329925733117,0.0510156819102021));
#40590=CARTESIAN_POINT('',(-0.00444424750172291,0.0453142323394283,0.0507748977756262));
#40591=CARTESIAN_POINT('',(-0.00598201094464286,0.0522818451405728,0.0466759019477942));
#40592=CARTESIAN_POINT('',(-0.00598201094464285,0.0522469637630059,0.0459285224420255));
#40593=CARTESIAN_POINT('',(-0.00583674035853046,0.0522088222220874,0.0451584909126088));
#40594=CARTESIAN_POINT('',(-0.00526679477720715,0.0521338852768137,0.043738054600265));
#40595=CARTESIAN_POINT('',(-0.00485551285147822,0.052099331586432,0.0431001763752942));
#40596=CARTESIAN_POINT('',(-0.00380735353003082,0.0520259786143161,0.0419998055503637));
#40597=CARTESIAN_POINT('',(-0.00316594922103819,0.0519873667693672,0.0415440076504345));
#40598=CARTESIAN_POINT('',(-0.00178519030427026,0.0519144438444302,0.0409163299908685));
#40599=CARTESIAN_POINT('',(-0.00104574457906955,0.0518795919503936,0.0407364425364496));
#40600=CARTESIAN_POINT('',(0.00124883818411648,0.051766988980597,0.0406285820737455));
#40601=CARTESIAN_POINT('',(0.0027736318720953,0.0516958457785613,0.041159545998454));
#40602=CARTESIAN_POINT('',(0.00450401018390079,0.0515837079647362,0.0426655356739834));
#40603=CARTESIAN_POINT('',(0.00497090043471929,0.0515493623836453,0.0432621087295777));
#40604=CARTESIAN_POINT('',(0.00566742120758123,0.051475622806077,0.0446157630873064));
#40605=CARTESIAN_POINT('',(0.00588684376001165,0.0514370366546741,0.0453712275482034));
#40606=CARTESIAN_POINT('',(0.0060262886549628,0.0513645863483636,0.0468782624943499));
#40607=CARTESIAN_POINT('',(0.00595354459638783,0.0513293467603279,0.0476384545546751));
#40608=CARTESIAN_POINT('',(0.00551892559300571,0.0512541933888842,0.049107498353668));
#40609=CARTESIAN_POINT('',(0.00516078841230873,0.0512175390398432,0.0497929457474596));
#40610=CARTESIAN_POINT('',(0.0042289612539199,0.0511465043648003,0.050973062149427));
#40611=CARTESIAN_POINT('',(0.00363547045728982,0.0511081037359278,0.0514874847945174));
#40612=CARTESIAN_POINT('',(0.00230967647504479,0.0510335699261577,0.0522466621757463));
#40613=CARTESIAN_POINT('',(0.00159375727545667,0.0509993419376012,0.052491876340922));
#40614=CARTESIAN_POINT('',(8.41419074369142E-5,0.0509252599840465,0.0527057063006735));
#40615=CARTESIAN_POINT('',(-0.00070110682816806,0.0508867251614736,0.0526644631841532));
#40616=CARTESIAN_POINT('',(-0.0021669940603479,0.0508147890960683,0.0523024953406513));
#40617=CARTESIAN_POINT('',(-0.00286428837585678,0.0507790731068005,0.0519831845300897));
#40618=CARTESIAN_POINT('',(-0.00473183918614788,0.0506662866924996,0.0506435105883454));
#40619=CARTESIAN_POINT('',(-0.00559797051942237,0.0505948694316636,0.049278904374021));
#40620=CARTESIAN_POINT('',(-0.00602010683490445,0.0504834746117803,0.0470292838863863));
#40621=CARTESIAN_POINT('',(-0.00601702730980891,0.0504492734600153,0.0462727235034844));
#40622=CARTESIAN_POINT('',(-0.00572295460377424,0.0503748940618053,0.0447745968412735));
#40623=CARTESIAN_POINT('',(-0.00542594286454709,0.0503364360871027,0.0440470889901856));
#40624=CARTESIAN_POINT('',(-0.00419473858185236,0.0502293642475896,0.0421529761750096));
#40625=CARTESIAN_POINT('',(-0.00285634696512304,0.0501541586449474,0.0412068905161621));
#40626=CARTESIAN_POINT('',(-0.000650935336709183,0.0500459316056059,0.0406815858567029));
#40627=CARTESIAN_POINT('',(0.000134804213528367,0.050007372697092,0.040647075667539));
#40628=CARTESIAN_POINT('',(0.00164167590883445,0.0499334253848764,0.0408733319392693));
#40629=CARTESIAN_POINT('',(0.00235581443537718,0.0498991602595873,0.0411244497890724));
#40630=CARTESIAN_POINT('',(0.00433579048496438,0.0497872133117777,0.0422802806102534));
#40631=CARTESIAN_POINT('',(0.00532798133591556,0.0497160175944833,0.0435544519204082));
#40632=CARTESIAN_POINT('',(0.00596136440889945,0.049603330980127,0.0457631125755893));
#40633=CARTESIAN_POINT('',(0.00602782510225254,0.0495682607309359,0.0465227163609867));
#40634=CARTESIAN_POINT('',(0.00587578144387195,0.049495612034624,0.0480299084881039));
#40635=CARTESIAN_POINT('',(0.00564985425987283,0.0494570122715007,0.0487835511151446));
#40636=CARTESIAN_POINT('',(0.00494259057665489,0.0493834255151677,0.0501304404932439));
#40637=CARTESIAN_POINT('',(0.00447054501904416,0.0493490057361101,0.0507235904043108));
#40638=CARTESIAN_POINT('',(0.00330820369998183,0.0492741686030541,0.0517182568428551));
#40639=CARTESIAN_POINT('',(0.00262492815279643,0.0492359401299618,0.0521031329958861));
#40640=CARTESIAN_POINT('',(0.00120628154563118,0.0491657859304066,0.0525826751353633));
#40641=CARTESIAN_POINT('',(0.000433509776971783,0.0491281189377555,0.0526910975554302));
#40642=CARTESIAN_POINT('',(-0.00109522981267062,0.0490530984936899,0.0526064146222846));
#40643=CARTESIAN_POINT('',(-0.00183230736936312,0.0490183794209455,0.052420740389839));
#40644=CARTESIAN_POINT('',(-0.00320894594061515,0.0489452754076659,0.0517811134978896));
#40645=CARTESIAN_POINT('',(-0.00384643009871131,0.0489066604560766,0.0513198122705482));
#40646=CARTESIAN_POINT('',(-0.0048846195327673,0.0488334781730987,0.0502116366112216));
#40647=CARTESIAN_POINT('',(-0.00529110431748674,0.0487988133741944,0.0495697919341571));
#40648=CARTESIAN_POINT('',(-0.00612839681505211,0.0486863186631421,0.0474314972485811));
#40649=CARTESIAN_POINT('',(-0.00611457685600949,0.0486152040309839,0.0458171355611411));
#40650=CARTESIAN_POINT('',(-0.00524213722913385,0.0485028996266502,0.0436943384425134));
#40651=CARTESIAN_POINT('',(-0.00482603837135703,0.0484684419711546,0.0430603764341383));
#40652=CARTESIAN_POINT('',(-0.00376799594300458,0.0483949255780527,0.0419679429765193));
#40653=CARTESIAN_POINT('',(-0.00312274344804228,0.0483563211385916,0.0415176983874283));
#40654=CARTESIAN_POINT('',(-0.00173801800845273,0.0482835864245213,0.040902005168776));
#40655=CARTESIAN_POINT('',(-0.000996149780969905,0.0482485867366295,0.0407279060321564));
#40656=CARTESIAN_POINT('',(0.000534394153117021,0.0481734777472535,0.0406687901053457));
#40657=CARTESIAN_POINT('',(0.00130116707099782,0.0481364191925979,0.0407890711511285));
#40658=CARTESIAN_POINT('',(0.00271519543873335,0.0480657446305251,0.04129300994584));
#40659=CARTESIAN_POINT('',(0.00339241327145998,0.0480274101558552,0.0416898987444526));
#40660=CARTESIAN_POINT('',(0.00453713172897902,0.047952737955284,0.0427031030072484));
#40661=CARTESIAN_POINT('',(0.00499890489099844,0.0479184514278423,0.0433031369857737));
#40662=CARTESIAN_POINT('',(0.00568458829322409,0.0478445664290073,0.0446634284610569));
#40663=CARTESIAN_POINT('',(0.00589748451337995,0.0478059981784228,0.0454206299072185));
#40664=CARTESIAN_POINT('',(0.00602435095420808,0.0477337532258091,0.0469273518671414));
#40665=CARTESIAN_POINT('',(0.00594530062534477,0.0476983294574074,0.0476881820089443));
#40666=CARTESIAN_POINT('',(0.00527488903437779,0.0475855677913276,0.0498864194514419));
#40667=CARTESIAN_POINT('',(0.00426061021221676,0.0475142599502743,0.0511439601596007));
#40668=CARTESIAN_POINT('',(0.00226342439943811,0.0474026169789338,0.0522655653621272));
#40669=CARTESIAN_POINT('',(0.00154567488468326,0.0473684109428015,0.0525048960399918));
#40670=CARTESIAN_POINT('',(3.34690311347955E-5,0.0472942018653233,0.0527062554034359));
#40671=CARTESIAN_POINT('',(-0.000751201884539185,0.047255695398337,0.0526582886400806));
#40672=CARTESIAN_POINT('',(-0.00294324433531448,0.0471481244299511,0.0520977989577606));
#40673=CARTESIAN_POINT('',(-0.00426698861795472,0.0470729594173918,0.0511318035742654));
#40674=CARTESIAN_POINT('',(-0.00546935161541402,0.0469652022941011,0.0492136365489639));
#40675=CARTESIAN_POINT('',(-0.00575400166720846,0.0469266795617434,0.0484807246240088));
#40676=CARTESIAN_POINT('',(-0.00602276831052684,0.0468525401133065,0.0469795167638521));
#40677=CARTESIAN_POINT('',(-0.00601352874026243,0.0468183237681012,0.0462229028297622));
#40678=CARTESIAN_POINT('',(-0.00555346454973278,0.0467065918233419,0.0439783825107965));
#40679=CARTESIAN_POINT('',(-0.00466460616883524,0.0466353196831958,0.0426295328261682));
#40680=CARTESIAN_POINT('',(-0.00277511890321976,0.0465225740995476,0.0413214673628862));
#40681=CARTESIAN_POINT('',(-0.00207521442244891,0.0464872543893709,0.0410146196892824));
#40682=CARTESIAN_POINT('',(-0.000600692686594825,0.046414894599543,0.0406762519575071));
#40683=CARTESIAN_POINT('',(0.000185450487053797,0.0463763158838573,0.0406484824662403));
#40684=CARTESIAN_POINT('',(0.00168942626526117,0.0463025106841298,0.0408871182772802));
#40685=CARTESIAN_POINT('',(0.00240183301928324,0.0462681932504333,0.0411441618553943));
#40686=CARTESIAN_POINT('',(0.00371586134380875,0.0461934721703794,0.0419260256571976));
#40687=CARTESIAN_POINT('',(0.00429996898030531,0.0461551654383893,0.0424501078491));
#40688=CARTESIAN_POINT('',(0.00521018041629069,0.0460846327602562,0.0436425722548912));
#40689=CARTESIAN_POINT('',(0.00555890724136474,0.046047411022836,0.0443372252724397));
#40690=CARTESIAN_POINT('',(0.00596876005678161,0.0459723234542639,0.0458129061804159));
#40691=CARTESIAN_POINT('',(0.00602895839985307,0.0459374076452096,0.0465719721046274));
#40692=CARTESIAN_POINT('',(0.00586429821692855,0.045864567589108,0.0480791650102269));
#40693=CARTESIAN_POINT('',(0.00563188957955514,0.0458259585085263,0.048830901324237));
#40694=CARTESIAN_POINT('',(0.00491397942628084,0.0457525319211894,0.0501708996225944));
#40695=CARTESIAN_POINT('',(0.0044367389074107,0.0457180228250612,0.0507606627917028));
#40696=CARTESIAN_POINT('',(0.0026802632123916,0.0456056609079619,0.052238501827766));
#40697=CARTESIAN_POINT('',(0.00114679585513747,0.0455345508797335,0.0527432212211965));
#40698=CARTESIAN_POINT('',(-0.00114460042476067,0.0454221042814947,0.0525970595245437));
#40699=CARTESIAN_POINT('',(-0.00187936400588002,0.0453875030124909,0.052405598071758));
#40700=CARTESIAN_POINT('',(-0.00290863757287697,0.0453325445740626,0.0519169443403826));
#40701=CARTESIAN_POINT('',(-0.00323913157385276,0.0453137321729947,0.0517196323634921));
#40702=CARTESIAN_POINT('',(-0.00385599157597277,0.0452761368647077,0.0512652939363906));
#40703=CARTESIAN_POINT('',(-0.00414665186685566,0.0452573973352165,0.0510156819102021));
#40704=CARTESIAN_POINT('',(-0.00444424750172291,0.0452386371013331,0.0507748977756262));
#40705=CARTESIAN_POINT('',(-0.00598201094464286,0.0522062499024776,0.0466759019477942));
#40706=CARTESIAN_POINT('',(-0.00598201094464285,0.0521713685249106,0.0459285224420255));
#40707=CARTESIAN_POINT('',(-0.00583674035853046,0.0521332269839922,0.0451584909126088));
#40708=CARTESIAN_POINT('',(-0.00526679477720715,0.0520582900387185,0.043738054600265));
#40709=CARTESIAN_POINT('',(-0.00485551285147822,0.0520237363483368,0.0431001763752942));
#40710=CARTESIAN_POINT('',(-0.00380735353003082,0.0519503833762209,0.0419998055503637));
#40711=CARTESIAN_POINT('',(-0.00316594922103819,0.0519117715312719,0.0415440076504345));
#40712=CARTESIAN_POINT('',(-0.00178519030427026,0.051838848606335,0.0409163299908685));
#40713=CARTESIAN_POINT('',(-0.00104574457906955,0.0518039967122984,0.0407364425364496));
#40714=CARTESIAN_POINT('',(0.00124883818411648,0.0516913937425018,0.0406285820737455));
#40715=CARTESIAN_POINT('',(0.0027736318720953,0.051620250540466,0.041159545998454));
#40716=CARTESIAN_POINT('',(0.00450401018390079,0.0515081127266409,0.0426655356739834));
#40717=CARTESIAN_POINT('',(0.00497090043471929,0.05147376714555,0.0432621087295777));
#40718=CARTESIAN_POINT('',(0.00566742120758123,0.0514000275679818,0.0446157630873064));
#40719=CARTESIAN_POINT('',(0.00588684376001165,0.0513614414165789,0.0453712275482034));
#40720=CARTESIAN_POINT('',(0.0060262886549628,0.0512889911102684,0.0468782624943499));
#40721=CARTESIAN_POINT('',(0.00595354459638783,0.0512537515222327,0.0476384545546751));
#40722=CARTESIAN_POINT('',(0.00551892559300571,0.051178598150789,0.049107498353668));
#40723=CARTESIAN_POINT('',(0.00516078841230873,0.051141943801748,0.0497929457474596));
#40724=CARTESIAN_POINT('',(0.0042289612539199,0.051070909126705,0.050973062149427));
#40725=CARTESIAN_POINT('',(0.00363547045728982,0.0510325084978326,0.0514874847945174));
#40726=CARTESIAN_POINT('',(0.00230967647504479,0.0509579746880625,0.0522466621757463));
#40727=CARTESIAN_POINT('',(0.00159375727545667,0.050923746699506,0.052491876340922));
#40728=CARTESIAN_POINT('',(8.41419074369142E-5,0.0508496647459513,0.0527057063006735));
#40729=CARTESIAN_POINT('',(-0.00070110682816806,0.0508111299233784,0.0526644631841532));
#40730=CARTESIAN_POINT('',(-0.0021669940603479,0.0507391938579731,0.0523024953406513));
#40731=CARTESIAN_POINT('',(-0.00286428837585678,0.0507034778687052,0.0519831845300897));
#40732=CARTESIAN_POINT('',(-0.00473183918614788,0.0505906914544044,0.0506435105883454));
#40733=CARTESIAN_POINT('',(-0.00559797051942237,0.0505192741935684,0.049278904374021));
#40734=CARTESIAN_POINT('',(-0.00602010683490445,0.0504078793736851,0.0470292838863863));
#40735=CARTESIAN_POINT('',(-0.00601702730980891,0.0503736782219201,0.0462727235034844));
#40736=CARTESIAN_POINT('',(-0.00572295460377424,0.0502992988237101,0.0447745968412735));
#40737=CARTESIAN_POINT('',(-0.00542594286454709,0.0502608408490074,0.0440470889901856));
#40738=CARTESIAN_POINT('',(-0.00419473858185236,0.0501537690094944,0.0421529761750096));
#40739=CARTESIAN_POINT('',(-0.00285634696512304,0.0500785634068521,0.0412068905161621));
#40740=CARTESIAN_POINT('',(-0.000650935336709183,0.0499703363675107,0.0406815858567029));
#40741=CARTESIAN_POINT('',(0.000134804213528367,0.0499317774589967,0.040647075667539));
#40742=CARTESIAN_POINT('',(0.00164167590883445,0.0498578301467811,0.0408733319392693));
#40743=CARTESIAN_POINT('',(0.00235581443537718,0.0498235650214921,0.0411244497890724));
#40744=CARTESIAN_POINT('',(0.00433579048496438,0.0497116180736825,0.0422802806102534));
#40745=CARTESIAN_POINT('',(0.00532798133591556,0.0496404223563881,0.0435544519204082));
#40746=CARTESIAN_POINT('',(0.00596136440889945,0.0495277357420318,0.0457631125755893));
#40747=CARTESIAN_POINT('',(0.00602782510225254,0.0494926654928407,0.0465227163609867));
#40748=CARTESIAN_POINT('',(0.00587578144387195,0.0494200167965288,0.0480299084881039));
#40749=CARTESIAN_POINT('',(0.00564985425987283,0.0493814170334055,0.0487835511151446));
#40750=CARTESIAN_POINT('',(0.00494259057665489,0.0493078302770725,0.0501304404932439));
#40751=CARTESIAN_POINT('',(0.00447054501904416,0.0492734104980149,0.0507235904043108));
#40752=CARTESIAN_POINT('',(0.00330820369998183,0.0491985733649588,0.0517182568428551));
#40753=CARTESIAN_POINT('',(0.00262492815279643,0.0491603448918666,0.0521031329958861));
#40754=CARTESIAN_POINT('',(0.00120628154563118,0.0490901906923114,0.0525826751353633));
#40755=CARTESIAN_POINT('',(0.000433509776971783,0.0490525236996602,0.0526910975554302));
#40756=CARTESIAN_POINT('',(-0.00109522981267062,0.0489775032555947,0.0526064146222846));
#40757=CARTESIAN_POINT('',(-0.00183230736936312,0.0489427841828503,0.052420740389839));
#40758=CARTESIAN_POINT('',(-0.00320894594061515,0.0488696801695706,0.0517811134978896));
#40759=CARTESIAN_POINT('',(-0.00384643009871131,0.0488310652179814,0.0513198122705482));
#40760=CARTESIAN_POINT('',(-0.0048846195327673,0.0487578829350035,0.0502116366112216));
#40761=CARTESIAN_POINT('',(-0.00529110431748674,0.0487232181360992,0.0495697919341571));
#40762=CARTESIAN_POINT('',(-0.00612839681505211,0.0486107234250468,0.0474314972485811));
#40763=CARTESIAN_POINT('',(-0.00611457685600949,0.0485396087928887,0.0458171355611411));
#40764=CARTESIAN_POINT('',(-0.00524213722913385,0.048427304388555,0.0436943384425134));
#40765=CARTESIAN_POINT('',(-0.00482603837135703,0.0483928467330594,0.0430603764341383));
#40766=CARTESIAN_POINT('',(-0.00376799594300458,0.0483193303399575,0.0419679429765193));
#40767=CARTESIAN_POINT('',(-0.00312274344804228,0.0482807259004964,0.0415176983874283));
#40768=CARTESIAN_POINT('',(-0.00173801800845273,0.0482079911864261,0.040902005168776));
#40769=CARTESIAN_POINT('',(-0.000996149780969905,0.0481729914985343,0.0407279060321564));
#40770=CARTESIAN_POINT('',(0.000534394153117021,0.0480978825091583,0.0406687901053457));
#40771=CARTESIAN_POINT('',(0.00130116707099782,0.0480608239545026,0.0407890711511285));
#40772=CARTESIAN_POINT('',(0.00271519543873335,0.0479901493924298,0.04129300994584));
#40773=CARTESIAN_POINT('',(0.00339241327145998,0.04795181491776,0.0416898987444526));
#40774=CARTESIAN_POINT('',(0.00453713172897902,0.0478771427171888,0.0427031030072484));
#40775=CARTESIAN_POINT('',(0.00499890489099844,0.0478428561897471,0.0433031369857737));
#40776=CARTESIAN_POINT('',(0.00568458829322409,0.0477689711909121,0.0446634284610569));
#40777=CARTESIAN_POINT('',(0.00589748451337995,0.0477304029403275,0.0454206299072185));
#40778=CARTESIAN_POINT('',(0.00602435095420808,0.0476581579877139,0.0469273518671414));
#40779=CARTESIAN_POINT('',(0.00594530062534477,0.0476227342193121,0.0476881820089443));
#40780=CARTESIAN_POINT('',(0.00527488903437779,0.0475099725532324,0.0498864194514419));
#40781=CARTESIAN_POINT('',(0.00426061021221676,0.0474386647121791,0.0511439601596007));
#40782=CARTESIAN_POINT('',(0.00226342439943811,0.0473270217408386,0.0522655653621272));
#40783=CARTESIAN_POINT('',(0.00154567488468326,0.0472928157047063,0.0525048960399918));
#40784=CARTESIAN_POINT('',(3.34690311347955E-5,0.0472186066272281,0.0527062554034359));
#40785=CARTESIAN_POINT('',(-0.000751201884539185,0.0471801001602418,0.0526582886400806));
#40786=CARTESIAN_POINT('',(-0.00294324433531448,0.0470725291918558,0.0520977989577606));
#40787=CARTESIAN_POINT('',(-0.00426698861795472,0.0469973641792965,0.0511318035742654));
#40788=CARTESIAN_POINT('',(-0.00546935161541402,0.0468896070560058,0.0492136365489639));
#40789=CARTESIAN_POINT('',(-0.00575400166720846,0.0468510843236482,0.0484807246240088));
#40790=CARTESIAN_POINT('',(-0.00602276831052684,0.0467769448752113,0.0469795167638521));
#40791=CARTESIAN_POINT('',(-0.00601352874026243,0.046742728530006,0.0462229028297622));
#40792=CARTESIAN_POINT('',(-0.00555346454973278,0.0466309965852467,0.0439783825107965));
#40793=CARTESIAN_POINT('',(-0.00466460616883524,0.0465597244451005,0.0426295328261682));
#40794=CARTESIAN_POINT('',(-0.00277511890321976,0.0464469788614523,0.0413214673628862));
#40795=CARTESIAN_POINT('',(-0.00207521442244891,0.0464116591512757,0.0410146196892824));
#40796=CARTESIAN_POINT('',(-0.000600692686594825,0.0463392993614478,0.0406762519575071));
#40797=CARTESIAN_POINT('',(0.000185450487053797,0.0463007206457621,0.0406484824662403));
#40798=CARTESIAN_POINT('',(0.00168942626526117,0.0462269154460345,0.0408871182772802));
#40799=CARTESIAN_POINT('',(0.00240183301928324,0.0461925980123381,0.0411441618553943));
#40800=CARTESIAN_POINT('',(0.00371586134380875,0.0461178769322841,0.0419260256571976));
#40801=CARTESIAN_POINT('',(0.00429996898030531,0.046079570200294,0.0424501078491));
#40802=CARTESIAN_POINT('',(0.00521018041629069,0.0460090375221609,0.0436425722548912));
#40803=CARTESIAN_POINT('',(0.00555890724136474,0.0459718157847407,0.0443372252724397));
#40804=CARTESIAN_POINT('',(0.00596876005678161,0.0458967282161687,0.0458129061804159));
#40805=CARTESIAN_POINT('',(0.00602895839985307,0.0458618124071143,0.0465719721046274));
#40806=CARTESIAN_POINT('',(0.00586429821692855,0.0457889723510128,0.0480791650102269));
#40807=CARTESIAN_POINT('',(0.00563188957955514,0.0457503632704311,0.048830901324237));
#40808=CARTESIAN_POINT('',(0.00491397942628084,0.0456769366830941,0.0501708996225944));
#40809=CARTESIAN_POINT('',(0.0044367389074107,0.0456424275869659,0.0507606627917028));
#40810=CARTESIAN_POINT('',(0.0026802632123916,0.0455300656698666,0.052238501827766));
#40811=CARTESIAN_POINT('',(0.00114679585513747,0.0454589556416382,0.0527432212211965));
#40812=CARTESIAN_POINT('',(-0.00114460042476067,0.0453465090433995,0.0525970595245437));
#40813=CARTESIAN_POINT('',(-0.00187936400588002,0.0453119077743956,0.052405598071758));
#40814=CARTESIAN_POINT('',(-0.00290863757287697,0.0452569493359673,0.0519169443403826));
#40815=CARTESIAN_POINT('',(-0.00323913157385276,0.0452381369348995,0.0517196323634921));
#40816=CARTESIAN_POINT('',(-0.00385599157597277,0.0452005416266125,0.0512652939363906));
#40817=CARTESIAN_POINT('',(-0.00414665186685566,0.0451818020971212,0.0510156819102021));
#40818=CARTESIAN_POINT('',(-0.00444424750172291,0.0451630418632379,0.0507748977756262));
#40819=CARTESIAN_POINT('',(-0.00598201094464286,0.0523196427596204,0.0466759019477942));
#40820=CARTESIAN_POINT('',(-0.00376267327913618,0.0453194007129105,0.0513263583486537));
#40821=CARTESIAN_POINT('',(-0.00376267526235003,0.0452627041593186,0.0513263567440401));
#40822=CARTESIAN_POINT('',(-0.00314499195769477,0.0452627041593186,0.0505629349533058));
#40823=CARTESIAN_POINT('',(-0.00598201094464286,0.0523196427596204,0.0466759019477942));
#40824=CARTESIAN_POINT('',(-0.005,0.058,0.0466759019477942));
#40825=CARTESIAN_POINT('',(-0.00240259137190233,0.0451571425815504,0.0522640639622369));
#40826=CARTESIAN_POINT('',(-0.00310564610108304,0.0529999999,0.0533580384747061));
#40827=CARTESIAN_POINT('',(-0.00310564610108304,0.0529999999,0.0533580384747061));
#40828=CARTESIAN_POINT('',(-0.00310564610108304,0.058,0.0533580384747061));
#40829=CARTESIAN_POINT('',(0.000841253532831189,0.058,0.0472165427652498));
#40830=CARTESIAN_POINT('',(-0.00240259137190233,0.058,0.0522640639622369));
#40831=CARTESIAN_POINT('',(-0.00240259137190233,0.0451571425815504,0.0522640639622369));
#40832=CARTESIAN_POINT('',(-0.00240259137190233,0.0529999999,0.0522640639622369));
#40833=CARTESIAN_POINT('',(-0.00240259137190233,0.0529999999,0.0522640639622369));
#40834=CARTESIAN_POINT('',(-0.00240259137190233,0.0451571425815504,0.0522640639622369));
#40835=CARTESIAN_POINT('',(-0.00240259137190233,0.0529999999,0.0522640639622369));
#40836=CARTESIAN_POINT('',(-0.00408509843756471,0.0529999999,0.0511827823273257));
#40837=CARTESIAN_POINT('',(-0.00240259137190233,0.058,0.0522640639622369));
#40838=CARTESIAN_POINT('',(-0.00408509843756471,0.058,0.0511827823273257));
#40839=CARTESIAN_POINT('',(-0.00408509843756471,0.0451571425815504,0.0511827823273257));
#40840=CARTESIAN_POINT('',(-0.00408509843756471,0.0451571425815504,0.0511827823273257));
#40841=CARTESIAN_POINT('',(-0.00478815316674541,0.0529999999,0.052276756839795));
#40842=CARTESIAN_POINT('',(-0.00478815316674541,0.058,0.052276756839795));
#40843=CARTESIAN_POINT('',(-0.00478815316674541,0.0529999999,0.052276756839795));
#40844=CARTESIAN_POINT('',(-0.00408509843756471,0.0529999999,0.0511827823273257));
#40845=CARTESIAN_POINT('',(-0.00408509843756471,0.058,0.0511827823273257));
#40846=CARTESIAN_POINT('',(-0.00504237695912518,0.0451571425815504,0.0500780240211601));
#40847=CARTESIAN_POINT('',(-0.00622527150851907,0.0529999999,0.0506182338611018));
#40848=CARTESIAN_POINT('',(-0.00622527150851907,0.0529999999,0.0506182338611018));
#40849=CARTESIAN_POINT('',(-0.00622527150851907,0.058,0.0506182338611018));
#40850=CARTESIAN_POINT('',(0.000415415013001893,0.058,0.0475855339431487));
#40851=CARTESIAN_POINT('',(-0.00504237695912518,0.058,0.0500780240211601));
#40852=CARTESIAN_POINT('',(-0.00504237695912518,0.0451571425815504,0.0500780240211601));
#40853=CARTESIAN_POINT('',(-0.00504237695912518,0.0529999999,0.0500780240211601));
#40854=CARTESIAN_POINT('',(-0.00504237695912518,0.0529999999,0.0500780240211601));
#40855=CARTESIAN_POINT('',(-0.00504237695912518,0.0451571425815504,0.0500780240211601));
#40856=CARTESIAN_POINT('',(-0.00504237695912518,0.0529999999,0.0500780240211601));
#40857=CARTESIAN_POINT('',(-0.00587320698512898,0.0529999999,0.0482587600304511));
#40858=CARTESIAN_POINT('',(-0.00504237695912518,0.058,0.0500780240211601));
#40859=CARTESIAN_POINT('',(-0.00587320698512898,0.058,0.0482587600304511));
#40860=CARTESIAN_POINT('',(-0.00587320698512898,0.0451571425815504,0.0482587600304511));
#40861=CARTESIAN_POINT('',(-0.00587320698512898,0.0451571425815504,0.0482587600304511));
#40862=CARTESIAN_POINT('',(-0.00705610153452287,0.0529999999,0.0487989698703928));
#40863=CARTESIAN_POINT('',(-0.00705610153452287,0.058,0.0487989698703928));
#40864=CARTESIAN_POINT('',(-0.00705610153452287,0.0529999999,0.0487989698703928));
#40865=CARTESIAN_POINT('',(-0.00587320698512898,0.0529999999,0.0482587600304511));
#40866=CARTESIAN_POINT('',(-0.00587320698512898,0.058,0.0482587600304511));
#40867=CARTESIAN_POINT('',(-0.00608124348955888,0.0451571425815504,0.0468118343600355));
#40868=CARTESIAN_POINT('',(-0.00736841719766689,0.0529999999,0.0466267667202085));
#40869=CARTESIAN_POINT('',(-0.00736841719766689,0.0529999999,0.0466267667202085));
#40870=CARTESIAN_POINT('',(-0.00736841719766689,0.058,0.0466267667202085));
#40871=CARTESIAN_POINT('',(-0.000142314838273275,0.058,0.0476657233896751));
#40872=CARTESIAN_POINT('',(-0.00608124348955888,0.058,0.0468118343600355));
#40873=CARTESIAN_POINT('',(-0.00608124348955888,0.0451571425815504,0.0468118343600355));
#40874=CARTESIAN_POINT('',(-0.00608124348955888,0.0529999999,0.0468118343600355));
#40875=CARTESIAN_POINT('',(-0.00608124348955888,0.0529999999,0.0468118343600355));
#40876=CARTESIAN_POINT('',(-0.00608124348955888,0.0451571425815504,0.0468118343600355));
#40877=CARTESIAN_POINT('',(-0.00608124348955888,0.0529999999,0.0468118343600355));
#40878=CARTESIAN_POINT('',(-0.00579661381301233,0.0529999999,0.0448321914762736));
#40879=CARTESIAN_POINT('',(-0.00608124348955888,0.058,0.0468118343600355));
#40880=CARTESIAN_POINT('',(-0.00579661381301233,0.058,0.0448321914762736));
#40881=CARTESIAN_POINT('',(-0.00579661381301233,0.0451571425815504,0.0448321914762736));
#40882=CARTESIAN_POINT('',(-0.00579661381301233,0.0451571425815504,0.0448321914762736));
#40883=CARTESIAN_POINT('',(-0.00708378752112034,0.0529999999,0.0446471238364467));
#40884=CARTESIAN_POINT('',(-0.00708378752112034,0.058,0.0446471238364467));
#40885=CARTESIAN_POINT('',(-0.00708378752112034,0.0529999999,0.0446471238364467));
#40886=CARTESIAN_POINT('',(-0.00579661381301233,0.0529999999,0.0448321914762736));
#40887=CARTESIAN_POINT('',(-0.00579661381301233,0.058,0.0448321914762736));
#40888=CARTESIAN_POINT('',(-0.00518935818007087,0.0451571425815504,0.0435024871184768));
#40889=CARTESIAN_POINT('',(-0.00617214248930353,0.0529999999,0.0426508996669008));
#40890=CARTESIAN_POINT('',(-0.00617214248930353,0.0529999999,0.0426508996669008));
#40891=CARTESIAN_POINT('',(-0.00617214248930353,0.058,0.0426508996669008));
#40892=CARTESIAN_POINT('',(-0.00065486073394528,0.058,0.0474316515221485));
#40893=CARTESIAN_POINT('',(-0.00518935818007087,0.058,0.0435024871184768));
#40894=CARTESIAN_POINT('',(-0.00518935818007087,0.0451571425815504,0.0435024871184768));
#40895=CARTESIAN_POINT('',(-0.00518935818007087,0.0529999999,0.0435024871184768));
#40896=CARTESIAN_POINT('',(-0.00518935818007087,0.0529999999,0.0435024871184768));
#40897=CARTESIAN_POINT('',(-0.00518935818007087,0.0451571425815504,0.0435024871184768));
#40898=CARTESIAN_POINT('',(-0.00518935818007087,0.0529999999,0.0435024871184768));
#40899=CARTESIAN_POINT('',(-0.0038796367121803,0.0529999999,0.0419909879697682));
#40900=CARTESIAN_POINT('',(-0.00518935818007087,0.058,0.0435024871184768));
#40901=CARTESIAN_POINT('',(-0.0038796367121803,0.058,0.0419909879697682));
#40902=CARTESIAN_POINT('',(-0.0038796367121803,0.0451571425815504,0.0419909879697682));
#40903=CARTESIAN_POINT('',(-0.0038796367121803,0.0451571425815504,0.0419909879697682));
#40904=CARTESIAN_POINT('',(-0.00486242102141297,0.0529999999,0.0411394005181923));
#40905=CARTESIAN_POINT('',(-0.00486242102141297,0.058,0.0411394005181923));
#40906=CARTESIAN_POINT('',(-0.00486242102141297,0.0529999999,0.0411394005181923));
#40907=CARTESIAN_POINT('',(-0.0038796367121803,0.0529999999,0.0419909879697682));
#40908=CARTESIAN_POINT('',(-0.0038796367121803,0.058,0.0419909879697682));
#40909=CARTESIAN_POINT('',(-0.00264988831466312,0.0451571425815504,0.0412006766629487));
#40910=CARTESIAN_POINT('',(-0.00301625615086116,0.0529999999,0.0399529423984696));
#40911=CARTESIAN_POINT('',(-0.00301625615086116,0.0529999999,0.0399529423984696));
#40912=CARTESIAN_POINT('',(-0.00301625615086115,0.058,0.0399529423984696));
#40913=CARTESIAN_POINT('',(-0.000959492973614494,0.058,0.0469576345046356));
#40914=CARTESIAN_POINT('',(-0.00264988831466312,0.058,0.0412006766629487));
#40915=CARTESIAN_POINT('',(-0.00264988831466312,0.0451571425815504,0.0412006766629487));
#40916=CARTESIAN_POINT('',(-0.00264988831466312,0.0529999999,0.0412006766629487));
#40917=CARTESIAN_POINT('',(-0.00264988831466312,0.0529999999,0.0412006766629487));
#40918=CARTESIAN_POINT('',(-0.00264988831466312,0.0451571425815504,0.0412006766629487));
#40919=CARTESIAN_POINT('',(-0.00264988831466312,0.0529999999,0.0412006766629487));
#40920=CARTESIAN_POINT('',(-0.000730902367434127,0.0529999999,0.0406372115492658));
#40921=CARTESIAN_POINT('',(-0.00264988831466312,0.058,0.0412006766629487));
#40922=CARTESIAN_POINT('',(-0.000730902367434127,0.058,0.0406372115492658));
#40923=CARTESIAN_POINT('',(-0.000730902367434127,0.0451571425815504,0.0406372115492658));
#40924=CARTESIAN_POINT('',(-0.000730902367434127,0.0451571425815504,0.0406372115492658));
#40925=CARTESIAN_POINT('',(-0.00109727020363217,0.0529999999,0.0393894772847867));
#40926=CARTESIAN_POINT('',(-0.00109727020363217,0.058,0.0393894772847867));
#40927=CARTESIAN_POINT('',(-0.00109727020363217,0.0529999999,0.0393894772847867));
#40928=CARTESIAN_POINT('',(-0.000730902367434127,0.0529999999,0.0406372115492658));
#40929=CARTESIAN_POINT('',(-0.000730902367434127,0.058,0.0406372115492658));
#40930=CARTESIAN_POINT('',(0.00073090236743404,0.0451571425815504,0.0406372115492658));
#40931=CARTESIAN_POINT('',(0.00109727020363206,0.0529999999,0.0393894772847867));
#40932=CARTESIAN_POINT('',(0.00109727020363206,0.0529999999,0.0393894772847867));
#40933=CARTESIAN_POINT('',(0.00109727020363206,0.058,0.0393894772847867));
#40934=CARTESIAN_POINT('',(-0.000959492973614499,0.058,0.0463941693909528));
#40935=CARTESIAN_POINT('',(0.00073090236743404,0.058,0.0406372115492658));
#40936=CARTESIAN_POINT('',(0.00073090236743404,0.0451571425815504,0.0406372115492658));
#40937=CARTESIAN_POINT('',(0.00073090236743404,0.0529999999,0.0406372115492658));
#40938=CARTESIAN_POINT('',(0.00073090236743404,0.0529999999,0.0406372115492658));
#40939=CARTESIAN_POINT('',(0.00073090236743404,0.0451571425815504,0.0406372115492658));
#40940=CARTESIAN_POINT('',(0.00073090236743404,0.0529999999,0.0406372115492658));
#40941=CARTESIAN_POINT('',(0.00264988831466304,0.0529999999,0.0412006766629486));
#40942=CARTESIAN_POINT('',(0.00073090236743404,0.058,0.0406372115492658));
#40943=CARTESIAN_POINT('',(0.00264988831466304,0.058,0.0412006766629486));
#40944=CARTESIAN_POINT('',(0.00264988831466304,0.0451571425815504,0.0412006766629486));
#40945=CARTESIAN_POINT('',(0.00264988831466304,0.0451571425815504,0.0412006766629486));
#40946=CARTESIAN_POINT('',(0.00301625615086107,0.0529999999,0.0399529423984695));
#40947=CARTESIAN_POINT('',(0.00301625615086107,0.058,0.0399529423984695));
#40948=CARTESIAN_POINT('',(0.00301625615086107,0.0529999999,0.0399529423984695));
#40949=CARTESIAN_POINT('',(0.00264988831466304,0.0529999999,0.0412006766629486));
#40950=CARTESIAN_POINT('',(0.00264988831466304,0.058,0.0412006766629486));
#40951=CARTESIAN_POINT('',(0.00387963671218024,0.0451571425815504,0.0419909879697682));
#40952=CARTESIAN_POINT('',(0.00486242102141288,0.0529999999,0.0411394005181922));
#40953=CARTESIAN_POINT('',(0.00486242102141288,0.0529999999,0.0411394005181922));
#40954=CARTESIAN_POINT('',(0.00486242102141289,0.058,0.0411394005181921));
#40955=CARTESIAN_POINT('',(-0.000654860733945287,0.058,0.0459201523734399));
#40956=CARTESIAN_POINT('',(0.00387963671218024,0.058,0.0419909879697682));
#40957=CARTESIAN_POINT('',(0.00387963671218024,0.0451571425815504,0.0419909879697682));
#40958=CARTESIAN_POINT('',(0.00387963671218024,0.0529999999,0.0419909879697682));
#40959=CARTESIAN_POINT('',(0.00387963671218024,0.0529999999,0.0419909879697682));
#40960=CARTESIAN_POINT('',(0.00387963671218024,0.0451571425815504,0.0419909879697682));
#40961=CARTESIAN_POINT('',(0.00387963671218024,0.0529999999,0.0419909879697682));
#40962=CARTESIAN_POINT('',(0.00518935818007081,0.0529999999,0.0435024871184767));
#40963=CARTESIAN_POINT('',(0.00387963671218024,0.058,0.0419909879697682));
#40964=CARTESIAN_POINT('',(0.00518935818007081,0.058,0.0435024871184767));
#40965=CARTESIAN_POINT('',(0.00518935818007081,0.0451571425815504,0.0435024871184767));
#40966=CARTESIAN_POINT('',(0.00518935818007081,0.0451571425815504,0.0435024871184767));
#40967=CARTESIAN_POINT('',(0.00617214248930346,0.0529999999,0.0426508996669007));
#40968=CARTESIAN_POINT('',(0.00617214248930346,0.058,0.0426508996669007));
#40969=CARTESIAN_POINT('',(0.00617214248930346,0.0529999999,0.0426508996669007));
#40970=CARTESIAN_POINT('',(0.00518935818007081,0.0529999999,0.0435024871184767));
#40971=CARTESIAN_POINT('',(0.00518935818007081,0.058,0.0435024871184767));
#40972=CARTESIAN_POINT('',(0.0057966138130123,0.0451571425815504,0.0448321914762735));
#40973=CARTESIAN_POINT('',(0.00708378752112031,0.0529999999,0.0446471238364465));
#40974=CARTESIAN_POINT('',(0.00708378752112031,0.0529999999,0.0446471238364465));
#40975=CARTESIAN_POINT('',(0.00708378752112031,0.058,0.0446471238364465));
#40976=CARTESIAN_POINT('',(-0.000142314838273289,0.058,0.0456860805059133));
#40977=CARTESIAN_POINT('',(0.0057966138130123,0.058,0.0448321914762735));
#40978=CARTESIAN_POINT('',(0.0057966138130123,0.0451571425815504,0.0448321914762735));
#40979=CARTESIAN_POINT('',(0.0057966138130123,0.0529999999,0.0448321914762735));
#40980=CARTESIAN_POINT('',(0.0057966138130123,0.0529999999,0.0448321914762735));
#40981=CARTESIAN_POINT('',(0.0057966138130123,0.0451571425815504,0.0448321914762735));
#40982=CARTESIAN_POINT('',(0.0057966138130123,0.0529999999,0.0448321914762735));
#40983=CARTESIAN_POINT('',(0.00608124348955888,0.0529999999,0.0468118343600354));
#40984=CARTESIAN_POINT('',(0.0057966138130123,0.058,0.0448321914762735));
#40985=CARTESIAN_POINT('',(0.00608124348955888,0.058,0.0468118343600354));
#40986=CARTESIAN_POINT('',(0.00608124348955888,0.0451571425815504,0.0468118343600354));
#40987=CARTESIAN_POINT('',(0.00608124348955888,0.0451571425815504,0.0468118343600354));
#40988=CARTESIAN_POINT('',(0.00736841719766689,0.0529999999,0.0466267667202084));
#40989=CARTESIAN_POINT('',(0.00736841719766689,0.058,0.0466267667202084));
#40990=CARTESIAN_POINT('',(0.00736841719766689,0.0529999999,0.0466267667202084));
#40991=CARTESIAN_POINT('',(0.00608124348955888,0.0529999999,0.0468118343600354));
#40992=CARTESIAN_POINT('',(0.00608124348955888,0.058,0.0468118343600354));
#40993=CARTESIAN_POINT('',(0.005873206985129,0.0451571425815504,0.048258760030451));
#40994=CARTESIAN_POINT('',(0.0070561015345229,0.0529999999,0.0487989698703927));
#40995=CARTESIAN_POINT('',(0.0070561015345229,0.0529999999,0.0487989698703927));
#40996=CARTESIAN_POINT('',(0.0070561015345229,0.058,0.0487989698703927));
#40997=CARTESIAN_POINT('',(0.000415415013001886,0.058,0.0457662699524397));
#40998=CARTESIAN_POINT('',(0.005873206985129,0.058,0.048258760030451));
#40999=CARTESIAN_POINT('',(0.005873206985129,0.0451571425815504,0.048258760030451));
#41000=CARTESIAN_POINT('',(0.005873206985129,0.0529999999,0.048258760030451));
#41001=CARTESIAN_POINT('',(0.005873206985129,0.0529999999,0.048258760030451));
#41002=CARTESIAN_POINT('',(0.005873206985129,0.0451571425815504,0.048258760030451));
#41003=CARTESIAN_POINT('',(0.005873206985129,0.0529999999,0.048258760030451));
#41004=CARTESIAN_POINT('',(0.00504237695912523,0.0529999999,0.05007802402116));
#41005=CARTESIAN_POINT('',(0.005873206985129,0.058,0.048258760030451));
#41006=CARTESIAN_POINT('',(0.00504237695912523,0.058,0.05007802402116));
#41007=CARTESIAN_POINT('',(0.00504237695912523,0.0451571425815504,0.05007802402116));
#41008=CARTESIAN_POINT('',(0.00504237695912523,0.0451571425815504,0.05007802402116));
#41009=CARTESIAN_POINT('',(0.00622527150851913,0.0529999999,0.0506182338611017));
#41010=CARTESIAN_POINT('',(0.00622527150851913,0.058,0.0506182338611017));
#41011=CARTESIAN_POINT('',(0.00622527150851913,0.0529999999,0.0506182338611017));
#41012=CARTESIAN_POINT('',(0.00504237695912523,0.0529999999,0.05007802402116));
#41013=CARTESIAN_POINT('',(0.00504237695912523,0.058,0.05007802402116));
#41014=CARTESIAN_POINT('',(0.00408509843756477,0.0451571425815504,0.0511827823273257));
#41015=CARTESIAN_POINT('',(0.00478815316674549,0.0529999999,0.0522767568397949));
#41016=CARTESIAN_POINT('',(0.00478815316674549,0.0529999999,0.0522767568397949));
#41017=CARTESIAN_POINT('',(0.00478815316674549,0.058,0.0522767568397949));
#41018=CARTESIAN_POINT('',(0.000841253532831179,0.058,0.0461352611303386));
#41019=CARTESIAN_POINT('',(0.00408509843756477,0.058,0.0511827823273257));
#41020=CARTESIAN_POINT('',(0.00408509843756477,0.0451571425815504,0.0511827823273257));
#41021=CARTESIAN_POINT('',(0.00408509843756477,0.0529999999,0.0511827823273257));
#41022=CARTESIAN_POINT('',(0.00408509843756477,0.0529999999,0.0511827823273257));
#41023=CARTESIAN_POINT('',(0.00408509843756477,0.0451571425815504,0.0511827823273257));
#41024=CARTESIAN_POINT('',(0.00408509843756477,0.0529999999,0.0511827823273257));
#41025=CARTESIAN_POINT('',(0.00240259137190241,0.0529999999,0.0522640639622369));
#41026=CARTESIAN_POINT('',(0.00408509843756477,0.058,0.0511827823273257));
#41027=CARTESIAN_POINT('',(0.00240259137190241,0.058,0.0522640639622369));
#41028=CARTESIAN_POINT('',(0.00240259137190241,0.0451571425815504,0.0522640639622369));
#41029=CARTESIAN_POINT('',(0.00240259137190241,0.0451571425815504,0.0522640639622369));
#41030=CARTESIAN_POINT('',(0.00310564610108313,0.0529999999,0.0533580384747061));
#41031=CARTESIAN_POINT('',(0.00310564610108313,0.058,0.0533580384747061));
#41032=CARTESIAN_POINT('',(0.00310564610108313,0.0529999999,0.0533580384747061));
#41033=CARTESIAN_POINT('',(0.00240259137190241,0.0529999999,0.0522640639622369));
#41034=CARTESIAN_POINT('',(0.00240259137190241,0.058,0.0522640639622369));
#41035=CARTESIAN_POINT('',(0.001,0.0451571425815504,0.0526759019477942));
#41036=CARTESIAN_POINT('',(0.001,0.0529999999,0.0539763119547365));
#41037=CARTESIAN_POINT('',(0.001,0.0529999999,0.0539763119547365));
#41038=CARTESIAN_POINT('',(0.001,0.058,0.0539763119547365));
#41039=CARTESIAN_POINT('',(0.001,0.058,0.0466759019477942));
#41040=CARTESIAN_POINT('',(0.001,0.058,0.0526759019477942));
#41041=CARTESIAN_POINT('',(0.001,0.0451571425815504,0.0526759019477942));
#41042=CARTESIAN_POINT('',(0.001,0.0529999999,0.0526759019477942));
#41043=CARTESIAN_POINT('',(0.001,0.0529999999,0.0526759019477942));
#41044=CARTESIAN_POINT('',(0.001,0.0451571425815504,0.0526759019477942));
#41045=CARTESIAN_POINT('',(0.001,0.0529999999,0.0526759019477942));
#41046=CARTESIAN_POINT('',(-0.001,0.0529999999,0.0526759019477942));
#41047=CARTESIAN_POINT('',(0.001,0.058,0.0526759019477942));
#41048=CARTESIAN_POINT('',(-0.001,0.058,0.0526759019477942));
#41049=CARTESIAN_POINT('',(-0.001,0.0451571425815504,0.0526759019477942));
#41050=CARTESIAN_POINT('',(-0.001,0.0451571425815504,0.0526759019477942));
#41051=CARTESIAN_POINT('',(-0.001,0.0529999999,0.0539763119547365));
#41052=CARTESIAN_POINT('',(-0.001,0.058,0.0539763119547365));
#41053=CARTESIAN_POINT('',(-0.001,0.0529999999,0.0539763119547365));
#41054=CARTESIAN_POINT('',(-0.001,0.0529999999,0.0526759019477942));
#41055=CARTESIAN_POINT('',(-0.001,0.058,0.0526759019477942));
#41056=CARTESIAN_POINT('',(0.,0.058,0.0466759019477942));
#41057=CARTESIAN_POINT('',(0.,0.058,0.0466759019477942));
#41058=CARTESIAN_POINT('',(0.,0.058,0.0466759019477942));
#41059=CARTESIAN_POINT('',(0.,0.058,0.0466759019477942));
#41060=CARTESIAN_POINT('',(0.,0.058,0.0466759019477942));
#41061=CARTESIAN_POINT('',(0.,0.058,0.0466759019477942));
#41062=CARTESIAN_POINT('',(0.,0.058,0.0466759019477942));
#41063=CARTESIAN_POINT('',(0.,0.058,0.0466759019477942));
#41064=CARTESIAN_POINT('',(0.,0.058,0.0466759019477942));
#41065=CARTESIAN_POINT('',(0.,0.058,0.0466759019477942));
#41066=CARTESIAN_POINT('',(0.,0.058,0.0466759019477942));
#41067=CARTESIAN_POINT('',(0.,0.058,0.0466759019477942));
#41068=CARTESIAN_POINT('',(0.,0.058,0.0466759019477942));
#41069=CARTESIAN_POINT('',(0.,0.058,0.0470759019477942));
#41070=CARTESIAN_POINT('',(0.,0.0529999999,0.0466759019477942));
#41071=CARTESIAN_POINT('',(0.,0.0529999999,0.0466759019477942));
#41072=CARTESIAN_POINT('',(0.,0.0529999999,0.0466759019477942));
#41073=CARTESIAN_POINT('',(0.,0.0529999999,0.0466759019477942));
#41074=CARTESIAN_POINT('',(0.,0.0529999999,0.0466759019477942));
#41075=CARTESIAN_POINT('',(0.,0.0529999999,0.0466759019477942));
#41076=CARTESIAN_POINT('',(0.,0.0529999999,0.0466759019477942));
#41077=CARTESIAN_POINT('',(0.,0.0529999999,0.0466759019477942));
#41078=CARTESIAN_POINT('',(0.,0.0529999999,0.0466759019477942));
#41079=CARTESIAN_POINT('',(0.,0.0529999999,0.0466759019477942));
#41080=CARTESIAN_POINT('',(0.,0.0529999999,0.0466759019477942));
#41081=CARTESIAN_POINT('',(0.,0.0529999999,0.0466759019477942));
#41082=CARTESIAN_POINT('',(0.,0.0529999999,0.0466759019477942));
#41083=CARTESIAN_POINT('',(0.,0.0529999999,0.0466759019477942));
#41084=CARTESIAN_POINT('',(0.,0.043,0.0466759019477942));
#41085=CARTESIAN_POINT('',(0.,0.043,0.0466759019477942));
#41086=CARTESIAN_POINT('',(0.,0.043,0.0516759019477942));
#41087=CARTESIAN_POINT('',(0.,0.043,0.0466759019477942));
#41088=CARTESIAN_POINT('',(0.,0.043,0.0470759019477942));
#41089=CARTESIAN_POINT('',(0.,0.0529999999,0.0466759019477942));
#41090=CARTESIAN_POINT('',(0.,0.0529999999,0.0466759019477942));
#41091=CARTESIAN_POINT('',(0.,0.0529999999,0.0466759019477942));
#41092=CARTESIAN_POINT('',(0.,0.0529999999,0.0466759019477942));
#41093=CARTESIAN_POINT('',(0.,0.0529999999,0.0466759019477942));
#41094=CARTESIAN_POINT('',(0.,0.0529999999,0.0466759019477942));
#41095=CARTESIAN_POINT('',(0.,0.0529999999,0.0466759019477942));
#41096=CARTESIAN_POINT('',(0.,0.0529999999,0.0466759019477942));
#41097=CARTESIAN_POINT('',(0.,0.0529999999,0.0466759019477942));
#41098=CARTESIAN_POINT('',(0.,0.0529999999,0.0466759019477942));
#41099=CARTESIAN_POINT('',(0.,0.058,0.0466759019477942));
#41100=CARTESIAN_POINT('',(0.,-0.053,0.0466759019477942));
#41101=CARTESIAN_POINT('',(0.0250669692618323,-6.93889390390723E-18,0.00730221943438869));
#41102=CARTESIAN_POINT('',(0.0259807621135331,-0.015,0.11392908368361));
#41103=CARTESIAN_POINT('',(-0.012852081728299,0.0305608891324553,0.026));
#41104=CARTESIAN_POINT('',(-0.0115,0.0303108891324553,0.026));
#41105=CARTESIAN_POINT('',(-0.0092649160435001,0.0298976219627052,0.026));
#41106=CARTESIAN_POINT('',(-0.0092649160435001,0.0307241563022055,0.026));
#41107=CARTESIAN_POINT('',(-0.00879583654340205,0.0308108891324553,0.026));
#41108=CARTESIAN_POINT('',(-0.00832675704330399,0.0308976219627052,0.026));
#41109=CARTESIAN_POINT('',(-0.0115,0.0303108891324553,0.026));
#41110=CARTESIAN_POINT('',(-0.008326757043304,0.0297241563022054,0.026));
#41111=CARTESIAN_POINT('',(-0.00879583654340205,0.0298108891324554,0.026));
#41112=CARTESIAN_POINT('',(-0.0115,0.0303108891324553,0.026));
#41113=CARTESIAN_POINT('',(-0.0115,0.0303108891324553,0.021));
#41114=CARTESIAN_POINT('',(-0.008326757043304,0.0308976219627052,0.021));
#41115=CARTESIAN_POINT('',(-0.00832675704330399,0.0297241563022054,0.021));
#41116=CARTESIAN_POINT('',(-0.008326757043304,0.0297241563022054,0.026));
#41117=CARTESIAN_POINT('',(-0.008326757043304,0.0308976219627052,0.026));
#41118=CARTESIAN_POINT('',(-0.0115,0.0303108891324553,0.026));
#41119=CARTESIAN_POINT('',(-0.0115,0.0303108891324553,0.021));
#41120=CARTESIAN_POINT('',(-0.0092649160435001,0.0298976219627052,0.021));
#41121=CARTESIAN_POINT('',(-0.0092649160435001,0.0307241563022055,0.021));
#41122=CARTESIAN_POINT('',(-0.0092649160435001,0.0307241563022055,0.026));
#41123=CARTESIAN_POINT('',(-0.0092649160435001,0.0298976219627052,0.026));
#41124=CARTESIAN_POINT('',(-0.012852081728299,0.0305608891324553,0.026));
#41125=CARTESIAN_POINT('',(-0.014204163456598,0.0308108891324553,0.026));
#41126=CARTESIAN_POINT('',(-0.0146732429566961,0.0308976219627052,0.026));
#41127=CARTESIAN_POINT('',(-0.0137350839565,0.0307241563022055,0.026));
#41128=CARTESIAN_POINT('',(-0.0115,0.0303108891324553,0.026));
#41129=CARTESIAN_POINT('',(-0.0137350839565,0.0298976219627052,0.026));
#41130=CARTESIAN_POINT('',(-0.014204163456598,0.0298108891324554,0.026));
#41131=CARTESIAN_POINT('',(-0.0146732429566961,0.0297241563022054,0.026));
#41132=CARTESIAN_POINT('',(-0.0115,0.0303108891324553,0.026));
#41133=CARTESIAN_POINT('',(-0.014204163456598,0.0298108891324554,0.026));
#41134=CARTESIAN_POINT('',(-0.014204163456598,0.0298108891324554,0.021));
#41135=CARTESIAN_POINT('',(-0.0137350839565,0.0298976219627052,0.021));
#41136=CARTESIAN_POINT('',(-0.0146732429566961,0.0297241563022054,0.021));
#41137=CARTESIAN_POINT('',(-0.0146732429566961,0.0297241563022054,0.026));
#41138=CARTESIAN_POINT('',(-0.0137350839565,0.0298976219627052,0.026));
#41139=CARTESIAN_POINT('',(-0.014204163456598,0.0308108891324553,0.026));
#41140=CARTESIAN_POINT('',(-0.014204163456598,0.0308108891324553,0.021));
#41141=CARTESIAN_POINT('',(-0.0146732429566961,0.0308976219627052,0.021));
#41142=CARTESIAN_POINT('',(-0.0137350839565,0.0307241563022055,0.021));
#41143=CARTESIAN_POINT('',(-0.0137350839565,0.0307241563022055,0.026));
#41144=CARTESIAN_POINT('',(-0.0146732429566961,0.0308976219627052,0.026));
#41145=CARTESIAN_POINT('',(-0.0115,0.0303108891324553,0.031));
#41146=CARTESIAN_POINT('',(-0.0115,0.0328108891324553,0.031));
#41147=CARTESIAN_POINT('',(-0.0099006579232147,0.0328108891324553,0.031));
#41148=CARTESIAN_POINT('',(-0.0115,0.0328108891324553,0.031));
#41149=CARTESIAN_POINT('',(-0.0175,0.0303108891324553,0.031));
#41150=CARTESIAN_POINT('',(-0.0101875,0.0335554759705597,0.031));
#41151=CARTESIAN_POINT('',(-0.0115,0.0303108891324553,0.031));
#41152=CARTESIAN_POINT('',(-0.0101875,0.027066302294351,0.031));
#41153=CARTESIAN_POINT('',(-0.0175,0.0303108891324553,0.031));
#41154=CARTESIAN_POINT('',(-0.0099006579232147,0.0278108891324554,0.031));
#41155=CARTESIAN_POINT('',(-0.0115,0.0278108891324554,0.031));
#41156=CARTESIAN_POINT('',(-0.0115,0.0278108891324554,0.031));
#41157=CARTESIAN_POINT('',(-0.0115,0.0303108891324553,0.031));
#41158=CARTESIAN_POINT('',(-0.00678810118750004,0.0303108891324553,0.0216562499979516));
#41159=CARTESIAN_POINT('',(-0.00678810118750004,0.0347479028993611,0.0217499999979516));
#41160=CARTESIAN_POINT('',(-0.00992554371029717,0.0378853454221582,0.0218437499979516));
#41161=CARTESIAN_POINT('',(-0.0130629862330943,0.0410227879449553,0.0219374999979516));
#41162=CARTESIAN_POINT('',(-0.0175,0.0410227879449554,0.0220312499979516));
#41163=CARTESIAN_POINT('',(-0.0219370137669058,0.0410227879449553,0.0221249999979516));
#41164=CARTESIAN_POINT('',(-0.025074456289703,0.0378853454221582,0.0222187499979516));
#41165=CARTESIAN_POINT('',(-0.0282118988125001,0.0347479028993611,0.0223124999979516));
#41166=CARTESIAN_POINT('',(-0.0282118988125,0.0303108891324553,0.0224062499979516));
#41167=CARTESIAN_POINT('',(-0.0282118988125001,0.0258738753655496,0.0224999999979516));
#41168=CARTESIAN_POINT('',(-0.025074456289703,0.0227364328427525,0.0225937499979516));
#41169=CARTESIAN_POINT('',(-0.0219370137669058,0.0195989903199553,0.0226874999979516));
#41170=CARTESIAN_POINT('',(-0.0175,0.0195989903199554,0.0227812499979516));
#41171=CARTESIAN_POINT('',(-0.0130629862330943,0.0195989903199553,0.0228749999979516));
#41172=CARTESIAN_POINT('',(-0.00992554371029717,0.0227364328427525,0.0229687499979516));
#41173=CARTESIAN_POINT('',(-0.00678810118750004,0.0258738753655496,0.0230624999979516));
#41174=CARTESIAN_POINT('',(-0.00678810118750004,0.0303108891324553,0.0231562499979516));
#41175=CARTESIAN_POINT('',(-0.00678810118750004,0.0347479028993611,0.0232499999979516));
#41176=CARTESIAN_POINT('',(-0.00992554371029717,0.0378853454221582,0.0233437499979516));
#41177=CARTESIAN_POINT('',(-0.0130629862330943,0.0410227879449553,0.0234374999979516));
#41178=CARTESIAN_POINT('',(-0.0175,0.0410227879449554,0.0235312499979516));
#41179=CARTESIAN_POINT('',(-0.0219370137669058,0.0410227879449553,0.0236249999979516));
#41180=CARTESIAN_POINT('',(-0.025074456289703,0.0378853454221582,0.0237187499979516));
#41181=CARTESIAN_POINT('',(-0.0282118988125001,0.0347479028993611,0.0238124999979516));
#41182=CARTESIAN_POINT('',(-0.0282118988125,0.0303108891324553,0.0239062499979516));
#41183=CARTESIAN_POINT('',(-0.0282118988125001,0.0258738753655496,0.0239999999979516));
#41184=CARTESIAN_POINT('',(-0.025074456289703,0.0227364328427525,0.0240937499979516));
#41185=CARTESIAN_POINT('',(-0.0219370137669058,0.0195989903199553,0.0241874999979516));
#41186=CARTESIAN_POINT('',(-0.0175,0.0195989903199554,0.0242812499979516));
#41187=CARTESIAN_POINT('',(-0.0130629862330943,0.0195989903199553,0.0243749999979516));
#41188=CARTESIAN_POINT('',(-0.00992554371029717,0.0227364328427525,0.0244687499979516));
#41189=CARTESIAN_POINT('',(-0.00678810118750004,0.0258738753655496,0.0245624999979516));
#41190=CARTESIAN_POINT('',(-0.00678810118750004,0.0303108891324553,0.0246562499979516));
#41191=CARTESIAN_POINT('',(-0.00678810118750004,0.0347479028993611,0.0247499999979516));
#41192=CARTESIAN_POINT('',(-0.00992554371029717,0.0378853454221582,0.0248437499979516));
#41193=CARTESIAN_POINT('',(-0.0130629862330943,0.0410227879449553,0.0249374999979516));
#41194=CARTESIAN_POINT('',(-0.0175,0.0410227879449554,0.0250312499979516));
#41195=CARTESIAN_POINT('',(-0.0219370137669058,0.0410227879449553,0.0251249999979516));
#41196=CARTESIAN_POINT('',(-0.025074456289703,0.0378853454221582,0.0252187499979516));
#41197=CARTESIAN_POINT('',(-0.0282118988125001,0.0347479028993611,0.0253124999979516));
#41198=CARTESIAN_POINT('',(-0.0282118988125,0.0303108891324553,0.0254062499979516));
#41199=CARTESIAN_POINT('',(-0.0282118988125001,0.0258738753655496,0.0254999999979516));
#41200=CARTESIAN_POINT('',(-0.025074456289703,0.0227364328427525,0.0255937499979516));
#41201=CARTESIAN_POINT('',(-0.0219370137669058,0.0195989903199553,0.0256874999979516));
#41202=CARTESIAN_POINT('',(-0.0175,0.0195989903199554,0.0257812499979516));
#41203=CARTESIAN_POINT('',(-0.0130629862330943,0.0195989903199553,0.0258749999979516));
#41204=CARTESIAN_POINT('',(-0.00992554371029717,0.0227364328427525,0.0259687499979516));
#41205=CARTESIAN_POINT('',(-0.00678810118750004,0.0258738753655496,0.0260624999979516));
#41206=CARTESIAN_POINT('',(-0.00678810118750004,0.0303108891324553,0.0261562499979516));
#41207=CARTESIAN_POINT('',(-0.00678810118750004,0.0347479028993611,0.0262499999979516));
#41208=CARTESIAN_POINT('',(-0.00992554371029717,0.0378853454221582,0.0263437499979516));
#41209=CARTESIAN_POINT('',(-0.0130629862330943,0.0410227879449553,0.0264374999979516));
#41210=CARTESIAN_POINT('',(-0.0175,0.0410227879449554,0.0265312499979516));
#41211=CARTESIAN_POINT('',(-0.0219370137669058,0.0410227879449553,0.0266249999979516));
#41212=CARTESIAN_POINT('',(-0.025074456289703,0.0378853454221582,0.0267187499979516));
#41213=CARTESIAN_POINT('',(-0.0282118988125001,0.0347479028993611,0.0268124999979516));
#41214=CARTESIAN_POINT('',(-0.0282118988125,0.0303108891324553,0.0269062499979516));
#41215=CARTESIAN_POINT('',(-0.0282118988125001,0.0258738753655496,0.0269999999979516));
#41216=CARTESIAN_POINT('',(-0.025074456289703,0.0227364328427525,0.0270937499979516));
#41217=CARTESIAN_POINT('',(-0.0219370137669058,0.0195989903199553,0.0271874999979516));
#41218=CARTESIAN_POINT('',(-0.0175,0.0195989903199554,0.0272812499979516));
#41219=CARTESIAN_POINT('',(-0.0130629862330943,0.0195989903199553,0.0273749999979516));
#41220=CARTESIAN_POINT('',(-0.00992554371029717,0.0227364328427525,0.0274687499979516));
#41221=CARTESIAN_POINT('',(-0.00678810118750004,0.0258738753655496,0.0275624999979516));
#41222=CARTESIAN_POINT('',(-0.00678810118750004,0.0303108891324553,0.0276562499979516));
#41223=CARTESIAN_POINT('',(-0.0076,0.0303108891324553,0.0221249999959033));
#41224=CARTESIAN_POINT('',(-0.00760000000000004,0.0344116033999489,0.0222187499959032));
#41225=CARTESIAN_POINT('',(-0.0104996428662532,0.0373112462662021,0.0223124999959033));
#41226=CARTESIAN_POINT('',(-0.0133992857325064,0.0402108891324553,0.0224062499959032));
#41227=CARTESIAN_POINT('',(-0.0175,0.0402108891324554,0.0224999999959033));
#41228=CARTESIAN_POINT('',(-0.0216007142674937,0.0402108891324553,0.0225937499959032));
#41229=CARTESIAN_POINT('',(-0.0245003571337469,0.0373112462662021,0.0226874999959033));
#41230=CARTESIAN_POINT('',(-0.0274,0.0344116033999489,0.0227812499959032));
#41231=CARTESIAN_POINT('',(-0.0274,0.0303108891324553,0.0228749999959033));
#41232=CARTESIAN_POINT('',(-0.0274,0.0262101748649617,0.0229687499959032));
#41233=CARTESIAN_POINT('',(-0.0245003571337469,0.0233105319987085,0.0230624999959032));
#41234=CARTESIAN_POINT('',(-0.0216007142674937,0.0204108891324553,0.0231562499959032));
#41235=CARTESIAN_POINT('',(-0.0175,0.0204108891324553,0.0232499999959032));
#41236=CARTESIAN_POINT('',(-0.0133992857325064,0.0204108891324553,0.0233437499959032));
#41237=CARTESIAN_POINT('',(-0.0104996428662532,0.0233105319987085,0.0234374999959032));
#41238=CARTESIAN_POINT('',(-0.00760000000000004,0.0262101748649617,0.0235312499959032));
#41239=CARTESIAN_POINT('',(-0.0076,0.0303108891324553,0.0236249999959032));
#41240=CARTESIAN_POINT('',(-0.00760000000000004,0.0344116033999489,0.0237187499959032));
#41241=CARTESIAN_POINT('',(-0.0104996428662532,0.0373112462662021,0.0238124999959032));
#41242=CARTESIAN_POINT('',(-0.0133992857325064,0.0402108891324553,0.0239062499959032));
#41243=CARTESIAN_POINT('',(-0.0175,0.0402108891324554,0.0239999999959032));
#41244=CARTESIAN_POINT('',(-0.0216007142674937,0.0402108891324553,0.0240937499959032));
#41245=CARTESIAN_POINT('',(-0.0245003571337469,0.0373112462662021,0.0241874999959032));
#41246=CARTESIAN_POINT('',(-0.0274,0.0344116033999489,0.0242812499959032));
#41247=CARTESIAN_POINT('',(-0.0274,0.0303108891324553,0.0243749999959032));
#41248=CARTESIAN_POINT('',(-0.0274,0.0262101748649617,0.0244687499959032));
#41249=CARTESIAN_POINT('',(-0.0245003571337469,0.0233105319987085,0.0245624999959033));
#41250=CARTESIAN_POINT('',(-0.0216007142674937,0.0204108891324553,0.0246562499959032));
#41251=CARTESIAN_POINT('',(-0.0175,0.0204108891324553,0.0247499999959033));
#41252=CARTESIAN_POINT('',(-0.0133992857325064,0.0204108891324553,0.0248437499959032));
#41253=CARTESIAN_POINT('',(-0.0104996428662532,0.0233105319987085,0.0249374999959033));
#41254=CARTESIAN_POINT('',(-0.00760000000000004,0.0262101748649617,0.0250312499959032));
#41255=CARTESIAN_POINT('',(-0.0076,0.0303108891324553,0.0251249999959033));
#41256=CARTESIAN_POINT('',(-0.00760000000000004,0.0344116033999489,0.0252187499959032));
#41257=CARTESIAN_POINT('',(-0.0104996428662532,0.0373112462662021,0.0253124999959033));
#41258=CARTESIAN_POINT('',(-0.0133992857325064,0.0402108891324553,0.0254062499959032));
#41259=CARTESIAN_POINT('',(-0.0175,0.0402108891324554,0.0254999999959033));
#41260=CARTESIAN_POINT('',(-0.0216007142674937,0.0402108891324553,0.0255937499959032));
#41261=CARTESIAN_POINT('',(-0.0245003571337469,0.0373112462662021,0.0256874999959033));
#41262=CARTESIAN_POINT('',(-0.0274,0.0344116033999489,0.0257812499959032));
#41263=CARTESIAN_POINT('',(-0.0274,0.0303108891324553,0.0258749999959033));
#41264=CARTESIAN_POINT('',(-0.0274,0.0262101748649617,0.0259687499959032));
#41265=CARTESIAN_POINT('',(-0.0245003571337469,0.0233105319987085,0.0260624999959033));
#41266=CARTESIAN_POINT('',(-0.0216007142674937,0.0204108891324553,0.0261562499959032));
#41267=CARTESIAN_POINT('',(-0.0175,0.0204108891324553,0.0262499999959033));
#41268=CARTESIAN_POINT('',(-0.0133992857325064,0.0204108891324553,0.0263437499959032));
#41269=CARTESIAN_POINT('',(-0.0104996428662532,0.0233105319987085,0.0264374999959033));
#41270=CARTESIAN_POINT('',(-0.00760000000000004,0.0262101748649617,0.0265312499959032));
#41271=CARTESIAN_POINT('',(-0.0076,0.0303108891324553,0.0266249999959033));
#41272=CARTESIAN_POINT('',(-0.00760000000000004,0.0344116033999489,0.0267187499959032));
#41273=CARTESIAN_POINT('',(-0.0104996428662532,0.0373112462662021,0.0268124999959033));
#41274=CARTESIAN_POINT('',(-0.0133992857325064,0.0402108891324553,0.0269062499959032));
#41275=CARTESIAN_POINT('',(-0.0175,0.0402108891324554,0.0269999999959032));
#41276=CARTESIAN_POINT('',(-0.0216007142674937,0.0402108891324553,0.0270937499959032));
#41277=CARTESIAN_POINT('',(-0.0245003571337469,0.0373112462662021,0.0271874999959032));
#41278=CARTESIAN_POINT('',(-0.0274,0.0344116033999489,0.0272812499959032));
#41279=CARTESIAN_POINT('',(-0.0274,0.0303108891324553,0.0273749999959032));
#41280=CARTESIAN_POINT('',(-0.0274,0.0262101748649617,0.0274687499959032));
#41281=CARTESIAN_POINT('',(-0.0245003571337469,0.0233105319987085,0.0275624999959032));
#41282=CARTESIAN_POINT('',(-0.0216007142674937,0.0204108891324553,0.0276562499959032));
#41283=CARTESIAN_POINT('',(-0.0175,0.0204108891324553,0.0277499999959032));
#41284=CARTESIAN_POINT('',(-0.0133992857325064,0.0204108891324553,0.0278437499959032));
#41285=CARTESIAN_POINT('',(-0.0104996428662532,0.0233105319987085,0.0279374999959032));
#41286=CARTESIAN_POINT('',(-0.00760000000000004,0.0262101748649617,0.0280312499959032));
#41287=CARTESIAN_POINT('',(-0.0076,0.0303108891324553,0.0281249999959032));
#41288=CARTESIAN_POINT('',(-0.00719405059375004,0.0303108891324553,0.0218906249969274));
#41289=CARTESIAN_POINT('',(-0.00678810118750004,0.0303108891324553,0.0216562499979516));
#41290=CARTESIAN_POINT('',(-0.0076,0.0303108891324553,0.0221249999959033));
#41291=CARTESIAN_POINT('',(-0.00678810118750004,0.0303108891324553,0.0216562499979516));
#41292=CARTESIAN_POINT('',(-0.00678810118750004,0.0347479028993611,0.0217499999979516));
#41293=CARTESIAN_POINT('',(-0.00992554371029717,0.0378853454221582,0.0218437499979516));
#41294=CARTESIAN_POINT('',(-0.0130629862330943,0.0410227879449553,0.0219374999979516));
#41295=CARTESIAN_POINT('',(-0.0175,0.0410227879449554,0.0220312499979516));
#41296=CARTESIAN_POINT('',(-0.0219370137669058,0.0410227879449553,0.0221249999979516));
#41297=CARTESIAN_POINT('',(-0.025074456289703,0.0378853454221582,0.0222187499979516));
#41298=CARTESIAN_POINT('',(-0.0282118988125001,0.0347479028993611,0.0223124999979516));
#41299=CARTESIAN_POINT('',(-0.0282118988125,0.0303108891324553,0.0224062499979516));
#41300=CARTESIAN_POINT('',(-0.0282118988125001,0.0258738753655496,0.0224999999979516));
#41301=CARTESIAN_POINT('',(-0.025074456289703,0.0227364328427525,0.0225937499979516));
#41302=CARTESIAN_POINT('',(-0.0219370137669058,0.0195989903199553,0.0226874999979516));
#41303=CARTESIAN_POINT('',(-0.0175,0.0195989903199554,0.0227812499979516));
#41304=CARTESIAN_POINT('',(-0.0130629862330943,0.0195989903199553,0.0228749999979516));
#41305=CARTESIAN_POINT('',(-0.00992554371029717,0.0227364328427525,0.0229687499979516));
#41306=CARTESIAN_POINT('',(-0.00678810118750004,0.0258738753655496,0.0230624999979516));
#41307=CARTESIAN_POINT('',(-0.00678810118750004,0.0303108891324553,0.0231562499979516));
#41308=CARTESIAN_POINT('',(-0.00678810118750004,0.0347479028993611,0.0232499999979516));
#41309=CARTESIAN_POINT('',(-0.00992554371029717,0.0378853454221582,0.0233437499979516));
#41310=CARTESIAN_POINT('',(-0.0130629862330943,0.0410227879449553,0.0234374999979516));
#41311=CARTESIAN_POINT('',(-0.0175,0.0410227879449554,0.0235312499979516));
#41312=CARTESIAN_POINT('',(-0.0219370137669058,0.0410227879449553,0.0236249999979516));
#41313=CARTESIAN_POINT('',(-0.025074456289703,0.0378853454221582,0.0237187499979516));
#41314=CARTESIAN_POINT('',(-0.0282118988125001,0.0347479028993611,0.0238124999979516));
#41315=CARTESIAN_POINT('',(-0.0282118988125,0.0303108891324553,0.0239062499979516));
#41316=CARTESIAN_POINT('',(-0.0282118988125001,0.0258738753655496,0.0239999999979516));
#41317=CARTESIAN_POINT('',(-0.025074456289703,0.0227364328427525,0.0240937499979516));
#41318=CARTESIAN_POINT('',(-0.0219370137669058,0.0195989903199553,0.0241874999979516));
#41319=CARTESIAN_POINT('',(-0.0175,0.0195989903199554,0.0242812499979516));
#41320=CARTESIAN_POINT('',(-0.0130629862330943,0.0195989903199553,0.0243749999979516));
#41321=CARTESIAN_POINT('',(-0.00992554371029717,0.0227364328427525,0.0244687499979516));
#41322=CARTESIAN_POINT('',(-0.00678810118750004,0.0258738753655496,0.0245624999979516));
#41323=CARTESIAN_POINT('',(-0.00678810118750004,0.0303108891324553,0.0246562499979516));
#41324=CARTESIAN_POINT('',(-0.00678810118750004,0.0347479028993611,0.0247499999979516));
#41325=CARTESIAN_POINT('',(-0.00992554371029717,0.0378853454221582,0.0248437499979516));
#41326=CARTESIAN_POINT('',(-0.0130629862330943,0.0410227879449553,0.0249374999979516));
#41327=CARTESIAN_POINT('',(-0.0175,0.0410227879449554,0.0250312499979516));
#41328=CARTESIAN_POINT('',(-0.0219370137669058,0.0410227879449553,0.0251249999979516));
#41329=CARTESIAN_POINT('',(-0.025074456289703,0.0378853454221582,0.0252187499979516));
#41330=CARTESIAN_POINT('',(-0.0282118988125001,0.0347479028993611,0.0253124999979516));
#41331=CARTESIAN_POINT('',(-0.0282118988125,0.0303108891324553,0.0254062499979516));
#41332=CARTESIAN_POINT('',(-0.0282118988125001,0.0258738753655496,0.0254999999979516));
#41333=CARTESIAN_POINT('',(-0.025074456289703,0.0227364328427525,0.0255937499979516));
#41334=CARTESIAN_POINT('',(-0.0219370137669058,0.0195989903199553,0.0256874999979516));
#41335=CARTESIAN_POINT('',(-0.0175,0.0195989903199554,0.0257812499979516));
#41336=CARTESIAN_POINT('',(-0.0130629862330943,0.0195989903199553,0.0258749999979516));
#41337=CARTESIAN_POINT('',(-0.00992554371029717,0.0227364328427525,0.0259687499979516));
#41338=CARTESIAN_POINT('',(-0.00678810118750004,0.0258738753655496,0.0260624999979516));
#41339=CARTESIAN_POINT('',(-0.00678810118750004,0.0303108891324553,0.0261562499979516));
#41340=CARTESIAN_POINT('',(-0.00678810118750004,0.0347479028993611,0.0262499999979516));
#41341=CARTESIAN_POINT('',(-0.00992554371029717,0.0378853454221582,0.0263437499979516));
#41342=CARTESIAN_POINT('',(-0.0130629862330943,0.0410227879449553,0.0264374999979516));
#41343=CARTESIAN_POINT('',(-0.0175,0.0410227879449554,0.0265312499979516));
#41344=CARTESIAN_POINT('',(-0.0219370137669058,0.0410227879449553,0.0266249999979516));
#41345=CARTESIAN_POINT('',(-0.025074456289703,0.0378853454221582,0.0267187499979516));
#41346=CARTESIAN_POINT('',(-0.0282118988125001,0.0347479028993611,0.0268124999979516));
#41347=CARTESIAN_POINT('',(-0.0282118988125,0.0303108891324553,0.0269062499979516));
#41348=CARTESIAN_POINT('',(-0.0282118988125001,0.0258738753655496,0.0269999999979516));
#41349=CARTESIAN_POINT('',(-0.025074456289703,0.0227364328427525,0.0270937499979516));
#41350=CARTESIAN_POINT('',(-0.0219370137669058,0.0195989903199553,0.0271874999979516));
#41351=CARTESIAN_POINT('',(-0.0175,0.0195989903199554,0.0272812499979516));
#41352=CARTESIAN_POINT('',(-0.0130629862330943,0.0195989903199553,0.0273749999979516));
#41353=CARTESIAN_POINT('',(-0.00992554371029717,0.0227364328427525,0.0274687499979516));
#41354=CARTESIAN_POINT('',(-0.00678810118750004,0.0258738753655496,0.0275624999979516));
#41355=CARTESIAN_POINT('',(-0.00678810118750004,0.0303108891324553,0.0276562499979516));
#41356=CARTESIAN_POINT('',(-0.00678810118750004,0.0303108891324553,0.0276562499979516));
#41357=CARTESIAN_POINT('',(-0.00719405059375004,0.0303108891324553,0.0278906249969274));
#41358=CARTESIAN_POINT('',(-0.0076,0.0303108891324553,0.0281249999959032));
#41359=CARTESIAN_POINT('',(-0.0274,0.0303108891324553,0.0273749999959032));
#41360=CARTESIAN_POINT('',(-0.0274,0.0262101748649617,0.0274687499959032));
#41361=CARTESIAN_POINT('',(-0.0245003571337469,0.0233105319987085,0.0275624999959032));
#41362=CARTESIAN_POINT('',(-0.0216007142674937,0.0204108891324553,0.0276562499959032));
#41363=CARTESIAN_POINT('',(-0.0175,0.0204108891324553,0.0277499999959032));
#41364=CARTESIAN_POINT('',(-0.0133992857325064,0.0204108891324553,0.0278437499959032));
#41365=CARTESIAN_POINT('',(-0.0104996428662532,0.0233105319987085,0.0279374999959032));
#41366=CARTESIAN_POINT('',(-0.00760000000000004,0.0262101748649617,0.0280312499959032));
#41367=CARTESIAN_POINT('',(-0.0076,0.0303108891324553,0.0281249999959032));
#41368=CARTESIAN_POINT('',(-0.0274,0.0303108891324553,0.0273749999959032));
#41369=CARTESIAN_POINT('',(-0.0076,0.0303108891324553,0.0266249999959033));
#41370=CARTESIAN_POINT('',(-0.00760000000000004,0.0344116033999489,0.0267187499959032));
#41371=CARTESIAN_POINT('',(-0.0104996428662532,0.0373112462662021,0.0268124999959033));
#41372=CARTESIAN_POINT('',(-0.0133992857325064,0.0402108891324553,0.0269062499959032));
#41373=CARTESIAN_POINT('',(-0.0175,0.0402108891324554,0.0269999999959032));
#41374=CARTESIAN_POINT('',(-0.0216007142674937,0.0402108891324553,0.0270937499959032));
#41375=CARTESIAN_POINT('',(-0.0245003571337469,0.0373112462662021,0.0271874999959032));
#41376=CARTESIAN_POINT('',(-0.0274,0.0344116033999489,0.0272812499959032));
#41377=CARTESIAN_POINT('',(-0.0274,0.0303108891324553,0.0273749999959032));
#41378=CARTESIAN_POINT('',(-0.0076,0.0303108891324553,0.0266249999959033));
#41379=CARTESIAN_POINT('',(-0.0274,0.0303108891324553,0.0258749999959033));
#41380=CARTESIAN_POINT('',(-0.0274,0.0262101748649617,0.0259687499959032));
#41381=CARTESIAN_POINT('',(-0.0245003571337469,0.0233105319987085,0.0260624999959033));
#41382=CARTESIAN_POINT('',(-0.0216007142674937,0.0204108891324553,0.0261562499959032));
#41383=CARTESIAN_POINT('',(-0.0175,0.0204108891324553,0.0262499999959033));
#41384=CARTESIAN_POINT('',(-0.0133992857325064,0.0204108891324553,0.0263437499959032));
#41385=CARTESIAN_POINT('',(-0.0104996428662532,0.0233105319987085,0.0264374999959033));
#41386=CARTESIAN_POINT('',(-0.00760000000000004,0.0262101748649617,0.0265312499959032));
#41387=CARTESIAN_POINT('',(-0.0076,0.0303108891324553,0.0266249999959033));
#41388=CARTESIAN_POINT('',(-0.0274,0.0303108891324553,0.0258749999959033));
#41389=CARTESIAN_POINT('',(-0.0076,0.0303108891324553,0.0251249999959033));
#41390=CARTESIAN_POINT('',(-0.00760000000000002,0.034411603399949,0.0252187499959033));
#41391=CARTESIAN_POINT('',(-0.0104996428662532,0.0373112462662021,0.0253124999959033));
#41392=CARTESIAN_POINT('',(-0.0133992857325064,0.0402108891324553,0.0254062499959032));
#41393=CARTESIAN_POINT('',(-0.0175,0.0402108891324554,0.0254999999959033));
#41394=CARTESIAN_POINT('',(-0.0216007142674937,0.0402108891324553,0.0255937499959032));
#41395=CARTESIAN_POINT('',(-0.0245003571337469,0.0373112462662021,0.0256874999959033));
#41396=CARTESIAN_POINT('',(-0.0274,0.034411603399949,0.0257812499959032));
#41397=CARTESIAN_POINT('',(-0.0274,0.0303108891324553,0.0258749999959032));
#41398=CARTESIAN_POINT('',(-0.0076,0.0303108891324553,0.0251249999959033));
#41399=CARTESIAN_POINT('',(-0.0274,0.0303108891324553,0.0243749999959033));
#41400=CARTESIAN_POINT('',(-0.0274000000000001,0.0262101748649617,0.0244687499959032));
#41401=CARTESIAN_POINT('',(-0.0245003571337469,0.0233105319987085,0.0245624999959033));
#41402=CARTESIAN_POINT('',(-0.0216007142674937,0.0204108891324553,0.0246562499959032));
#41403=CARTESIAN_POINT('',(-0.0175,0.0204108891324553,0.0247499999959033));
#41404=CARTESIAN_POINT('',(-0.0133992857325064,0.0204108891324553,0.0248437499959032));
#41405=CARTESIAN_POINT('',(-0.0104996428662532,0.0233105319987085,0.0249374999959033));
#41406=CARTESIAN_POINT('',(-0.00760000000000006,0.0262101748649616,0.0250312499959033));
#41407=CARTESIAN_POINT('',(-0.0076,0.0303108891324553,0.0251249999959032));
#41408=CARTESIAN_POINT('',(-0.0274,0.0303108891324553,0.0243749999959032));
#41409=CARTESIAN_POINT('',(-0.0076,0.0303108891324553,0.0236249999959032));
#41410=CARTESIAN_POINT('',(-0.00760000000000006,0.034411603399949,0.0237187499959032));
#41411=CARTESIAN_POINT('',(-0.0104996428662532,0.0373112462662021,0.0238124999959032));
#41412=CARTESIAN_POINT('',(-0.0133992857325064,0.0402108891324553,0.0239062499959032));
#41413=CARTESIAN_POINT('',(-0.0175,0.0402108891324554,0.0239999999959032));
#41414=CARTESIAN_POINT('',(-0.0216007142674937,0.0402108891324553,0.0240937499959032));
#41415=CARTESIAN_POINT('',(-0.0245003571337469,0.0373112462662021,0.0241874999959032));
#41416=CARTESIAN_POINT('',(-0.0274,0.034411603399949,0.0242812499959032));
#41417=CARTESIAN_POINT('',(-0.0274,0.0303108891324553,0.0243749999959032));
#41418=CARTESIAN_POINT('',(-0.0076,0.0303108891324553,0.0236249999959032));
#41419=CARTESIAN_POINT('',(-0.0274,0.0303108891324553,0.0228749999959032));
#41420=CARTESIAN_POINT('',(-0.0274,0.0262101748649617,0.0229687499959032));
#41421=CARTESIAN_POINT('',(-0.0245003571337469,0.0233105319987085,0.0230624999959032));
#41422=CARTESIAN_POINT('',(-0.0216007142674937,0.0204108891324553,0.0231562499959032));
#41423=CARTESIAN_POINT('',(-0.0175,0.0204108891324553,0.0232499999959032));
#41424=CARTESIAN_POINT('',(-0.0133992857325064,0.0204108891324553,0.0233437499959032));
#41425=CARTESIAN_POINT('',(-0.0104996428662532,0.0233105319987085,0.0234374999959032));
#41426=CARTESIAN_POINT('',(-0.00760000000000003,0.0262101748649617,0.0235312499959033));
#41427=CARTESIAN_POINT('',(-0.0076,0.0303108891324553,0.0236249999959032));
#41428=CARTESIAN_POINT('',(-0.0274,0.0303108891324553,0.0228749999959033));
#41429=CARTESIAN_POINT('',(-0.0076,0.0303108891324553,0.0221249999959033));
#41430=CARTESIAN_POINT('',(-0.00760000000000004,0.0344116033999489,0.0222187499959032));
#41431=CARTESIAN_POINT('',(-0.0104996428662532,0.0373112462662021,0.0223124999959033));
#41432=CARTESIAN_POINT('',(-0.0133992857325064,0.0402108891324553,0.0224062499959032));
#41433=CARTESIAN_POINT('',(-0.0175,0.0402108891324554,0.0224999999959033));
#41434=CARTESIAN_POINT('',(-0.0216007142674937,0.0402108891324553,0.0225937499959032));
#41435=CARTESIAN_POINT('',(-0.0245003571337469,0.0373112462662021,0.0226874999959033));
#41436=CARTESIAN_POINT('',(-0.0274,0.0344116033999489,0.0227812499959032));
#41437=CARTESIAN_POINT('',(-0.0274,0.0303108891324553,0.0228749999959033));
#41438=CARTESIAN_POINT('',(-0.0076,0.0303108891324553,0.021));
#41439=CARTESIAN_POINT('',(-0.00760000000000004,0.0344116033999489,0.02109375));
#41440=CARTESIAN_POINT('',(-0.0104996428662532,0.0373112462662021,0.0211875));
#41441=CARTESIAN_POINT('',(-0.0133992857325064,0.0402108891324553,0.02128125));
#41442=CARTESIAN_POINT('',(-0.0175,0.0402108891324554,0.021375));
#41443=CARTESIAN_POINT('',(-0.0216007142674937,0.0402108891324553,0.02146875));
#41444=CARTESIAN_POINT('',(-0.0245003571337469,0.0373112462662021,0.0215625));
#41445=CARTESIAN_POINT('',(-0.0274,0.0344116033999489,0.02165625));
#41446=CARTESIAN_POINT('',(-0.0274,0.0303108891324553,0.02175));
#41447=CARTESIAN_POINT('',(-0.0274,0.0262101748649617,0.02184375));
#41448=CARTESIAN_POINT('',(-0.0245003571337469,0.0233105319987085,0.0219375));
#41449=CARTESIAN_POINT('',(-0.0216007142674937,0.0204108891324553,0.02203125));
#41450=CARTESIAN_POINT('',(-0.0175,0.0204108891324553,0.022125));
#41451=CARTESIAN_POINT('',(-0.0133992857325064,0.0204108891324553,0.02221875));
#41452=CARTESIAN_POINT('',(-0.0104996428662532,0.0233105319987085,0.0223125));
#41453=CARTESIAN_POINT('',(-0.00760000000000004,0.0262101748649617,0.02240625));
#41454=CARTESIAN_POINT('',(-0.0076,0.0303108891324553,0.0225));
#41455=CARTESIAN_POINT('',(-0.00760000000000004,0.0344116033999489,0.02259375));
#41456=CARTESIAN_POINT('',(-0.0104996428662532,0.0373112462662021,0.0226875));
#41457=CARTESIAN_POINT('',(-0.0133992857325064,0.0402108891324553,0.02278125));
#41458=CARTESIAN_POINT('',(-0.0175,0.0402108891324554,0.022875));
#41459=CARTESIAN_POINT('',(-0.0216007142674937,0.0402108891324553,0.02296875));
#41460=CARTESIAN_POINT('',(-0.0245003571337469,0.0373112462662021,0.0230625));
#41461=CARTESIAN_POINT('',(-0.0274,0.0344116033999489,0.02315625));
#41462=CARTESIAN_POINT('',(-0.0274,0.0303108891324553,0.02325));
#41463=CARTESIAN_POINT('',(-0.0274,0.0262101748649617,0.02334375));
#41464=CARTESIAN_POINT('',(-0.0245003571337469,0.0233105319987085,0.0234375));
#41465=CARTESIAN_POINT('',(-0.0216007142674937,0.0204108891324553,0.02353125));
#41466=CARTESIAN_POINT('',(-0.0175,0.0204108891324553,0.023625));
#41467=CARTESIAN_POINT('',(-0.0133992857325064,0.0204108891324553,0.02371875));
#41468=CARTESIAN_POINT('',(-0.0104996428662532,0.0233105319987085,0.0238125));
#41469=CARTESIAN_POINT('',(-0.00760000000000004,0.0262101748649617,0.02390625));
#41470=CARTESIAN_POINT('',(-0.0076,0.0303108891324553,0.024));
#41471=CARTESIAN_POINT('',(-0.00760000000000004,0.0344116033999489,0.02409375));
#41472=CARTESIAN_POINT('',(-0.0104996428662532,0.0373112462662021,0.0241875));
#41473=CARTESIAN_POINT('',(-0.0133992857325064,0.0402108891324553,0.02428125));
#41474=CARTESIAN_POINT('',(-0.0175,0.0402108891324554,0.024375));
#41475=CARTESIAN_POINT('',(-0.0216007142674937,0.0402108891324553,0.02446875));
#41476=CARTESIAN_POINT('',(-0.0245003571337469,0.0373112462662021,0.0245625));
#41477=CARTESIAN_POINT('',(-0.0274,0.0344116033999489,0.02465625));
#41478=CARTESIAN_POINT('',(-0.0274,0.0303108891324553,0.02475));
#41479=CARTESIAN_POINT('',(-0.0274,0.0262101748649617,0.02484375));
#41480=CARTESIAN_POINT('',(-0.0245003571337469,0.0233105319987085,0.0249375));
#41481=CARTESIAN_POINT('',(-0.0216007142674937,0.0204108891324553,0.02503125));
#41482=CARTESIAN_POINT('',(-0.0175,0.0204108891324553,0.025125));
#41483=CARTESIAN_POINT('',(-0.0133992857325064,0.0204108891324553,0.02521875));
#41484=CARTESIAN_POINT('',(-0.0104996428662532,0.0233105319987085,0.0253125));
#41485=CARTESIAN_POINT('',(-0.00760000000000004,0.0262101748649617,0.02540625));
#41486=CARTESIAN_POINT('',(-0.0076,0.0303108891324553,0.0255));
#41487=CARTESIAN_POINT('',(-0.00760000000000004,0.0344116033999489,0.02559375));
#41488=CARTESIAN_POINT('',(-0.0104996428662532,0.0373112462662021,0.0256875));
#41489=CARTESIAN_POINT('',(-0.0133992857325064,0.0402108891324553,0.02578125));
#41490=CARTESIAN_POINT('',(-0.0175,0.0402108891324554,0.025875));
#41491=CARTESIAN_POINT('',(-0.0216007142674937,0.0402108891324553,0.02596875));
#41492=CARTESIAN_POINT('',(-0.0245003571337469,0.0373112462662021,0.0260625));
#41493=CARTESIAN_POINT('',(-0.0274,0.0344116033999489,0.02615625));
#41494=CARTESIAN_POINT('',(-0.0274,0.0303108891324553,0.02625));
#41495=CARTESIAN_POINT('',(-0.0274,0.0262101748649617,0.02634375));
#41496=CARTESIAN_POINT('',(-0.0245003571337469,0.0233105319987085,0.0264375));
#41497=CARTESIAN_POINT('',(-0.0216007142674937,0.0204108891324553,0.02653125));
#41498=CARTESIAN_POINT('',(-0.0175,0.0204108891324553,0.026625));
#41499=CARTESIAN_POINT('',(-0.0133992857325064,0.0204108891324553,0.02671875));
#41500=CARTESIAN_POINT('',(-0.0104996428662532,0.0233105319987085,0.0268125));
#41501=CARTESIAN_POINT('',(-0.00760000000000004,0.0262101748649617,0.02690625));
#41502=CARTESIAN_POINT('',(-0.0076,0.0303108891324553,0.027));
#41503=CARTESIAN_POINT('',(-0.00678810118750004,0.0303108891324553,0.0214687499979516));
#41504=CARTESIAN_POINT('',(-0.00678810118750004,0.0347479028993611,0.0215624999979516));
#41505=CARTESIAN_POINT('',(-0.00992554371029717,0.0378853454221582,0.0216562499979516));
#41506=CARTESIAN_POINT('',(-0.0130629862330943,0.0410227879449553,0.0217499999979516));
#41507=CARTESIAN_POINT('',(-0.0175,0.0410227879449554,0.0218437499979516));
#41508=CARTESIAN_POINT('',(-0.0219370137669058,0.0410227879449553,0.0219374999979516));
#41509=CARTESIAN_POINT('',(-0.025074456289703,0.0378853454221582,0.0220312499979516));
#41510=CARTESIAN_POINT('',(-0.0282118988125001,0.0347479028993611,0.0221249999979516));
#41511=CARTESIAN_POINT('',(-0.0282118988125,0.0303108891324553,0.0222187499979516));
#41512=CARTESIAN_POINT('',(-0.0282118988125001,0.0258738753655496,0.0223124999979516));
#41513=CARTESIAN_POINT('',(-0.025074456289703,0.0227364328427525,0.0224062499979516));
#41514=CARTESIAN_POINT('',(-0.0219370137669058,0.0195989903199553,0.0224999999979516));
#41515=CARTESIAN_POINT('',(-0.0175,0.0195989903199554,0.0225937499979516));
#41516=CARTESIAN_POINT('',(-0.0130629862330943,0.0195989903199553,0.0226874999979516));
#41517=CARTESIAN_POINT('',(-0.00992554371029717,0.0227364328427525,0.0227812499979516));
#41518=CARTESIAN_POINT('',(-0.00678810118750004,0.0258738753655496,0.0228749999979516));
#41519=CARTESIAN_POINT('',(-0.00678810118750004,0.0303108891324553,0.0229687499979516));
#41520=CARTESIAN_POINT('',(-0.00678810118750004,0.0347479028993611,0.0230624999979516));
#41521=CARTESIAN_POINT('',(-0.00992554371029717,0.0378853454221582,0.0231562499979516));
#41522=CARTESIAN_POINT('',(-0.0130629862330943,0.0410227879449553,0.0232499999979516));
#41523=CARTESIAN_POINT('',(-0.0175,0.0410227879449554,0.0233437499979516));
#41524=CARTESIAN_POINT('',(-0.0219370137669058,0.0410227879449553,0.0234374999979516));
#41525=CARTESIAN_POINT('',(-0.025074456289703,0.0378853454221582,0.0235312499979516));
#41526=CARTESIAN_POINT('',(-0.0282118988125001,0.0347479028993611,0.0236249999979516));
#41527=CARTESIAN_POINT('',(-0.0282118988125,0.0303108891324553,0.0237187499979516));
#41528=CARTESIAN_POINT('',(-0.0282118988125001,0.0258738753655496,0.0238124999979516));
#41529=CARTESIAN_POINT('',(-0.025074456289703,0.0227364328427525,0.0239062499979516));
#41530=CARTESIAN_POINT('',(-0.0219370137669058,0.0195989903199553,0.0239999999979516));
#41531=CARTESIAN_POINT('',(-0.0175,0.0195989903199554,0.0240937499979516));
#41532=CARTESIAN_POINT('',(-0.0130629862330943,0.0195989903199553,0.0241874999979516));
#41533=CARTESIAN_POINT('',(-0.00992554371029717,0.0227364328427525,0.0242812499979516));
#41534=CARTESIAN_POINT('',(-0.00678810118750004,0.0258738753655496,0.0243749999979516));
#41535=CARTESIAN_POINT('',(-0.00678810118750004,0.0303108891324553,0.0244687499979516));
#41536=CARTESIAN_POINT('',(-0.00678810118750004,0.0347479028993611,0.0245624999979516));
#41537=CARTESIAN_POINT('',(-0.00992554371029717,0.0378853454221582,0.0246562499979516));
#41538=CARTESIAN_POINT('',(-0.0130629862330943,0.0410227879449553,0.0247499999979516));
#41539=CARTESIAN_POINT('',(-0.0175,0.0410227879449554,0.0248437499979516));
#41540=CARTESIAN_POINT('',(-0.0219370137669058,0.0410227879449553,0.0249374999979516));
#41541=CARTESIAN_POINT('',(-0.025074456289703,0.0378853454221582,0.0250312499979516));
#41542=CARTESIAN_POINT('',(-0.0282118988125001,0.0347479028993611,0.0251249999979516));
#41543=CARTESIAN_POINT('',(-0.0282118988125,0.0303108891324553,0.0252187499979516));
#41544=CARTESIAN_POINT('',(-0.0282118988125001,0.0258738753655496,0.0253124999979516));
#41545=CARTESIAN_POINT('',(-0.025074456289703,0.0227364328427525,0.0254062499979516));
#41546=CARTESIAN_POINT('',(-0.0219370137669058,0.0195989903199553,0.0254999999979516));
#41547=CARTESIAN_POINT('',(-0.0175,0.0195989903199554,0.0255937499979516));
#41548=CARTESIAN_POINT('',(-0.0130629862330943,0.0195989903199553,0.0256874999979516));
#41549=CARTESIAN_POINT('',(-0.00992554371029717,0.0227364328427525,0.0257812499979516));
#41550=CARTESIAN_POINT('',(-0.00678810118750004,0.0258738753655496,0.0258749999979516));
#41551=CARTESIAN_POINT('',(-0.00678810118750004,0.0303108891324553,0.0259687499979516));
#41552=CARTESIAN_POINT('',(-0.00678810118750004,0.0347479028993611,0.0260624999979516));
#41553=CARTESIAN_POINT('',(-0.00992554371029717,0.0378853454221582,0.0261562499979516));
#41554=CARTESIAN_POINT('',(-0.0130629862330943,0.0410227879449553,0.0262499999979516));
#41555=CARTESIAN_POINT('',(-0.0175,0.0410227879449554,0.0263437499979516));
#41556=CARTESIAN_POINT('',(-0.0219370137669058,0.0410227879449553,0.0264374999979516));
#41557=CARTESIAN_POINT('',(-0.025074456289703,0.0378853454221582,0.0265312499979516));
#41558=CARTESIAN_POINT('',(-0.0282118988125001,0.0347479028993611,0.0266249999979516));
#41559=CARTESIAN_POINT('',(-0.0282118988125,0.0303108891324553,0.0267187499979516));
#41560=CARTESIAN_POINT('',(-0.0282118988125001,0.0258738753655496,0.0268124999979516));
#41561=CARTESIAN_POINT('',(-0.025074456289703,0.0227364328427525,0.0269062499979516));
#41562=CARTESIAN_POINT('',(-0.0219370137669058,0.0195989903199553,0.0269999999979516));
#41563=CARTESIAN_POINT('',(-0.0175,0.0195989903199554,0.0270937499979516));
#41564=CARTESIAN_POINT('',(-0.0130629862330943,0.0195989903199553,0.0271874999979516));
#41565=CARTESIAN_POINT('',(-0.00992554371029717,0.0227364328427525,0.0272812499979516));
#41566=CARTESIAN_POINT('',(-0.00678810118750004,0.0258738753655496,0.0273749999979516));
#41567=CARTESIAN_POINT('',(-0.00678810118750004,0.0303108891324553,0.0274687499979516));
#41568=CARTESIAN_POINT('',(-0.00719405059375004,0.0303108891324553,0.0212343749989758));
#41569=CARTESIAN_POINT('',(-0.0076,0.0303108891324553,0.021));
#41570=CARTESIAN_POINT('',(-0.00678810118750004,0.0303108891324553,0.0214687499979516));
#41571=CARTESIAN_POINT('',(-0.0076,0.0303108891324553,0.021));
#41572=CARTESIAN_POINT('',(-0.00760000000000004,0.0344116033999489,0.02109375));
#41573=CARTESIAN_POINT('',(-0.0104996428662532,0.0373112462662021,0.0211875));
#41574=CARTESIAN_POINT('',(-0.0133992857325064,0.0402108891324553,0.02128125));
#41575=CARTESIAN_POINT('',(-0.0175,0.0402108891324554,0.021375));
#41576=CARTESIAN_POINT('',(-0.0216007142674937,0.0402108891324553,0.02146875));
#41577=CARTESIAN_POINT('',(-0.0245003571337469,0.0373112462662021,0.0215625));
#41578=CARTESIAN_POINT('',(-0.0274,0.0344116033999489,0.02165625));
#41579=CARTESIAN_POINT('',(-0.0274,0.0303108891324553,0.02175));
#41580=CARTESIAN_POINT('',(-0.0274,0.0303108891324553,0.02175));
#41581=CARTESIAN_POINT('',(-0.0274,0.0303108891324553,0.02175));
#41582=CARTESIAN_POINT('',(-0.0274,0.0262101748649617,0.02184375));
#41583=CARTESIAN_POINT('',(-0.0245003571337469,0.0233105319987085,0.0219375));
#41584=CARTESIAN_POINT('',(-0.0216007142674937,0.0204108891324553,0.02203125));
#41585=CARTESIAN_POINT('',(-0.0175,0.0204108891324553,0.022125));
#41586=CARTESIAN_POINT('',(-0.0133992857325064,0.0204108891324553,0.02221875));
#41587=CARTESIAN_POINT('',(-0.0104996428662532,0.0233105319987085,0.0223125));
#41588=CARTESIAN_POINT('',(-0.00760000000000003,0.0262101748649617,0.02240625));
#41589=CARTESIAN_POINT('',(-0.0076,0.0303108891324553,0.0225));
#41590=CARTESIAN_POINT('',(-0.0076,0.0303108891324553,0.0225));
#41591=CARTESIAN_POINT('',(-0.0076,0.0303108891324553,0.0225));
#41592=CARTESIAN_POINT('',(-0.00760000000000006,0.034411603399949,0.02259375));
#41593=CARTESIAN_POINT('',(-0.0104996428662532,0.0373112462662021,0.0226875));
#41594=CARTESIAN_POINT('',(-0.0133992857325064,0.0402108891324553,0.02278125));
#41595=CARTESIAN_POINT('',(-0.0175,0.0402108891324554,0.022875));
#41596=CARTESIAN_POINT('',(-0.0216007142674937,0.0402108891324553,0.02296875));
#41597=CARTESIAN_POINT('',(-0.0245003571337469,0.0373112462662021,0.0230625));
#41598=CARTESIAN_POINT('',(-0.0274000000000001,0.0344116033999489,0.02315625));
#41599=CARTESIAN_POINT('',(-0.0274,0.0303108891324553,0.02325));
#41600=CARTESIAN_POINT('',(-0.0274,0.0303108891324553,0.02325));
#41601=CARTESIAN_POINT('',(-0.0274,0.0303108891324553,0.02325));
#41602=CARTESIAN_POINT('',(-0.0274,0.0262101748649617,0.02334375));
#41603=CARTESIAN_POINT('',(-0.0245003571337469,0.0233105319987085,0.0234375));
#41604=CARTESIAN_POINT('',(-0.0216007142674937,0.0204108891324553,0.02353125));
#41605=CARTESIAN_POINT('',(-0.0175,0.0204108891324553,0.023625));
#41606=CARTESIAN_POINT('',(-0.0133992857325064,0.0204108891324553,0.02371875));
#41607=CARTESIAN_POINT('',(-0.0104996428662532,0.0233105319987085,0.0238125));
#41608=CARTESIAN_POINT('',(-0.00760000000000006,0.0262101748649616,0.02390625));
#41609=CARTESIAN_POINT('',(-0.0076,0.0303108891324553,0.024));
#41610=CARTESIAN_POINT('',(-0.0076,0.0303108891324553,0.024));
#41611=CARTESIAN_POINT('',(-0.0076,0.0303108891324553,0.024));
#41612=CARTESIAN_POINT('',(-0.00760000000000002,0.034411603399949,0.02409375));
#41613=CARTESIAN_POINT('',(-0.0104996428662532,0.0373112462662021,0.0241875));
#41614=CARTESIAN_POINT('',(-0.0133992857325064,0.0402108891324553,0.02428125));
#41615=CARTESIAN_POINT('',(-0.0175,0.0402108891324554,0.024375));
#41616=CARTESIAN_POINT('',(-0.0216007142674937,0.0402108891324553,0.02446875));
#41617=CARTESIAN_POINT('',(-0.0245003571337469,0.0373112462662021,0.0245625));
#41618=CARTESIAN_POINT('',(-0.0274,0.034411603399949,0.02465625));
#41619=CARTESIAN_POINT('',(-0.0274,0.0303108891324553,0.02475));
#41620=CARTESIAN_POINT('',(-0.0274,0.0303108891324553,0.02475));
#41621=CARTESIAN_POINT('',(-0.0274,0.0303108891324553,0.02475));
#41622=CARTESIAN_POINT('',(-0.0274,0.0262101748649617,0.02484375));
#41623=CARTESIAN_POINT('',(-0.0245003571337469,0.0233105319987085,0.0249375));
#41624=CARTESIAN_POINT('',(-0.0216007142674937,0.0204108891324553,0.02503125));
#41625=CARTESIAN_POINT('',(-0.0175,0.0204108891324553,0.025125));
#41626=CARTESIAN_POINT('',(-0.0133992857325064,0.0204108891324553,0.02521875));
#41627=CARTESIAN_POINT('',(-0.0104996428662532,0.0233105319987085,0.0253125));
#41628=CARTESIAN_POINT('',(-0.00760000000000004,0.0262101748649617,0.02540625));
#41629=CARTESIAN_POINT('',(-0.0076,0.0303108891324553,0.0255));
#41630=CARTESIAN_POINT('',(-0.0076,0.0303108891324553,0.0255));
#41631=CARTESIAN_POINT('',(-0.0076,0.0303108891324553,0.0255));
#41632=CARTESIAN_POINT('',(-0.00760000000000004,0.0344116033999489,0.02559375));
#41633=CARTESIAN_POINT('',(-0.0104996428662532,0.0373112462662021,0.0256875));
#41634=CARTESIAN_POINT('',(-0.0133992857325064,0.0402108891324553,0.02578125));
#41635=CARTESIAN_POINT('',(-0.0175,0.0402108891324554,0.025875));
#41636=CARTESIAN_POINT('',(-0.0216007142674937,0.0402108891324553,0.02596875));
#41637=CARTESIAN_POINT('',(-0.0245003571337469,0.0373112462662021,0.0260625));
#41638=CARTESIAN_POINT('',(-0.0274,0.0344116033999489,0.02615625));
#41639=CARTESIAN_POINT('',(-0.0274,0.0303108891324553,0.02625));
#41640=CARTESIAN_POINT('',(-0.0274,0.0303108891324553,0.02625));
#41641=CARTESIAN_POINT('',(-0.0274,0.0303108891324553,0.02625));
#41642=CARTESIAN_POINT('',(-0.0274,0.0262101748649617,0.02634375));
#41643=CARTESIAN_POINT('',(-0.0245003571337469,0.0233105319987085,0.0264375));
#41644=CARTESIAN_POINT('',(-0.0216007142674937,0.0204108891324553,0.02653125));
#41645=CARTESIAN_POINT('',(-0.0175,0.0204108891324553,0.026625));
#41646=CARTESIAN_POINT('',(-0.0133992857325064,0.0204108891324553,0.02671875));
#41647=CARTESIAN_POINT('',(-0.0104996428662532,0.0233105319987085,0.0268125));
#41648=CARTESIAN_POINT('',(-0.00760000000000004,0.0262101748649617,0.02690625));
#41649=CARTESIAN_POINT('',(-0.0076,0.0303108891324553,0.027));
#41650=CARTESIAN_POINT('',(-0.0076,0.0303108891324553,0.027));
#41651=CARTESIAN_POINT('',(-0.00719405059375004,0.0303108891324553,0.0272343749989758));
#41652=CARTESIAN_POINT('',(-0.00678810118750004,0.0303108891324553,0.0274687499979516));
#41653=CARTESIAN_POINT('',(-0.00678810118750004,0.0303108891324553,0.0214687499979516));
#41654=CARTESIAN_POINT('',(-0.00678810118750004,0.0347479028993611,0.0215624999979516));
#41655=CARTESIAN_POINT('',(-0.00992554371029717,0.0378853454221582,0.0216562499979516));
#41656=CARTESIAN_POINT('',(-0.0130629862330943,0.0410227879449553,0.0217499999979516));
#41657=CARTESIAN_POINT('',(-0.0175,0.0410227879449554,0.0218437499979516));
#41658=CARTESIAN_POINT('',(-0.0219370137669058,0.0410227879449553,0.0219374999979516));
#41659=CARTESIAN_POINT('',(-0.025074456289703,0.0378853454221582,0.0220312499979516));
#41660=CARTESIAN_POINT('',(-0.0282118988125001,0.0347479028993611,0.0221249999979516));
#41661=CARTESIAN_POINT('',(-0.0282118988125,0.0303108891324553,0.0222187499979516));
#41662=CARTESIAN_POINT('',(-0.0282118988125001,0.0258738753655496,0.0223124999979516));
#41663=CARTESIAN_POINT('',(-0.025074456289703,0.0227364328427525,0.0224062499979516));
#41664=CARTESIAN_POINT('',(-0.0219370137669058,0.0195989903199553,0.0224999999979516));
#41665=CARTESIAN_POINT('',(-0.0175,0.0195989903199554,0.0225937499979516));
#41666=CARTESIAN_POINT('',(-0.0130629862330943,0.0195989903199553,0.0226874999979516));
#41667=CARTESIAN_POINT('',(-0.00992554371029717,0.0227364328427525,0.0227812499979516));
#41668=CARTESIAN_POINT('',(-0.00678810118750004,0.0258738753655496,0.0228749999979516));
#41669=CARTESIAN_POINT('',(-0.00678810118750004,0.0303108891324553,0.0229687499979516));
#41670=CARTESIAN_POINT('',(-0.00678810118750004,0.0347479028993611,0.0230624999979516));
#41671=CARTESIAN_POINT('',(-0.00992554371029717,0.0378853454221582,0.0231562499979516));
#41672=CARTESIAN_POINT('',(-0.0130629862330943,0.0410227879449553,0.0232499999979516));
#41673=CARTESIAN_POINT('',(-0.0175,0.0410227879449554,0.0233437499979516));
#41674=CARTESIAN_POINT('',(-0.0219370137669058,0.0410227879449553,0.0234374999979516));
#41675=CARTESIAN_POINT('',(-0.025074456289703,0.0378853454221582,0.0235312499979516));
#41676=CARTESIAN_POINT('',(-0.0282118988125001,0.0347479028993611,0.0236249999979516));
#41677=CARTESIAN_POINT('',(-0.0282118988125,0.0303108891324553,0.0237187499979516));
#41678=CARTESIAN_POINT('',(-0.0282118988125001,0.0258738753655496,0.0238124999979516));
#41679=CARTESIAN_POINT('',(-0.025074456289703,0.0227364328427525,0.0239062499979516));
#41680=CARTESIAN_POINT('',(-0.0219370137669058,0.0195989903199553,0.0239999999979516));
#41681=CARTESIAN_POINT('',(-0.0175,0.0195989903199554,0.0240937499979516));
#41682=CARTESIAN_POINT('',(-0.0130629862330943,0.0195989903199553,0.0241874999979516));
#41683=CARTESIAN_POINT('',(-0.00992554371029717,0.0227364328427525,0.0242812499979516));
#41684=CARTESIAN_POINT('',(-0.00678810118750004,0.0258738753655496,0.0243749999979516));
#41685=CARTESIAN_POINT('',(-0.00678810118750004,0.0303108891324553,0.0244687499979516));
#41686=CARTESIAN_POINT('',(-0.00678810118750004,0.0347479028993611,0.0245624999979516));
#41687=CARTESIAN_POINT('',(-0.00992554371029717,0.0378853454221582,0.0246562499979516));
#41688=CARTESIAN_POINT('',(-0.0130629862330943,0.0410227879449553,0.0247499999979516));
#41689=CARTESIAN_POINT('',(-0.0175,0.0410227879449554,0.0248437499979516));
#41690=CARTESIAN_POINT('',(-0.0219370137669058,0.0410227879449553,0.0249374999979516));
#41691=CARTESIAN_POINT('',(-0.025074456289703,0.0378853454221582,0.0250312499979516));
#41692=CARTESIAN_POINT('',(-0.0282118988125001,0.0347479028993611,0.0251249999979516));
#41693=CARTESIAN_POINT('',(-0.0282118988125,0.0303108891324553,0.0252187499979516));
#41694=CARTESIAN_POINT('',(-0.0282118988125001,0.0258738753655496,0.0253124999979516));
#41695=CARTESIAN_POINT('',(-0.025074456289703,0.0227364328427525,0.0254062499979516));
#41696=CARTESIAN_POINT('',(-0.0219370137669058,0.0195989903199553,0.0254999999979516));
#41697=CARTESIAN_POINT('',(-0.0175,0.0195989903199554,0.0255937499979516));
#41698=CARTESIAN_POINT('',(-0.0130629862330943,0.0195989903199553,0.0256874999979516));
#41699=CARTESIAN_POINT('',(-0.00992554371029717,0.0227364328427525,0.0257812499979516));
#41700=CARTESIAN_POINT('',(-0.00678810118750004,0.0258738753655496,0.0258749999979516));
#41701=CARTESIAN_POINT('',(-0.00678810118750004,0.0303108891324553,0.0259687499979516));
#41702=CARTESIAN_POINT('',(-0.00678810118750004,0.0347479028993611,0.0260624999979516));
#41703=CARTESIAN_POINT('',(-0.00992554371029717,0.0378853454221582,0.0261562499979516));
#41704=CARTESIAN_POINT('',(-0.0130629862330943,0.0410227879449553,0.0262499999979516));
#41705=CARTESIAN_POINT('',(-0.0175,0.0410227879449554,0.0263437499979516));
#41706=CARTESIAN_POINT('',(-0.0219370137669058,0.0410227879449553,0.0264374999979516));
#41707=CARTESIAN_POINT('',(-0.025074456289703,0.0378853454221582,0.0265312499979516));
#41708=CARTESIAN_POINT('',(-0.0282118988125001,0.0347479028993611,0.0266249999979516));
#41709=CARTESIAN_POINT('',(-0.0282118988125,0.0303108891324553,0.0267187499979516));
#41710=CARTESIAN_POINT('',(-0.0282118988125001,0.0258738753655496,0.0268124999979516));
#41711=CARTESIAN_POINT('',(-0.025074456289703,0.0227364328427525,0.0269062499979516));
#41712=CARTESIAN_POINT('',(-0.0219370137669058,0.0195989903199553,0.0269999999979516));
#41713=CARTESIAN_POINT('',(-0.0175,0.0195989903199554,0.0270937499979516));
#41714=CARTESIAN_POINT('',(-0.0130629862330943,0.0195989903199553,0.0271874999979516));
#41715=CARTESIAN_POINT('',(-0.00992554371029717,0.0227364328427525,0.0272812499979516));
#41716=CARTESIAN_POINT('',(-0.00678810118750004,0.0258738753655496,0.0273749999979516));
#41717=CARTESIAN_POINT('',(-0.00678810118750004,0.0303108891324553,0.0274687499979516));
#41718=CARTESIAN_POINT('',(-0.0175,0.0303108891324553,0.0227055389329771));
#41719=CARTESIAN_POINT('',(-0.00678810118750004,0.0303108891324553,0.0215624999979516));
#41720=CARTESIAN_POINT('',(-0.00678810118750004,0.0303108891324553,0.0275624999979516));
#41721=CARTESIAN_POINT('',(-0.00678810118750004,0.0303108891324553,0.0275624999979516));
#41722=CARTESIAN_POINT('',(-0.0076,0.0303108891324553,0.0275624999979516));
#41723=CARTESIAN_POINT('',(-0.00678810118750004,0.0303108891324553,0.0275624999979516));
#41724=CARTESIAN_POINT('',(-0.0076,0.0303108891324553,0.0215624999979516));
#41725=CARTESIAN_POINT('',(-0.0115,0.0303108891324553,0.031));
#41726=CARTESIAN_POINT('',(-0.00953134086570699,0.0310183293076278,0.021011430723831));
#41727=CARTESIAN_POINT('',(-0.00953134086570699,0.0310183293076278,0.021));
#41728=CARTESIAN_POINT('',(-0.00953134086570699,0.0310183293076278,0.026));
#41729=CARTESIAN_POINT('',(-0.0115,0.0303108891324553,0.026));
#41730=CARTESIAN_POINT('',(-0.00953134086570699,0.0296034489572829,0.026));
#41731=CARTESIAN_POINT('',(-0.00953134086570699,0.0296034489572829,0.021011430723831));
#41732=CARTESIAN_POINT('',(-0.00953134086570699,0.0296034489572829,0.021));
#41733=CARTESIAN_POINT('',(-0.0115,0.0303108891324553,0.021));
#41734=CARTESIAN_POINT('',(-0.0115,0.0303108891324553,0.031));
#41735=CARTESIAN_POINT('',(-0.0115,0.0303108891324553,0.031));
#41736=CARTESIAN_POINT('',(-0.013,0.0303108891324553,0.031));
#41737=CARTESIAN_POINT('',(-0.0115,0.0303108891324553,0.031));
#41738=CARTESIAN_POINT('',(-0.0105,0.0303108891324553,0.031));
#41739=CARTESIAN_POINT('',(-0.0175,0.0303108891324553,0.014));
#41740=CARTESIAN_POINT('',(-0.0101875,0.027066302294351,0.026));
#41741=CARTESIAN_POINT('',(-0.0101875,0.027066302294351,0.021));
#41742=CARTESIAN_POINT('',(-0.0175,0.0303108891324553,0.021));
#41743=CARTESIAN_POINT('',(-0.0101875,0.0335554759705597,0.021));
#41744=CARTESIAN_POINT('',(-0.0101875,0.0335554759705597,0.026));
#41745=CARTESIAN_POINT('',(-0.0099006579232147,0.0328108891324553,0.0142731879764631));
#41746=CARTESIAN_POINT('',(-0.0099006579232147,0.0328108891324553,0.091));
#41747=CARTESIAN_POINT('',(-0.0175,0.0303108891324553,0.091));
#41748=CARTESIAN_POINT('',(-0.0099006579232147,0.0278108891324554,0.091));
#41749=CARTESIAN_POINT('',(-0.0099006579232147,0.0278108891324554,0.0142731879764631));
#41750=CARTESIAN_POINT('',(-0.0175,0.0303108891324553,0.091));
#41751=CARTESIAN_POINT('',(-0.0115,0.0303108891324553,0.091));
#41752=CARTESIAN_POINT('',(-0.01,0.0303108891324553,0.091));
#41753=CARTESIAN_POINT('',(-0.0175,0.0303108891324553,0.091));
#41754=CARTESIAN_POINT('',(-0.0274,0.0303108891324553,0.091));
#41755=CARTESIAN_POINT('',(-0.0115,0.0328108891324553,0.091));
#41756=CARTESIAN_POINT('',(-0.0115,0.0328108891324553,0.091));
#41757=CARTESIAN_POINT('',(-0.0115,0.0303108891324553,0.091));
#41758=CARTESIAN_POINT('',(-0.0115,0.0278108891324554,0.091));
#41759=CARTESIAN_POINT('',(-0.0115,0.0278108891324554,0.091));
#41760=CARTESIAN_POINT('',(-0.0115,0.0278108891324554,0.0142731879764631));
#41761=CARTESIAN_POINT('',(-0.0115,0.0278108891324554,0.0142731879764631));
#41762=CARTESIAN_POINT('',(-0.0115,0.0328108891324553,0.0142731879764631));
#41763=CARTESIAN_POINT('',(-0.0115,0.0328108891324553,0.0142731879764631));
#41764=CARTESIAN_POINT('',(-0.0115,0.0303108891324553,0.0142731879764631));
#41765=CARTESIAN_POINT('',(-0.0175,0.0303108891324553,0.021));
#41766=CARTESIAN_POINT('',(-0.00879583654340205,0.0308108891324553,0.021));
#41767=CARTESIAN_POINT('',(-0.00879583654340205,0.0298108891324554,0.021));
#41768=CARTESIAN_POINT('',(-0.0175,0.0303108891324553,0.021));
#41769=CARTESIAN_POINT('',(-0.0175,0.0303108891324553,0.021));
#41770=CARTESIAN_POINT('',(-0.0115,0.0303108891324553,0.021));
#41771=CARTESIAN_POINT('',(-0.0115,0.0303108891324553,0.021));
#41772=CARTESIAN_POINT('',(-0.0115,0.0303108891324553,0.021));
#41773=CARTESIAN_POINT('',(-0.0175,0.0303108891324553,0.091));
#41774=CARTESIAN_POINT('',(-0.0175,0.0303108891324553,0.014));
#41775=CARTESIAN_POINT('',(-0.00953134086570699,0.0310183293076278,0.026));
#41776=CARTESIAN_POINT('',(-0.00951275551339847,0.0308089825068169,0.0261464579794882));
#41777=CARTESIAN_POINT('',(-0.00948724312072826,0.0303094965600865,0.0263585979226248));
#41778=CARTESIAN_POINT('',(-0.00951275836916453,0.0298127635905308,0.0261464354752214));
#41779=CARTESIAN_POINT('',(-0.00953134086570699,0.029603448957283,0.026));
#41780=CARTESIAN_POINT('',(-0.0115,0.0303108891324553,0.0142731879764631));
#41781=CARTESIAN_POINT('',(-0.0115,0.0303108891324553,0.031));
#41782=CARTESIAN_POINT('',(-0.0115,0.0303108891324553,0.029));
#41783=CARTESIAN_POINT('',(-0.0105,0.0303108891324553,0.029));
#41784=CARTESIAN_POINT('',(-0.0115,0.0303108891324553,0.029));
#41785=CARTESIAN_POINT('',(-0.0115,0.0303108891324553,0.031));
#41786=CARTESIAN_POINT('',(-0.0115,0.0303108891324553,0.026));
#41787=CARTESIAN_POINT('',(-0.0115,0.0303108891324553,0.026));
#41788=CARTESIAN_POINT('',(-0.00879583654340205,0.0308108891324553,0.026));
#41789=CARTESIAN_POINT('',(-0.00879583654340205,0.0298108891324554,0.026));
#41790=CARTESIAN_POINT('',(-0.00427548757800061,-0.0020945466955101,4.21297175334708E-35));
#41791=CARTESIAN_POINT('',(-0.00295442325903663,-0.000520944533000792,-0.0210189377942895));
#41792=CARTESIAN_POINT('',(-1.61911969068189E-18,9.18248406554907E-18,-0.00540230489496124));
#41793=CARTESIAN_POINT('',(-0.00295442325903663,-0.000520944533000792,-0.0110189377942895));
#41794=CARTESIAN_POINT('',(-0.00590884651807325,-0.00104188906600159,-0.0166355706936178));
#41795=CARTESIAN_POINT('',(-0.00590884651807325,-0.00104188906600159,-0.0210189377942895));
#41796=CARTESIAN_POINT('',(-0.00590884651807325,-0.00104188906600159,-0.0176355706936178));
#41797=CARTESIAN_POINT('',(-0.00746781659002574,-0.00131677755180384,-0.0176355706936178));
#41798=CARTESIAN_POINT('',(-0.00433080680353718,-0.000763638087699395,-0.0176355706936178));
#41799=CARTESIAN_POINT('',(-1.61911969068189E-18,9.18248406554907E-18,-0.00940230489496124));
#41800=CARTESIAN_POINT('',(-0.00295442325903663,-0.000520944533000792,-0.0150189377942895));
#41801=CARTESIAN_POINT('',(-0.00295442325903663,-0.000520944533000792,-0.0210189377942895));
#41802=CARTESIAN_POINT('',(0.,0.,-0.0210189377942895));
#41803=CARTESIAN_POINT('',(0.,0.,-0.0166355706936178));
#41804=CARTESIAN_POINT('',(-0.00104188906600158,-0.00590884651807325,-0.0166355706936178));
#41805=CARTESIAN_POINT('',(-0.00104188906600158,-0.00590884651807325,-0.0210189377942895));
#41806=CARTESIAN_POINT('',(-0.00104188906600158,-0.00590884651807325,-0.0176355706936178));
#41807=CARTESIAN_POINT('',(0.,0.,-0.0176355706936178));
#41808=CARTESIAN_POINT('',(-0.000520944533000823,-0.00295442325903662,-0.0210189377942895));
#41809=CARTESIAN_POINT('',(-6.4490934599903E-17,1.13714917810672E-17,-0.00540230489496124));
#41810=CARTESIAN_POINT('',(-0.000520944533000823,-0.00295442325903662,-0.0110189377942895));
#41811=CARTESIAN_POINT('',(-0.000520944533000823,-0.00295442325903662,-0.0210189377942895));
#41812=CARTESIAN_POINT('',(-0.000520944533000823,-0.00295442325903662,-0.0150189377942895));
#41813=CARTESIAN_POINT('',(-6.4490934599903E-17,1.13714917810672E-17,-0.00940230489496124));
#41814=CARTESIAN_POINT('',(-0.000763638087699406,-0.00433080680353718,-0.0176355706936178));
#41815=CARTESIAN_POINT('',(-0.000232183409974289,-0.00131677755180373,-0.0176355706936178));
#41816=CARTESIAN_POINT('',(0.,0.,-0.0210189377942895));
#41817=CARTESIAN_POINT('',(0.,0.,-0.0150189377942895));
#41818=CARTESIAN_POINT('',(0.,0.,-0.0110189377942895));
#41819=CARTESIAN_POINT('',(-0.00295442325903663,-0.000520944533000792,-0.0210189377942895));
#41820=CARTESIAN_POINT('',(8.99929316448808E-18,-5.1037527713168E-17,-0.00540230489496124));
#41821=CARTESIAN_POINT('',(0.00295442325903663,0.000520944533000772,-0.0110189377942895));
#41822=CARTESIAN_POINT('',(0.00590884651807325,0.00104188906600159,-0.0166355706936178));
#41823=CARTESIAN_POINT('',(0.00590884651807325,0.00104188906600159,-0.0210189377942895));
#41824=CARTESIAN_POINT('',(0.00590884651807325,0.00104188906600159,-0.0176355706936178));
#41825=CARTESIAN_POINT('',(-0.00746781659002571,-0.00131677755180395,-0.0176355706936178));
#41826=CARTESIAN_POINT('',(0.00433080680353718,0.000763638087699384,-0.0176355706936178));
#41827=CARTESIAN_POINT('',(8.99929316448808E-18,-5.1037527713168E-17,-0.00940230489496124));
#41828=CARTESIAN_POINT('',(0.00295442325903663,0.000520944533000771,-0.0150189377942895));
#41829=CARTESIAN_POINT('',(0.00295442325903663,0.000520944533000771,-0.0210189377942895));
#41830=CARTESIAN_POINT('',(0.,0.,-0.0210189377942895));
#41831=CARTESIAN_POINT('',(0.,0.,-0.0166355706936178));
#41832=CARTESIAN_POINT('',(0.00104188906600158,0.00590884651807325,-0.0166355706936178));
#41833=CARTESIAN_POINT('',(0.00104188906600158,0.00590884651807325,-0.0210189377942895));
#41834=CARTESIAN_POINT('',(0.00104188906600158,0.00590884651807325,-0.0176355706936178));
#41835=CARTESIAN_POINT('',(0.,0.,-0.0176355706936178));
#41836=CARTESIAN_POINT('',(-0.000520944533000823,-0.00295442325903662,-0.0210189377942895));
#41837=CARTESIAN_POINT('',(2.25291178817541E-17,-3.9724913341147E-18,-0.00540230489496124));
#41838=CARTESIAN_POINT('',(0.000520944533000802,0.00295442325903663,-0.0110189377942895));
#41839=CARTESIAN_POINT('',(0.000520944533000802,0.00295442325903663,-0.0210189377942895));
#41840=CARTESIAN_POINT('',(0.000520944533000802,0.00295442325903663,-0.0150189377942895));
#41841=CARTESIAN_POINT('',(2.25291178817541E-17,-3.9724913341147E-18,-0.00940230489496124));
#41842=CARTESIAN_POINT('',(0.000763638087699395,0.00433080680353718,-0.0176355706936178));
#41843=CARTESIAN_POINT('',(-0.000232183409974221,-0.0013167775518038,-0.0176355706936178));
#41844=CARTESIAN_POINT('',(0.,0.,-0.0210189377942895));
#41845=CARTESIAN_POINT('',(0.,0.,-0.0150189377942895));
#41846=CARTESIAN_POINT('',(0.,0.,-0.0110189377942895));
#41847=CARTESIAN_POINT('',(0.000520944533000761,-0.00295442325903663,-0.0210189377942895));
#41848=CARTESIAN_POINT('',(-7.21785956780367E-17,-1.27270338476863E-17,
-0.00540230489496124));
#41849=CARTESIAN_POINT('',(0.000520944533000761,-0.00295442325903663,-0.0110189377942895));
#41850=CARTESIAN_POINT('',(0.00104188906600159,-0.00590884651807325,-0.0166355706936178));
#41851=CARTESIAN_POINT('',(0.00104188906600159,-0.00590884651807325,-0.0210189377942895));
#41852=CARTESIAN_POINT('',(0.00104188906600159,-0.00590884651807325,-0.0176355706936178));
#41853=CARTESIAN_POINT('',(-0.000232183409974364,0.00131677755180391,-0.0176355706936178));
#41854=CARTESIAN_POINT('',(0.000763638087699379,-0.00433080680353719,-0.0176355706936178));
#41855=CARTESIAN_POINT('',(-7.21785956780367E-17,-1.27270338476863E-17,
-0.00940230489496124));
#41856=CARTESIAN_POINT('',(0.000520944533000761,-0.00295442325903663,-0.0150189377942895));
#41857=CARTESIAN_POINT('',(0.000520944533000761,-0.00295442325903663,-0.0210189377942895));
#41858=CARTESIAN_POINT('',(0.,0.,-0.0210189377942895));
#41859=CARTESIAN_POINT('',(0.,0.,-0.0166355706936178));
#41860=CARTESIAN_POINT('',(0.00590884651807325,-0.00104188906600158,-0.0166355706936178));
#41861=CARTESIAN_POINT('',(0.00590884651807325,-0.00104188906600158,-0.0210189377942895));
#41862=CARTESIAN_POINT('',(0.00590884651807325,-0.00104188906600158,-0.0176355706936178));
#41863=CARTESIAN_POINT('',(0.,0.,-0.0176355706936178));
#41864=CARTESIAN_POINT('',(-0.00295442325903663,0.000520944533000792,-0.0210189377942895));
#41865=CARTESIAN_POINT('',(-3.76539462949268E-19,-2.13546141059281E-18,
-0.00540230489496124));
#41866=CARTESIAN_POINT('',(0.00295442325903663,-0.000520944533000792,-0.0110189377942895));
#41867=CARTESIAN_POINT('',(0.00295442325903663,-0.000520944533000792,-0.0210189377942895));
#41868=CARTESIAN_POINT('',(0.00295442325903663,-0.000520944533000792,-0.0150189377942895));
#41869=CARTESIAN_POINT('',(-3.76539462949268E-19,-2.13546141059281E-18,
-0.00940230489496124));
#41870=CARTESIAN_POINT('',(0.00433080680353719,-0.00076363808769939,-0.0176355706936178));
#41871=CARTESIAN_POINT('',(-0.00746781659002575,0.00131677755180382,-0.0176355706936178));
#41872=CARTESIAN_POINT('',(0.,0.,-0.0210189377942895));
#41873=CARTESIAN_POINT('',(0.,0.,-0.0150189377942895));
#41874=CARTESIAN_POINT('',(0.,0.,-0.0110189377942895));
#41875=CARTESIAN_POINT('',(0.000520944533000761,-0.00295442325903663,-0.0210189377942895));
#41876=CARTESIAN_POINT('',(3.02167789598882E-17,5.32803340073238E-18,-0.00540230489496124));
#41877=CARTESIAN_POINT('',(-0.000520944533000782,0.00295442325903663,-0.0110189377942895));
#41878=CARTESIAN_POINT('',(-0.00104188906600159,0.00590884651807325,-0.0166355706936178));
#41879=CARTESIAN_POINT('',(-0.00104188906600159,0.00590884651807325,-0.0210189377942895));
#41880=CARTESIAN_POINT('',(-0.00104188906600159,0.00590884651807325,-0.0176355706936178));
#41881=CARTESIAN_POINT('',(-0.00023218340997424,0.00131677755180388,-0.0176355706936178));
#41882=CARTESIAN_POINT('',(-0.000763638087699389,0.00433080680353718,-0.0176355706936178));
#41883=CARTESIAN_POINT('',(3.02167789598882E-17,5.32803340073238E-18,-0.00940230489496124));
#41884=CARTESIAN_POINT('',(-0.000520944533000782,0.00295442325903663,-0.0150189377942895));
#41885=CARTESIAN_POINT('',(-0.000520944533000782,0.00295442325903663,-0.0210189377942895));
#41886=CARTESIAN_POINT('',(0.,0.,-0.0210189377942895));
#41887=CARTESIAN_POINT('',(0.,0.,-0.0166355706936178));
#41888=CARTESIAN_POINT('',(-0.00590884651807325,0.00104188906600158,-0.0166355706936178));
#41889=CARTESIAN_POINT('',(-0.00590884651807325,0.00104188906600158,-0.0210189377942895));
#41890=CARTESIAN_POINT('',(-0.00590884651807325,0.00104188906600158,-0.0176355706936178));
#41891=CARTESIAN_POINT('',(0.,0.,-0.0176355706936178));
#41892=CARTESIAN_POINT('',(-0.00295442325903663,0.000520944533000792,-0.0210189377942895));
#41893=CARTESIAN_POINT('',(3.76539462949268E-19,2.13546141059281E-18,-0.00540230489496124));
#41894=CARTESIAN_POINT('',(-0.00295442325903663,0.000520944533000792,-0.0110189377942895));
#41895=CARTESIAN_POINT('',(-0.00295442325903663,0.000520944533000792,-0.0210189377942895));
#41896=CARTESIAN_POINT('',(-0.00295442325903663,0.000520944533000792,-0.0150189377942895));
#41897=CARTESIAN_POINT('',(3.76539462949268E-19,2.13546141059281E-18,-0.00940230489496124));
#41898=CARTESIAN_POINT('',(-0.00433080680353719,0.00076363808769939,-0.0176355706936178));
#41899=CARTESIAN_POINT('',(-0.00746781659002575,0.00131677755180382,-0.0176355706936178));
#41900=CARTESIAN_POINT('',(0.,0.,-0.0210189377942895));
#41901=CARTESIAN_POINT('',(0.,0.,-0.0150189377942895));
#41902=CARTESIAN_POINT('',(0.,0.,-0.0110189377942895));
#41903=CARTESIAN_POINT('',(-0.00180420299878392,0.,-0.0150189377942895));
#41904=CARTESIAN_POINT('',(0.,0.,-0.0150189377942895));
#41905=CARTESIAN_POINT('',(-0.00180420299878392,0.,-0.0150189377942895));
#41906=CARTESIAN_POINT('',(0.,0.,-0.0150189377942895));
#41907=CARTESIAN_POINT('',(0.,0.,-0.0150189377942895));
#41908=CARTESIAN_POINT('',(0.,0.,-0.0150189377942895));
#41909=CARTESIAN_POINT('',(0.,0.,-0.0150189377942895));
#41910=CARTESIAN_POINT('',(-0.0077,0.,-0.0176355706936178));
#41911=CARTESIAN_POINT('',(0.,0.,-0.0176355706936178));
#41912=CARTESIAN_POINT('',(-0.0077,0.,-0.0176355706936178));
#41913=CARTESIAN_POINT('',(0.,0.,-0.0176355706936178));
#41914=CARTESIAN_POINT('',(0.,0.,-0.0176355706936178));
#41915=CARTESIAN_POINT('',(0.,0.,-0.0176355706936178));
#41916=CARTESIAN_POINT('',(0.,0.,-0.0176355706936178));
#41917=CARTESIAN_POINT('',(-0.008,0.,-0.0166355706936178));
#41918=CARTESIAN_POINT('',(0.,0.,-0.0166355706936178));
#41919=CARTESIAN_POINT('',(-0.008,0.,-0.0166355706936178));
#41920=CARTESIAN_POINT('',(0.,0.,-0.0166355706936178));
#41921=CARTESIAN_POINT('',(0.,0.,-0.0166355706936178));
#41922=CARTESIAN_POINT('',(0.,0.,-0.0166355706936178));
#41923=CARTESIAN_POINT('',(0.,0.,-0.0166355706936178));
#41924=CARTESIAN_POINT('',(-0.003,0.,-0.0110189377942895));
#41925=CARTESIAN_POINT('',(0.,0.,-0.0110189377942895));
#41926=CARTESIAN_POINT('',(0.,0.,-0.0110189377942895));
#41927=CARTESIAN_POINT('',(0.,0.,-0.0110189377942895));
#41928=CARTESIAN_POINT('',(0.,0.,-0.0110189377942895));
#41929=CARTESIAN_POINT('',(0.,0.,-0.0110189377942895));
#41930=CARTESIAN_POINT('',(-0.00180420299878392,0.,-0.0110189377942895));
#41931=CARTESIAN_POINT('',(0.,0.,-0.0150189377942895));
#41932=CARTESIAN_POINT('',(0.,0.,-0.0150189377942895));
#41933=CARTESIAN_POINT('',(0.,0.,-0.0150189377942895));
#41934=CARTESIAN_POINT('',(0.,0.,-0.0166355706936178));
#41935=CARTESIAN_POINT('',(0.,0.,-0.0166355706936178));
#41936=CARTESIAN_POINT('',(0.,0.,-0.0166355706936178));
#41937=CARTESIAN_POINT('',(0.,0.,-0.0300923697749146));
#41938=CARTESIAN_POINT('',(0.,0.,-0.0166355706936178));
#41939=CARTESIAN_POINT('',(0.,0.,-0.0300923697749146));
#41940=CARTESIAN_POINT('',(0.,0.,-0.0173355706936178));
#41941=CARTESIAN_POINT('',(-0.008,0.,-0.0173355706936178));
#41942=CARTESIAN_POINT('',(0.,0.,-0.0173355706936178));
#41943=CARTESIAN_POINT('',(0.,0.,-0.0150189377942895));
#41944=CARTESIAN_POINT('',(0.,0.,0.0238076302250854));
#41945=CARTESIAN_POINT('',(0.0135274197783234,0.0136559722321699,0.044681301720925));
#41946=CARTESIAN_POINT('',(0.0135383476416825,0.0136533363661855,0.0446112569865791));
#41947=CARTESIAN_POINT('',(0.0135507663442154,0.0136510730091971,0.0445355922223623));
#41948=CARTESIAN_POINT('',(0.0135793099051906,0.0136514390447496,0.0443921469902879));
#41949=CARTESIAN_POINT('',(0.0135905144371587,0.0136521608730817,0.0443390104257923));
#41950=CARTESIAN_POINT('',(0.0136202080437242,0.0136581861183181,0.0442206495600809));
#41951=CARTESIAN_POINT('',(0.0136379804308225,0.0136624072587615,0.0441533771102119));
#41952=CARTESIAN_POINT('',(0.0136649436921374,0.0136770530453923,0.0440953250454317));
#41953=CARTESIAN_POINT('',(0.0137591216979031,0.0135793490080381,0.0449376690887614));
#41954=CARTESIAN_POINT('',(0.0137955294557406,0.0135840244482818,0.044914581390673));
#41955=CARTESIAN_POINT('',(0.0138333620004707,0.0135966273451604,0.04489665312379));
#41956=CARTESIAN_POINT('',(0.0138821413352717,0.0136375372183026,0.0448929276695706));
#41957=CARTESIAN_POINT('',(0.0138977270969142,0.0136560593344022,0.0448960471700173));
#41958=CARTESIAN_POINT('',(0.0139209788879496,0.0137061451050335,0.0449176882817704));
#41959=CARTESIAN_POINT('',(0.0139284648226078,0.0137390765639426,0.0449375945732147));
#41960=CARTESIAN_POINT('',(0.0139245922828118,0.0137803595242899,0.0449696705691722));
#41961=CARTESIAN_POINT('',(0.0138718493710985,0.0133075760157319,0.0451344253785385));
#41962=CARTESIAN_POINT('',(0.0139238880279802,0.0132619733864548,0.0451212971220347));
#41963=CARTESIAN_POINT('',(0.0139802559536868,0.0132132977462015,0.0451071500355097));
#41964=CARTESIAN_POINT('',(0.0140916894400597,0.0131247754923386,0.0450799876902406));
#41965=CARTESIAN_POINT('',(0.0141335589045852,0.0130924063246476,0.0450698729824398));
#41966=CARTESIAN_POINT('',(0.0142313592568437,0.01302462045826,0.0450470959743368));
#41967=CARTESIAN_POINT('',(0.0142878782764567,0.0129864541955381,0.0450340100292577));
#41968=CARTESIAN_POINT('',(0.014346765827375,0.0129670186229265,0.0450227345929722));
#41969=CARTESIAN_POINT('',(0.014346765827375,0.0129670186229265,0.0450227345929722));
#41970=CARTESIAN_POINT('',(0.0142289907255384,0.0130058897681498,0.0450452854655432));
#41971=CARTESIAN_POINT('',(0.0140326505124449,0.0131746342432835,0.0450947923168716));
#41972=CARTESIAN_POINT('',(0.0139238880279802,0.0132619733864548,0.0451212971220347));
#41973=CARTESIAN_POINT('',(0.0138718493710985,0.0133075760157319,0.0451344253785385));
#41974=CARTESIAN_POINT('',(0.0138718493710985,0.0133075760157319,0.0451344253785385));
#41975=CARTESIAN_POINT('',(0.014346765827375,0.0129670186229265,0.0450227345929722));
#41976=CARTESIAN_POINT('',(0.0132248054813652,0.0127029266810005,0.0446699542964051));
#41977=CARTESIAN_POINT('',(0.0135274197783234,0.0136559722321699,0.044681301720925));
#41978=CARTESIAN_POINT('',(0.0136653071058316,0.0136772649389237,0.0440945308487834));
#41979=CARTESIAN_POINT('',(0.0136256373571829,0.0136555971622692,0.0441800375577949));
#41980=CARTESIAN_POINT('',(0.0135751070889845,0.0136444699217395,0.0443756388757358));
#41981=CARTESIAN_POINT('',(0.0135274210106334,0.0136559761133743,0.0446813017670743));
#41982=CARTESIAN_POINT('',(0.0136658374374733,0.0136775045728404,0.0440948376110462));
#41983=CARTESIAN_POINT('',(0.0143467558525134,0.0129670108776811,0.0450226952968607));
#41984=CARTESIAN_POINT('',(0.0143015465745449,0.0130541036653512,0.0450170051989192));
#41985=CARTESIAN_POINT('',(0.0141568573863817,0.0132997211390049,0.0449524875713156));
#41986=CARTESIAN_POINT('',(0.0140077224005055,0.0134863714630881,0.0447938026846776));
#41987=CARTESIAN_POINT('',(0.0138687740643729,0.0136139860601651,0.044580075342522));
#41988=CARTESIAN_POINT('',(0.01377445274251,0.0136755825517951,0.0444016168251007));
#41989=CARTESIAN_POINT('',(0.0136973975352464,0.0136900403740722,0.0442047157383087));
#41990=CARTESIAN_POINT('',(0.0136648649317818,0.0136771029055344,0.0440951738724241));
#41991=CARTESIAN_POINT('',(0.014105046329742,0.0127793291184313,0.0440704771345536));
#41992=CARTESIAN_POINT('',(0.0136667248958405,0.0136780328466249,0.0440944206993372));
#41993=CARTESIAN_POINT('',(0.0136861745689291,0.0136861421671065,0.0441460977181257));
#41994=CARTESIAN_POINT('',(0.0137287539986456,0.0136962243778536,0.0442503416155328));
#41995=CARTESIAN_POINT('',(0.0138254982236743,0.0136720093947,0.044436272884352));
#41996=CARTESIAN_POINT('',(0.013894272333865,0.0136395602741699,0.0445501271419491));
#41997=CARTESIAN_POINT('',(0.0140067954073001,0.0135525740966713,0.0447011391172071));
#41998=CARTESIAN_POINT('',(0.0140483773118853,0.0135136202857098,0.0447487234029328));
#41999=CARTESIAN_POINT('',(0.0141167481244794,0.0134440767451732,0.04482159174837));
#42000=CARTESIAN_POINT('',(0.0141793305834479,0.0133692749075648,0.0448758648631172));
#42001=CARTESIAN_POINT('',(0.0142269874670527,0.0133090276484192,0.0449131690072696));
#42002=CARTESIAN_POINT('',(0.0143333169163945,0.013155955993812,0.0449771088685464));
#42003=CARTESIAN_POINT('',(0.0143845245824868,0.0130657505275901,0.044988523237714));
#42004=CARTESIAN_POINT('',(0.0144087800451138,0.0130212016472391,0.0449922205233206));
#42005=CARTESIAN_POINT('',(0.0144088164060123,0.0130212306025444,0.0449923308680604));
#42006=CARTESIAN_POINT('',(0.0144087800451138,0.0130212016472391,0.0449922205233206));
#42007=CARTESIAN_POINT('',(0.0143883014579014,0.0130038037933579,0.0450035339760893));
#42008=CARTESIAN_POINT('',(0.0143676124044562,0.0129856909365987,0.0450137192723785));
#42009=CARTESIAN_POINT('',(0.0143467558525134,0.0129670108776811,0.0450226952968608));
#42010=CARTESIAN_POINT('',(0.0143543358721172,0.0129734997731774,0.0450223912595732));
#42011=CARTESIAN_POINT('',(0.0142498869604617,0.0131740311774407,0.0450086019078322));
#42012=CARTESIAN_POINT('',(0.0141071842607483,0.0133876340631727,0.0449084250872999));
#42013=CARTESIAN_POINT('',(0.0138413738506828,0.0136573423337213,0.0445489378073578));
#42014=CARTESIAN_POINT('',(0.0137286338022633,0.0137025434390836,0.0443029940318597));
#42015=CARTESIAN_POINT('',(0.0136626755570935,0.0136761558919233,0.0440873901519572));
#42016=CARTESIAN_POINT('',(0.0145100291225004,0.013109903869032,0.0449364853455191));
#42017=CARTESIAN_POINT('',(0.0143981204627331,0.0132993225006228,0.0449155041230904));
#42018=CARTESIAN_POINT('',(0.0142374830299031,0.0134883269982029,0.0448187565584134));
#42019=CARTESIAN_POINT('',(0.0139151016581816,0.0137039062309166,0.0444926329796269));
#42020=CARTESIAN_POINT('',(0.0137645876753501,0.013722544285296,0.0442739751078847));
#42021=CARTESIAN_POINT('',(0.0136641876361022,0.0136770327619371,0.0440804304725095));
#42022=CARTESIAN_POINT('',(0.0146565930206288,0.0132401123010691,0.0448110693510974));
#42023=CARTESIAN_POINT('',(0.0145353397028751,0.0134178028227805,0.0447873548684827));
#42024=CARTESIAN_POINT('',(0.0143562676911,0.0135837736709856,0.0447005316646434));
#42025=CARTESIAN_POINT('',(0.0139812259277474,0.0137490376643148,0.0444203306717967));
#42026=CARTESIAN_POINT('',(0.0137970658203665,0.0137425238909612,0.0442352488688624));
#42027=CARTESIAN_POINT('',(0.0136655812754718,0.0136779519004114,0.0440700642907236));
#42028=CARTESIAN_POINT('',(0.0148561869420901,0.0134245298225879,0.0444401372985064));
#42029=CARTESIAN_POINT('',(0.0147202361893934,0.0135851348071275,0.0444253746420989));
#42030=CARTESIAN_POINT('',(0.014514736203999,0.0137195113669646,0.0443775701105716));
#42031=CARTESIAN_POINT('',(0.0140682376951201,0.0138148735734959,0.0442272197318363));
#42032=CARTESIAN_POINT('',(0.0138397494067089,0.0137724753618642,0.0441285697805939));
#42033=CARTESIAN_POINT('',(0.0136672108305557,0.0136795271082228,0.0440391292696259));
#42034=CARTESIAN_POINT('',(0.0149102056749342,0.0134789301609788,0.0442095873452684));
#42035=CARTESIAN_POINT('',(0.0147697219839977,0.0136345088744832,0.0442047360754924));
#42036=CARTESIAN_POINT('',(0.0145566753949533,0.0137600265713512,0.044183579961384));
#42037=CARTESIAN_POINT('',(0.01409085414887,0.0138352218867532,0.0441124227906861));
#42038=CARTESIAN_POINT('',(0.0138507650317711,0.0137820491623528,0.0440642589994173));
#42039=CARTESIAN_POINT('',(0.0136674754888846,0.0136801592884,0.0440198285274441));
#42040=CARTESIAN_POINT('',(0.0149021535947794,0.0134874946220255,0.0437414750071867));
#42041=CARTESIAN_POINT('',(0.0147620013685623,0.0136426853747751,0.043756733998497));
#42042=CARTESIAN_POINT('',(0.0145498776236904,0.013767193588292,0.0437896627013868));
#42043=CARTESIAN_POINT('',(0.0140868194117618,0.0138394359615844,0.0438793233746439));
#42044=CARTESIAN_POINT('',(0.0138484956243084,0.0137843974750378,0.0439336850792973));
#42045=CARTESIAN_POINT('',(0.0136667755709176,0.013680850707678,0.0439806208483835));
#42046=CARTESIAN_POINT('',(0.0148408481024395,0.0134420273546197,0.0435127120710071));
#42047=CARTESIAN_POINT('',(0.0147055074066387,0.0136018084704029,0.0435378464395097));
#42048=CARTESIAN_POINT('',(0.0145017549573871,0.0137340910675512,0.0435972739054557));
#42049=CARTESIAN_POINT('',(0.0140605129996015,0.0138234042994072,0.0437655308068245));
#42050=CARTESIAN_POINT('',(0.0138353874056037,0.013777210507569,0.0438699383119697));
#42051=CARTESIAN_POINT('',(0.0136658319590425,0.0136809004841067,0.0439614578877055));
#42052=CARTESIAN_POINT('',(0.0146288177262632,0.013271447945054,0.0431420114315051));
#42053=CARTESIAN_POINT('',(0.0145084480711531,0.0134479229339361,0.0431762790242411));
#42054=CARTESIAN_POINT('',(0.0143324238504282,0.0136102716028767,0.0432749864733467));
#42055=CARTESIAN_POINT('',(0.0139669857610103,0.0137646036720782,0.0435731045341093));
#42056=CARTESIAN_POINT('',(0.0137890792080722,0.0137511116143412,0.0437636448274475));
#42057=CARTESIAN_POINT('',(0.013663097969023,0.0136804172320355,0.0439304809596632));
#42058=CARTESIAN_POINT('',(0.0144769486791919,0.013145005762609,0.0430154533168616));
#42059=CARTESIAN_POINT('',(0.0143659106593811,0.0133333811663706,0.0430471596869001));
#42060=CARTESIAN_POINT('',(0.0142088058302736,0.0135185141682279,0.0431561613858893));
#42061=CARTESIAN_POINT('',(0.0138979585191121,0.0137217698081853,0.0435006909193419));
#42062=CARTESIAN_POINT('',(0.0137550537397556,0.0137323746885259,0.0437248623853491));
#42063=CARTESIAN_POINT('',(0.0136613139372126,0.0136798578520549,0.0439199607480119));
#42064=CARTESIAN_POINT('',(0.0143182670268424,0.013011683094371,0.0429304918108316));
#42065=CARTESIAN_POINT('',(0.0142144398487442,0.0132114126772654,0.0429551488197019));
#42066=CARTESIAN_POINT('',(0.0140753928366151,0.0134210089472879,0.0430678050943401));
#42067=CARTESIAN_POINT('',(0.0138222829792609,0.013677197407846,0.0434455292881368));
#42068=CARTESIAN_POINT('',(0.0137181015819516,0.0137133992748758,0.0436965210630945));
#42069=CARTESIAN_POINT('',(0.0136595668833152,0.0136792312485303,0.0439130710733126));
#42070=CARTESIAN_POINT('',(0.0143722462106869,0.0130570322249862,0.0429594753784009));
#42071=CARTESIAN_POINT('',(0.0143488177373289,0.0131002062692814,0.0429654421756892));
#42072=CARTESIAN_POINT('',(0.0143064663956776,0.0131728485372548,0.0429817556535115));
#42073=CARTESIAN_POINT('',(0.0142441468438431,0.013269940183715,0.0430178358493532));
#42074=CARTESIAN_POINT('',(0.014176653268755,0.0133632559502267,0.0430702966139033));
#42075=CARTESIAN_POINT('',(0.0141597634282231,0.0133851885762827,0.0430845337421948));
#42076=CARTESIAN_POINT('',(0.0140819711780693,0.0134790357196756,0.0431602339511191));
#42077=CARTESIAN_POINT('',(0.0140279139033517,0.0135334375005743,0.0432248312851544));
#42078=CARTESIAN_POINT('',(0.0139771134946773,0.0135816930189672,0.0432884874805865));
#42079=CARTESIAN_POINT('',(0.0138779116499055,0.0136563552298041,0.0434358682978622));
#42080=CARTESIAN_POINT('',(0.0137833434819359,0.0137000933638628,0.0436056258056102));
#42081=CARTESIAN_POINT('',(0.0136988366239239,0.0137013802102704,0.043800906436155));
#42082=CARTESIAN_POINT('',(0.0136633334931184,0.0136813096353833,0.0439059502094003));
#42083=CARTESIAN_POINT('',(0.0136624515029435,0.0136808390639733,0.0439055621987736));
#42084=CARTESIAN_POINT('',(0.01437226696962,0.0130570532827275,0.0429594045199949));
#42085=CARTESIAN_POINT('',(0.01437226696962,0.0130570532827275,0.0429594045199949));
#42086=CARTESIAN_POINT('',(0.0146717499392492,0.0133086757482844,0.0431197540232505));
#42087=CARTESIAN_POINT('',(0.0148987545636125,0.0134914264033247,0.0435343329240457));
#42088=CARTESIAN_POINT('',(0.0149061886432635,0.0134832026201001,0.0439760606041642));
#42089=CARTESIAN_POINT('',(0.0149061886621837,0.0134832026369253,0.043976060604159));
#42090=CARTESIAN_POINT('',(0.0149061886432635,0.0134832026201001,0.0439760606041642));
#42091=CARTESIAN_POINT('',(0.0149136041538308,0.0134749993785061,0.0444166849226565));
#42092=CARTESIAN_POINT('',(0.0147019253362106,0.013278025669204,0.0448306039434562));
#42093=CARTESIAN_POINT('',(0.0144088164060122,0.0130212306025443,0.0449923308680605));
#42094=CARTESIAN_POINT('',(0.0136618759636351,0.0136805582427143,0.0439058480849644));
#42095=CARTESIAN_POINT('',(0.0136762744475629,0.0136866778567627,0.0439408460490943));
#42096=CARTESIAN_POINT('',(0.0136785483540271,0.0136846917340837,0.0440583127451966));
#42097=CARTESIAN_POINT('',(0.0136652248748306,0.013677224092152,0.0440945546229615));
#42098=CARTESIAN_POINT('',(0.0141018423856368,0.012782736153729,0.0438824700191097));
#42099=CARTESIAN_POINT('',(0.0136615152461314,0.0136804379623559,0.0439052547308507));
#42100=CARTESIAN_POINT('',(0.0136896569272057,0.0136969637596643,0.0437980033320951));
#42101=CARTESIAN_POINT('',(0.0137528858452649,0.0136935190147541,0.0436143884579431));
#42102=CARTESIAN_POINT('',(0.0138468528121099,0.0136371892690744,0.0434158218904349));
#42103=CARTESIAN_POINT('',(0.0139473868333189,0.0135469564206017,0.0432442411871308));
#42104=CARTESIAN_POINT('',(0.0140414782289585,0.0134368471581768,0.0431210525142315));
#42105=CARTESIAN_POINT('',(0.0141699419719539,0.0132607029984888,0.0429892353980327));
#42106=CARTESIAN_POINT('',(0.0142655458067999,0.0130945904910373,0.0429410276813476));
#42107=CARTESIAN_POINT('',(0.0143115126415105,0.013005915311329,0.0429303643960295));
#42108=CARTESIAN_POINT('',(0.0143115133909795,0.0130059161090858,0.0429303609927156));
#42109=CARTESIAN_POINT('',(0.0143115126415105,0.013005915311329,0.0429303643960295));
#42110=CARTESIAN_POINT('',(0.0143319072137059,0.0130235212915782,0.0429389825816724));
#42111=CARTESIAN_POINT('',(0.0143521649453348,0.0130406035866204,0.0429487100267025));
#42112=CARTESIAN_POINT('',(0.0143722462106869,0.0130570322249862,0.0429594753784009));
#42113=CARTESIAN_POINT('',(0.0138344560634004,0.0133469119961904,0.0428477145766624));
#42114=CARTESIAN_POINT('',(0.013886971005638,0.0133011649381436,0.0428574018561204));
#42115=CARTESIAN_POINT('',(0.0139438740787491,0.013252321577593,0.0428678503498006));
#42116=CARTESIAN_POINT('',(0.0140559810540401,0.0131637316702822,0.0428879083042912));
#42117=CARTESIAN_POINT('',(0.0140980505445236,0.0131313782827532,0.0428953757342894));
#42118=CARTESIAN_POINT('',(0.0141960853061902,0.01306368791893,0.042912215084704));
#42119=CARTESIAN_POINT('',(0.0142526252182071,0.0130257039963108,0.0429218802990572));
#42120=CARTESIAN_POINT('',(0.0143115133909795,0.0130059161090858,0.0429303609927156));
#42121=CARTESIAN_POINT('',(0.0137278240280471,0.0136129157959791,0.0430583504712026));
#42122=CARTESIAN_POINT('',(0.0137649908061728,0.013617058002644,0.0430801705136134));
#42123=CARTESIAN_POINT('',(0.0138033385422682,0.0136293033632107,0.0430970391927033));
#42124=CARTESIAN_POINT('',(0.0138520538399427,0.0136703266625429,0.0431003684914596));
#42125=CARTESIAN_POINT('',(0.0138674524027168,0.0136890038261722,0.0430973409796219));
#42126=CARTESIAN_POINT('',(0.0138898631504268,0.0137398103119725,0.0430767697306566));
#42127=CARTESIAN_POINT('',(0.0138966556662956,0.0137733367122553,0.0430579265936399));
#42128=CARTESIAN_POINT('',(0.0138918161470185,0.0138156031282396,0.0430276581554502));
#42129=CARTESIAN_POINT('',(0.0135040802168541,0.013679486763382,0.0433266840430606));
#42130=CARTESIAN_POINT('',(0.0135175127884876,0.0136744672531597,0.0433960521860028));
#42131=CARTESIAN_POINT('',(0.0135326432571359,0.0136696332551146,0.0434710039130298));
#42132=CARTESIAN_POINT('',(0.01356619801545,0.0136651356705284,0.0436126800003295));
#42133=CARTESIAN_POINT('',(0.0135792417840673,0.0136640591417054,0.04366509795279));
#42134=CARTESIAN_POINT('',(0.0136129108043982,0.0136660366205628,0.043781672082727));
#42135=CARTESIAN_POINT('',(0.0136329175571453,0.0136679793370068,0.0438477716337234));
#42136=CARTESIAN_POINT('',(0.0136615731878359,0.0136804198319751,0.0439051085754789));
#42137=CARTESIAN_POINT('',(0.0135040830062575,0.0136794957015745,0.04332668415021));
#42138=CARTESIAN_POINT('',(0.0135623712422786,0.0136576965251136,0.0436277204281935));
#42139=CARTESIAN_POINT('',(0.0136194652626658,0.0136620381699811,0.04382077118711));
#42140=CARTESIAN_POINT('',(0.0136619480096978,0.013680592991384,0.0439058672119058));
#42141=CARTESIAN_POINT('',(0.0135040802168541,0.013679486763382,0.0433266840430606));
#42142=CARTESIAN_POINT('',(0.0132063607148604,0.0127249017189299,0.0433152607755814));
#42143=CARTESIAN_POINT('',(0.0138344560634004,0.0133469119961904,0.0428477145766624));
#42144=CARTESIAN_POINT('',(0.0138344560634004,0.0133469119961904,0.0428477145766624));
#42145=CARTESIAN_POINT('',(0.013886971005638,0.0133011649381436,0.0428574018561204));
#42146=CARTESIAN_POINT('',(0.0139968700990166,0.0132131948679319,0.0428770439081624));
#42147=CARTESIAN_POINT('',(0.0141937370454347,0.0130454918835358,0.0429133996053987));
#42148=CARTESIAN_POINT('',(0.0143115133909795,0.0130059161090858,0.0429303609927156));
#42149=CARTESIAN_POINT('',(0.0133472984199313,0.0138340105634861,0.0361523640312129));
#42150=CARTESIAN_POINT('',(0.0133015007188745,0.0138865737234961,0.0361426658713359));
#42151=CARTESIAN_POINT('',(0.0132526083035492,0.013943522820677,0.0361322064277899));
#42152=CARTESIAN_POINT('',(0.0131639195283671,0.0140557264582103,0.0361121250269432));
#42153=CARTESIAN_POINT('',(0.0131315285880089,0.0140978328998557,0.0361046485389464));
#42154=CARTESIAN_POINT('',(0.0130637485736462,0.0141959634642915,0.0360877864006782));
#42155=CARTESIAN_POINT('',(0.0130257052961867,0.0142525630871666,0.0360781066097589));
#42156=CARTESIAN_POINT('',(0.0130058820419269,0.0143115230386036,0.0360696121138117));
#42157=CARTESIAN_POINT('',(0.0136128985927667,0.0137274518465749,0.0359418834605835));
#42158=CARTESIAN_POINT('',(0.0136169976274488,0.0137646732519322,0.0359199974709124));
#42159=CARTESIAN_POINT('',(0.0136292072606399,0.0138030888752574,0.0359030588909682));
#42160=CARTESIAN_POINT('',(0.0136702118163053,0.0138519200410911,0.0358996434566288));
#42161=CARTESIAN_POINT('',(0.0136888896648635,0.013867362410277,0.0359026444980052));
#42162=CARTESIAN_POINT('',(0.013739724994142,0.0138898605074415,0.0359231850985355));
#42163=CARTESIAN_POINT('',(0.0137732834801289,0.0138966982922935,0.035942026510332));
#42164=CARTESIAN_POINT('',(0.0138156107733477,0.0138918841669157,0.0359723251855485));
#42165=CARTESIAN_POINT('',(0.0136795294309768,0.0135039659523988,0.0356739008696862));
#42166=CARTESIAN_POINT('',(0.0136744997547652,0.0135174052624958,0.0356044661013661));
#42167=CARTESIAN_POINT('',(0.0136696558812933,0.0135325422766957,0.0355294490737307));
#42168=CARTESIAN_POINT('',(0.0136651420516113,0.0135661141628188,0.0353876400937255));
#42169=CARTESIAN_POINT('',(0.0136640597498046,0.0135791648240051,0.0353351716791691));
#42170=CARTESIAN_POINT('',(0.0136660274088303,0.0136128553332629,0.0352184742547098));
#42171=CARTESIAN_POINT('',(0.0136679631605594,0.0136328748127337,0.0351522974473094));
#42172=CARTESIAN_POINT('',(0.0136804125989053,0.0136615584408772,0.0350948893411197));
#42173=CARTESIAN_POINT('',(0.0136795440116764,0.0135039705136565,0.0356739006950023));
#42174=CARTESIAN_POINT('',(0.0136576885637337,0.0135622930115568,0.0353725345390528));
#42175=CARTESIAN_POINT('',(0.0136620275076353,0.0136194309372824,0.0351792878769671));
#42176=CARTESIAN_POINT('',(0.013680590999552,0.0136619306474012,0.0350941304125763));
#42177=CARTESIAN_POINT('',(0.0136795294309768,0.0135039659523988,0.0356739008696862));
#42178=CARTESIAN_POINT('',(0.013680831805632,0.0136624368944392,0.0350944355572129));
#42179=CARTESIAN_POINT('',(0.0127251061247038,0.0132057278958406,0.0356853119610551));
#42180=CARTESIAN_POINT('',(0.0133472984199313,0.0138340105634861,0.0361523640312129));
#42181=CARTESIAN_POINT('',(0.0133472984199313,0.0138340105634861,0.0361523640312129));
#42182=CARTESIAN_POINT('',(0.0133015007188745,0.0138865737234961,0.0361426658713359));
#42183=CARTESIAN_POINT('',(0.0132134502721952,0.0139965620617856,0.0361230041659299));
#42184=CARTESIAN_POINT('',(0.0130455285504465,0.0141936031357296,0.036086601105706));
#42185=CARTESIAN_POINT('',(0.0130058820419269,0.0143115230386036,0.0360696121138117));
#42186=CARTESIAN_POINT('',(0.0130058820419269,0.0143115230386036,0.0360696121138117));
#42187=CARTESIAN_POINT('',(0.0136804181869855,0.0136615064351884,0.0350947435404781));
#42188=CARTESIAN_POINT('',(0.0136845235441635,0.0136685117358603,0.0351214207542266));
#42189=CARTESIAN_POINT('',(0.0136962282247815,0.0137000990348768,0.0352319296825527));
#42190=CARTESIAN_POINT('',(0.0136867456212001,0.0137598515039631,0.0353955166288276));
#42191=CARTESIAN_POINT('',(0.0136444877520215,0.0138371855745404,0.0355651180311228));
#42192=CARTESIAN_POINT('',(0.0135938073861743,0.0138960677545512,0.0356688188803307));
#42193=CARTESIAN_POINT('',(0.0135566115191702,0.0139338748518138,0.0357288873200465));
#42194=CARTESIAN_POINT('',(0.0135433243902175,0.0139477100689181,0.0357513741953739));
#42195=CARTESIAN_POINT('',(0.0134294743133418,0.0140491444249602,0.0358910536670735));
#42196=CARTESIAN_POINT('',(0.0132581698826406,0.0141702913522595,0.0360077693277889));
#42197=CARTESIAN_POINT('',(0.0131050840320944,0.0142604570193312,0.0360585865159813));
#42198=CARTESIAN_POINT('',(0.0130061230521812,0.0143117701294611,0.0360705462182175));
#42199=CARTESIAN_POINT('',(0.0127820780883721,0.0141004771635773,0.035118051426175));
#42200=CARTESIAN_POINT('',(0.0130571681490899,0.0143724345256651,0.0360411286159117));
#42201=CARTESIAN_POINT('',(0.0131586168026541,0.0143173938115839,0.0360271105881626));
#42202=CARTESIAN_POINT('',(0.0133072254508839,0.0142232987437342,0.0359753879151188));
#42203=CARTESIAN_POINT('',(0.0134710348387075,0.0140916428982257,0.0358532903722309));
#42204=CARTESIAN_POINT('',(0.0135804170390299,0.0139801761974099,0.0357169716746656));
#42205=CARTESIAN_POINT('',(0.0136326038833519,0.0139121394107367,0.0356176123714242));
#42206=CARTESIAN_POINT('',(0.0136832257137762,0.0138229436469999,0.0354673177967897));
#42207=CARTESIAN_POINT('',(0.0137067063451301,0.0137410934370739,0.0353033719092715));
#42208=CARTESIAN_POINT('',(0.0136906404678223,0.0136798085372556,0.0351428401614667));
#42209=CARTESIAN_POINT('',(0.0136813031815613,0.0136633182575446,0.0350940474800154));
#42210=CARTESIAN_POINT('',(0.0130570107031178,0.0143722892292046,0.0360405596727561));
#42211=CARTESIAN_POINT('',(0.0130061230521812,0.0143117701294611,0.0360705462182175));
#42212=CARTESIAN_POINT('',(0.013023153596727,0.0143320069448286,0.0360607990551864));
#42213=CARTESIAN_POINT('',(0.0130401689831634,0.0143522282196738,0.0360509931426053));
#42214=CARTESIAN_POINT('',(0.0130571681490899,0.0143724345256651,0.0360411286159117));
#42215=CARTESIAN_POINT('',(0.0136808846299159,0.0136626724049009,0.0350920767725914));
#42216=CARTESIAN_POINT('',(0.0137210587275886,0.0137327886228891,0.0353000717275669));
#42217=CARTESIAN_POINT('',(0.0136904388863567,0.013851178063408,0.0355407663640888));
#42218=CARTESIAN_POINT('',(0.0134518098416119,0.01412260861273,0.0359035690516185));
#42219=CARTESIAN_POINT('',(0.0132517178337988,0.014266656880963,0.0360136694568607));
#42220=CARTESIAN_POINT('',(0.0130570107031176,0.0143722892292045,0.0360405596727562));
#42221=CARTESIAN_POINT('',(0.0136833127453435,0.0136683630339632,0.0350775860037388));
#42222=CARTESIAN_POINT('',(0.0137578650624181,0.0138044516106767,0.0352453746898784));
#42223=CARTESIAN_POINT('',(0.0137756675930909,0.0139953767732017,0.0354357476721513));
#42224=CARTESIAN_POINT('',(0.0136361532731369,0.014374592085454,0.0357368350948862));
#42225=CARTESIAN_POINT('',(0.0134817097350188,0.0145523279540323,0.035840266790345));
#42226=CARTESIAN_POINT('',(0.013308276944001,0.0146714608170859,0.035880362789578));
#42227=CARTESIAN_POINT('',(0.0136848811056226,0.0136729254478668,0.0350399692792684));
#42228=CARTESIAN_POINT('',(0.0137884825402338,0.0138528162957767,0.0351270500570564));
#42229=CARTESIAN_POINT('',(0.0138412758209031,0.0140905644001273,0.0352265946513145));
#42230=CARTESIAN_POINT('',(0.0137686281604507,0.0145492335926007,0.0353863968047801));
#42231=CARTESIAN_POINT('',(0.0136449518885705,0.0147591260207492,0.0354428150544384));
#42232=CARTESIAN_POINT('',(0.0134907921550379,0.0148982458255525,0.035466872082957));
#42233=CARTESIAN_POINT('',(0.0136834729528892,0.0136743637179171,0.0349598820818488));
#42234=CARTESIAN_POINT('',(0.0137840697280492,0.0138573385894591,0.0348757439524089));
#42235=CARTESIAN_POINT('',(0.0138334867729773,0.0140985532290686,0.0347830222095031));
#42236=CARTESIAN_POINT('',(0.0137555551293985,0.0145626385773065,0.0346424679496524));
#42237=CARTESIAN_POINT('',(0.0136300982234556,0.0147743494085679,0.0345980112820943));
#42238=CARTESIAN_POINT('',(0.0134752693808984,0.0149141454522923,0.0345843997163447));
#42239=CARTESIAN_POINT('',(0.0136805664818357,0.013671129001264,0.0349221271846283));
#42240=CARTESIAN_POINT('',(0.0137492535815907,0.0138131869707248,0.0347567882305654));
#42241=CARTESIAN_POINT('',(0.0137604582150299,0.0140108221137018,0.0345728698062549));
#42242=CARTESIAN_POINT('',(0.0136106422372575,0.0144005004670435,0.0342906828321895));
#42243=CARTESIAN_POINT('',(0.0134527417753365,0.0145817376785579,0.0341992056888346));
#42244=CARTESIAN_POINT('',(0.0132780514912236,0.0147021303845673,0.0341695534475961));
#42245=CARTESIAN_POINT('',(0.0136776403141161,0.0136659840267521,0.0349076015771296));
#42246=CARTESIAN_POINT('',(0.0137105256774238,0.013743550391952,0.0347009641812863));
#42247=CARTESIAN_POINT('',(0.0136715341765596,0.0138704942959491,0.0344658839028819));
#42248=CARTESIAN_POINT('',(0.0134204397438091,0.0141546429885548,0.0341216605741726));
#42249=CARTESIAN_POINT('',(0.013216668455911,0.0143024318724588,0.0340239118433991));
#42250=CARTESIAN_POINT('',(0.0130211889517766,0.0144088376077831,0.0340077073858473));
#42251=CARTESIAN_POINT('',(0.0136780272519456,0.0136667095752855,0.034905581586559));
#42252=CARTESIAN_POINT('',(0.0136964143905424,0.0137108187410915,0.034788422276699));
#42253=CARTESIAN_POINT('',(0.0136871620300887,0.0137953137079372,0.0346141668762517));
#42254=CARTESIAN_POINT('',(0.0136344884354508,0.0139000958670438,0.0344408365435239));
#42255=CARTESIAN_POINT('',(0.0135187620029207,0.0140539445911384,0.0342340356476201));
#42256=CARTESIAN_POINT('',(0.0133752357840903,0.0141802709063995,0.0341154657696032));
#42257=CARTESIAN_POINT('',(0.0131875796217974,0.014312480999393,0.0340340228098608));
#42258=CARTESIAN_POINT('',(0.0130829292098404,0.0143751763364855,0.0340129423431057));
#42259=CARTESIAN_POINT('',(0.0130211600827906,0.0144088013426358,0.0340078173960094));
#42260=CARTESIAN_POINT('',(0.0130211889517765,0.014408837607783,0.0340077073858472));
#42261=CARTESIAN_POINT('',(0.0136774973922645,0.0136658227481176,0.0349051645484567));
#42262=CARTESIAN_POINT('',(0.0136805537788317,0.0136618534337557,0.0350941516620443));
#42263=CARTESIAN_POINT('',(0.0136866691123424,0.0136762766325689,0.0350585201494323));
#42264=CARTESIAN_POINT('',(0.0136846746348222,0.0136785276008497,0.0349410108658378));
#42265=CARTESIAN_POINT('',(0.0136772282532725,0.013665211620951,0.034905449744478));
#42266=CARTESIAN_POINT('',(0.0130570107031176,0.0143722892292045,0.0360405596727562));
#42267=CARTESIAN_POINT('',(0.0133086060896628,0.0146718527161954,0.0358801529400381));
#42268=CARTESIAN_POINT('',(0.0134912320100738,0.0148988005893567,0.0354656660584956));
#42269=CARTESIAN_POINT('',(0.0134829993621013,0.014906225830457,0.0350239020087959));
#42270=CARTESIAN_POINT('',(0.013482999374259,0.0149062258439255,0.0350239020087958));
#42271=CARTESIAN_POINT('',(0.0134829993621013,0.014906225830457,0.0350239020087959));
#42272=CARTESIAN_POINT('',(0.0134747882545363,0.0149136316436989,0.0345832938205633));
#42273=CARTESIAN_POINT('',(0.0132777150147689,0.0147017461863572,0.0341693414377258));
#42274=CARTESIAN_POINT('',(0.0130211889517766,0.0144088376077831,0.0340077073858473));
#42275=CARTESIAN_POINT('',(0.0127792840555328,0.0141049572874922,0.0349295269758739));
#42276=CARTESIAN_POINT('',(0.0129669779043646,0.0143467645108084,0.0339773326375768));
#42277=CARTESIAN_POINT('',(0.0130263712183109,0.0143159396828672,0.0339812121960737));
#42278=CARTESIAN_POINT('',(0.0131233024692379,0.0142619016732827,0.0339979765471674));
#42279=CARTESIAN_POINT('',(0.0133261805475022,0.014133467545687,0.0340761972002906));
#42280=CARTESIAN_POINT('',(0.0135327339226899,0.0139708977511429,0.034245498563561));
#42281=CARTESIAN_POINT('',(0.0136832637964497,0.0137783721189361,0.0345773538662836));
#42282=CARTESIAN_POINT('',(0.0136908619908576,0.0136994685495474,0.0347882996132415));
#42283=CARTESIAN_POINT('',(0.0136770973445796,0.0136648493060317,0.0349048280955806));
#42284=CARTESIAN_POINT('',(0.0129669855780655,0.0143467743968879,0.0339772937079336));
#42285=CARTESIAN_POINT('',(0.0130211600827905,0.0144088013426356,0.0340078173960093));
#42286=CARTESIAN_POINT('',(0.0130032141795775,0.0143887737309074,0.0339965058562739));
#42287=CARTESIAN_POINT('',(0.0129851441896491,0.0143680468565852,0.0339863181194242));
#42288=CARTESIAN_POINT('',(0.0129669779043646,0.0143467645108084,0.0339773326375768));
#42289=CARTESIAN_POINT('',(0.0136559709074652,0.0135274255875118,0.0343187419294822));
#42290=CARTESIAN_POINT('',(0.0136533354668889,0.0135383536079546,0.0343887876498067));
#42291=CARTESIAN_POINT('',(0.0136510727552833,0.0135507726180141,0.0344644536835966));
#42292=CARTESIAN_POINT('',(0.0136514396594344,0.0135793138736788,0.0346078900124016));
#42293=CARTESIAN_POINT('',(0.0136521618108376,0.0135905171703827,0.0346610215461767));
#42294=CARTESIAN_POINT('',(0.0136581861359256,0.0136202052928602,0.0347793667883587));
#42295=CARTESIAN_POINT('',(0.0136624070632991,0.0136379739909101,0.0348466263114605));
#42296=CARTESIAN_POINT('',(0.0136770458879545,0.0136649288717871,0.0349046769298396));
#42297=CARTESIAN_POINT('',(0.0135793479802516,0.0137591529406104,0.0340623518581221));
#42298=CARTESIAN_POINT('',(0.0135840255876753,0.0137955634488069,0.034085439643062));
#42299=CARTESIAN_POINT('',(0.0135966310722218,0.0138333983907062,0.034103367183507));
#42300=CARTESIAN_POINT('',(0.0136375435327623,0.0138821833286537,0.0341070916759763));
#42301=CARTESIAN_POINT('',(0.0136560661394879,0.0138977713670621,0.0341039719527325));
#42302=CARTESIAN_POINT('',(0.0137061521383977,0.0139210308957088,0.0340823310548747));
#42303=CARTESIAN_POINT('',(0.0137390831725555,0.0139285228044378,0.0340624255868605));
#42304=CARTESIAN_POINT('',(0.0137803679828772,0.0139246596653472,0.0340303480415716));
#42305=CARTESIAN_POINT('',(0.0133075405240295,0.0138718879877591,0.0338655879802315));
#42306=CARTESIAN_POINT('',(0.013261936505332,0.0139239282081985,0.0338787180408429));
#42307=CARTESIAN_POINT('',(0.0132132593539372,0.0139802980185987,0.0338928674419205));
#42308=CARTESIAN_POINT('',(0.0131247399461771,0.0140917265396258,0.0339200333078431));
#42309=CARTESIAN_POINT('',(0.0130923728023401,0.0141335928811781,0.0339301491716137));
#42310=CARTESIAN_POINT('',(0.0130245918254165,0.0142313819201084,0.0339529285104976));
#42311=CARTESIAN_POINT('',(0.0129864308401398,0.0142878918202987,0.0339660153368474));
#42312=CARTESIAN_POINT('',(0.0129669855780655,0.0143467743968879,0.0339772937079336));
#42313=CARTESIAN_POINT('',(0.0129669855780655,0.0143467743968879,0.0339772937079336));
#42314=CARTESIAN_POINT('',(0.0130058761022141,0.0142290092437095,0.0339547369657612));
#42315=CARTESIAN_POINT('',(0.0131745865270879,0.014032698672613,0.0339052285351024));
#42316=CARTESIAN_POINT('',(0.013261936505332,0.0139239282081985,0.0338787180408429));
#42317=CARTESIAN_POINT('',(0.0133075405240295,0.0138718879877591,0.0338655879802315));
#42318=CARTESIAN_POINT('',(0.0133075405240295,0.0138718879877591,0.0338655879802315));
#42319=CARTESIAN_POINT('',(0.0127029149047374,0.0132248442373881,0.0343300901276774));
#42320=CARTESIAN_POINT('',(0.0136559709074652,0.0135274255875118,0.0343187419294822));
#42321=CARTESIAN_POINT('',(0.0136772662261439,0.0136652880999797,0.034905471069399));
#42322=CARTESIAN_POINT('',(0.0136556034899632,0.0136256284900497,0.0348199584719417));
#42323=CARTESIAN_POINT('',(0.01364447616907,0.0135751090501954,0.0346243712334455));
#42324=CARTESIAN_POINT('',(0.0136559727524311,0.0135274261730563,0.0343187419075286));
#42325=CARTESIAN_POINT('',(0.0152484657348856,0.0119111184403255,0.0338775863652793));
#42326=CARTESIAN_POINT('',(0.0151858258403965,0.011863360894658,0.0338569113318196));
#42327=CARTESIAN_POINT('',(0.0151277492026445,0.0118233336388945,0.0337656702120796));
#42328=CARTESIAN_POINT('',(0.0151254208358762,0.0118263115356238,0.0336843209195344));
#42329=CARTESIAN_POINT('',(0.0140382448373698,0.0134200696350122,0.0339611627334923));
#42330=CARTESIAN_POINT('',(0.0139873849465785,0.0133719181325723,0.0339320759062046));
#42331=CARTESIAN_POINT('',(0.013946293602799,0.0133349847830113,0.0338490484243907));
#42332=CARTESIAN_POINT('',(0.0139442238483378,0.0133370193734124,0.0337743619960435));
#42333=CARTESIAN_POINT('',(0.012658314481834,0.0147477052200364,0.0339896961860576));
#42334=CARTESIAN_POINT('',(0.0126090750223232,0.0146912370440514,0.0339654793180963));
#42335=CARTESIAN_POINT('',(0.0125657496565872,0.0146441278057015,0.0338778657456314));
#42336=CARTESIAN_POINT('',(0.0125642362393917,0.0146454221589132,0.0337995083619698));
#42337=CARTESIAN_POINT('',(0.00947688983191456,0.0169674284533521,0.0340865237787356));
#42338=CARTESIAN_POINT('',(0.00943997017358526,0.0169025023035178,0.0340621287700834));
#42339=CARTESIAN_POINT('',(0.00940709426201283,0.0168480005019376,0.0339747164540596));
#42340=CARTESIAN_POINT('',(0.0094054067916901,0.016848939004426,0.0338965239761736));
#42341=CARTESIAN_POINT('',(0.00775668729563145,0.0178191849284778,0.0341321851044574));
#42342=CARTESIAN_POINT('',(0.00772625457732441,0.0177506916439944,0.0341079928666602));
#42343=CARTESIAN_POINT('',(0.00769879493364172,0.0176928379308047,0.0340203470976657));
#42344=CARTESIAN_POINT('',(0.0076970813710619,0.0176935893561103,0.0339419630479391));
#42345=CARTESIAN_POINT('',(0.00408418112072838,0.0190005651886774,0.0342268669996844));
#42346=CARTESIAN_POINT('',(0.00406782135904743,0.0189272920959749,0.0342027738260244));
#42347=CARTESIAN_POINT('',(0.00405216994910225,0.0188649907657062,0.0341150197824115));
#42348=CARTESIAN_POINT('',(0.00405023404477903,0.0188654120049874,0.0340365471169725));
#42349=CARTESIAN_POINT('',(0.00216840361041831,0.0193117419450391,0.0342754880779789));
#42350=CARTESIAN_POINT('',(0.00215946952635624,0.0192374761738103,0.0342511839953137));
#42351=CARTESIAN_POINT('',(0.0021501921059827,0.0191743297555034,0.0341636686442656));
#42352=CARTESIAN_POINT('',(0.00214825046287373,0.0191745448583638,0.0340853917257764));
#42353=CARTESIAN_POINT('',(-0.00167360332837079,0.0193610642126229,0.0343700481021553));
#42354=CARTESIAN_POINT('',(-0.00166772909682775,0.019286428417166,0.0343457939093161));
#42355=CARTESIAN_POINT('',(-0.00166433877537794,0.0192225967005017,0.0342582198830898));
#42356=CARTESIAN_POINT('',(-0.00166623630989755,0.0192224297927247,0.0341798947461287));
#42357=CARTESIAN_POINT('',(-0.00361133617940907,0.0190948158684411,0.0344168625248252));
#42358=CARTESIAN_POINT('',(-0.00359794478513623,0.0190209413594288,0.0343927734792581));
#42359=CARTESIAN_POINT('',(-0.00358812593142569,0.0189574520910898,0.0343050135695173));
#42360=CARTESIAN_POINT('',(-0.00359004364584992,0.0189570900562084,0.0342265360377781));
#42361=CARTESIAN_POINT('',(-0.00728829361639954,0.0180142515371123,0.0345124729173908));
#42362=CARTESIAN_POINT('',(-0.00726075726241988,0.0179446383412048,0.0344882166245085));
#42363=CARTESIAN_POINT('',(-0.00723881613136299,0.0178846073086646,0.0344006473284614));
#42364=CARTESIAN_POINT('',(-0.00724064639673391,0.0178838674937992,0.0343223262238402));
#42365=CARTESIAN_POINT('',(-0.00906929804333343,0.0171862126464738,0.034560762512631));
#42366=CARTESIAN_POINT('',(-0.00903491514989842,0.0171197972123796,0.0345364495681483));
#42367=CARTESIAN_POINT('',(-0.00900705233761316,0.0170623997824801,0.034448942961856));
#42368=CARTESIAN_POINT('',(-0.00900874957067781,0.0170615031751766,0.0343706731538278));
#42369=CARTESIAN_POINT('',(-0.0122631905137826,0.0150748786324861,0.0346543869518873));
#42370=CARTESIAN_POINT('',(-0.0122163203849323,0.0150163415921938,0.0346302290363188));
#42371=CARTESIAN_POINT('',(-0.0121775450826729,0.0149652889674267,0.0345425456877034));
#42372=CARTESIAN_POINT('',(-0.0121790274739666,0.0149640819702418,0.0344641308966256));
#42373=CARTESIAN_POINT('',(-0.0137228510447306,0.0137592215827943,0.0347027838593881));
#42374=CARTESIAN_POINT('',(-0.0136703742361262,0.0137057774186251,0.0346785581107913));
#42375=CARTESIAN_POINT('',(-0.0136267651763594,0.0136589664244109,0.0345909540909438));
#42376=CARTESIAN_POINT('',(-0.0136281597039386,0.0136575719060068,0.0345126044943345));
#42377=CARTESIAN_POINT('',(-0.0161549996488971,0.0107998100077384,0.034797946258462));
#42378=CARTESIAN_POINT('',(-0.0160931630832887,0.0107577795404196,0.0347736188837651));
#42379=CARTESIAN_POINT('',(-0.0160413585894283,0.0107205833515088,0.0346861292106204));
#42380=CARTESIAN_POINT('',(-0.0160424287014922,0.0107189779662681,0.0346078733006445));
#42381=CARTESIAN_POINT('',(-0.0171612867006073,0.00911837226548826,0.0348448845895495));
#42382=CARTESIAN_POINT('',(-0.0170953462354564,0.00908269155364083,0.0348207145277423));
#42383=CARTESIAN_POINT('',(-0.0170397742567095,0.00905078118993255,0.0347330443100082));
#42384=CARTESIAN_POINT('',(-0.0170406643333398,0.00904911376884754,0.0346546402390712));
#42385=CARTESIAN_POINT('',(-0.018618876747511,0.00556775154408273,0.0349392970584412));
#42386=CARTESIAN_POINT('',(-0.0185471385013646,0.00554568163233485,0.0349151903208354));
#42387=CARTESIAN_POINT('',(-0.0184862866589607,0.00552519255369288,0.0348274513429876));
#42388=CARTESIAN_POINT('',(-0.0184868552108964,0.00552330384230827,0.0347489910210362));
#42389=CARTESIAN_POINT('',(-0.01908252879493,0.00367700453617041,0.0349880241107599));
#42390=CARTESIAN_POINT('',(-0.0190091993532158,0.00366227237929489,0.0349637137267457));
#42391=CARTESIAN_POINT('',(-0.0189469864824965,0.00364807081817205,0.0348762056218833));
#42392=CARTESIAN_POINT('',(-0.0189473534850118,0.00364615087558417,0.0347979346472256));
#42393=CARTESIAN_POINT('',(-0.0194330429780207,-0.000159071216011557,0.0350828838010445));
#42394=CARTESIAN_POINT('',(-0.0193581952805587,-0.000159034107970636,0.0350586138052778));
#42395=CARTESIAN_POINT('',(-0.0192943233846616,-0.000160631300607095,0.0349710578392802));
#42396=CARTESIAN_POINT('',(-0.0192943049086593,-0.000162537334766749,0.034892747516314));
#42397=CARTESIAN_POINT('',(-0.019323220858512,-0.00208279330176897,0.0351290854614679));
#42398=CARTESIAN_POINT('',(-0.0192485540725893,-0.00207532108809656,0.0351049608609899));
#42399=CARTESIAN_POINT('',(-0.0191845482294334,-0.00207058909152159,0.0350172412926273));
#42400=CARTESIAN_POINT('',(-0.0191843388777613,-0.00207253258253173,0.0349387968701855));
#42401=CARTESIAN_POINT('',(-0.018526423896832,-0.00587164369870195,0.035225609788055));
#42402=CARTESIAN_POINT('',(-0.0184549150235699,-0.00584958997299527,0.0352013255107728));
#42403=CARTESIAN_POINT('',(-0.0183934136736763,-0.00583237202561983,0.0351137878656332));
#42404=CARTESIAN_POINT('',(-0.0183928195717425,-0.0058342469680116,0.0350354927017894));
#42405=CARTESIAN_POINT('',(-0.0178587922177036,-0.00766578380247021,0.0352724553485967));
#42406=CARTESIAN_POINT('',(-0.017789822465766,-0.00763681873606203,0.0352481492370294));
#42407=CARTESIAN_POINT('',(-0.0177303624302418,-0.0076136257508411,0.0351606344733825));
#42408=CARTESIAN_POINT('',(-0.0177296077983877,-0.00761538266113453,0.0350823579657423));
#42409=CARTESIAN_POINT('',(-0.0159857063641824,-0.0110535861634857,0.0353669496908954));
#42410=CARTESIAN_POINT('',(-0.0159236482423738,-0.0110113827549873,0.0353428313428075));
#42411=CARTESIAN_POINT('',(-0.0158696595078198,-0.0109766550493149,0.0352551031157736));
#42412=CARTESIAN_POINT('',(-0.0158685715064848,-0.010978227730547,0.0351766515074452));
#42413=CARTESIAN_POINT('',(-0.0148111911879068,-0.0125819195993878,0.0354145067676068));
#42414=CARTESIAN_POINT('',(-0.0147537039270021,-0.0125338506107053,0.0353903052149494));
#42415=CARTESIAN_POINT('',(-0.0147035220233913,-0.0124940841885928,0.0353026737935011));
#42416=CARTESIAN_POINT('',(-0.0147022403647437,-0.0124955888864539,0.0352243017315574));
#42417=CARTESIAN_POINT('',(-0.0120387344173888,-0.0152554388784305,0.0355103574544654));
#42418=CARTESIAN_POINT('',(-0.0119919676073606,-0.0151971041221094,0.0354860257152941));
#42419=CARTESIAN_POINT('',(-0.0119508100978304,-0.0151483938894718,0.0353985411397392));
#42420=CARTESIAN_POINT('',(-0.0119492905153562,-0.0151495897482933,0.0353202894208755));
#42421=CARTESIAN_POINT('',(-0.010451420680373,-0.0163834982989298,0.0355570836717863));
#42422=CARTESIAN_POINT('',(-0.0104106338065928,-0.0163206205454677,0.0355328929543693));
#42423=CARTESIAN_POINT('',(-0.010374434674129,-0.0162677917784069,0.0354452462963411));
#42424=CARTESIAN_POINT('',(-0.0103728406094323,-0.0162688127609957,0.0353668615585341));
#42425=CARTESIAN_POINT('',(-0.00702795570842145,-0.0181180930152355,0.0356515539846757));
#42426=CARTESIAN_POINT('',(-0.00700027756530127,-0.0180483744095495,0.0356274130424822));
#42427=CARTESIAN_POINT('',(-0.00697504988780368,-0.0179894030893777,0.0355397127643222));
#42428=CARTESIAN_POINT('',(-0.00697321301761058,-0.017990119265087,0.0354612841950215));
#42429=CARTESIAN_POINT('',(-0.00516713643770654,-0.0187328837046514,0.0357004746702459));
#42430=CARTESIAN_POINT('',(-0.00514668355624036,-0.0186609611650446,0.035676151543525));
#42431=CARTESIAN_POINT('',(-0.00512764139888409,-0.0186000854485199,0.0355886577116004));
#42432=CARTESIAN_POINT('',(-0.00512576324307812,-0.0186006006840196,0.0355103984279492));
#42433=CARTESIAN_POINT('',(-0.00139218102196667,-0.0193827829215529,0.0357945730344739));
#42434=CARTESIAN_POINT('',(-0.00138624224911403,-0.0193081403307028,0.0357703296806507));
#42435=CARTESIAN_POINT('',(-0.00137954992248072,-0.0192445505752173,0.0356827431915192));
#42436=CARTESIAN_POINT('',(-0.0013776523864038,-0.0192446841629754,0.0356044078293643));
#42437=CARTESIAN_POINT('',(0.000572588218934399,-0.0194246737866148,0.035841714022483));
#42438=CARTESIAN_POINT('',(0.000570947370553278,-0.019349620051212,0.0358176203178043));
#42439=CARTESIAN_POINT('',(0.000571210769109811,-0.0192853859213364,0.0357298658608833));
#42440=CARTESIAN_POINT('',(0.000573167396785734,-0.0192853284395788,0.0356513928178601));
#42441=CARTESIAN_POINT('',(0.00436973798898508,-0.018934846936721,0.0359372961428186));
#42442=CARTESIAN_POINT('',(0.00435347581480306,-0.0188617958776991,0.0359130232916096));
#42443=CARTESIAN_POINT('',(0.00434123413948511,-0.0187990977995665,0.0358254727273128));
#42444=CARTESIAN_POINT('',(0.0043431547027079,-0.0187986547687731,0.0357471669804605));
#42445=CARTESIAN_POINT('',(0.00625864225674502,-0.018397160611825,0.0359854747050194));
#42446=CARTESIAN_POINT('',(0.00623511134760215,-0.0183261678087875,0.0359611636278828));
#42447=CARTESIAN_POINT('',(0.00621660098285804,-0.0182651048018455,0.0358736547360438));
#42448=CARTESIAN_POINT('',(0.00621841450216693,-0.0182644872522259,0.03579538304732));
#42449=CARTESIAN_POINT('',(0.00974796227618663,-0.016811426961068,0.0360791583163149));
#42450=CARTESIAN_POINT('',(0.00971084419310295,-0.0167462530048705,0.0360550101091685));
#42451=CARTESIAN_POINT('',(0.00968054611933654,-0.0166897336117225,0.0359673158108602));
#42452=CARTESIAN_POINT('',(0.00968220133754792,-0.0166887731953749,0.0358888920411454));
#42453=CARTESIAN_POINT('',(0.0113882717487478,-0.0157468141669751,0.0361274222318138));
#42454=CARTESIAN_POINT('',(0.0113448598901736,-0.0156857881408525,0.0361031878926111));
#42455=CARTESIAN_POINT('',(0.0113091654394432,-0.0156327125443483,0.0360155936464992));
#42456=CARTESIAN_POINT('',(0.0113107615506835,-0.0156315548533139,0.0359372520648063));
#42457=CARTESIAN_POINT('',(0.0142638915192683,-0.0131979063047583,0.0362228199557271));
#42458=CARTESIAN_POINT('',(0.0142093998765725,-0.0131467035594434,0.0361984945903921));
#42459=CARTESIAN_POINT('',(0.0141640569778619,-0.0131018477396012,0.0361110025320489));
#42460=CARTESIAN_POINT('',(0.0141653634357823,-0.0131004317761201,0.0360327446597237));
#42461=CARTESIAN_POINT('',(0.0155099871775632,-0.011710480490977,0.0362692166595979));
#42462=CARTESIAN_POINT('',(0.0154504782693005,-0.0116648392026414,0.036245060107269));
#42463=CARTESIAN_POINT('',(0.0154006067027975,-0.0116245513559714,0.0361573745561721));
#42464=CARTESIAN_POINT('',(0.015401748510621,-0.0116230458123332,0.0360789579026339));
#42465=CARTESIAN_POINT('',(0.0175178637361487,-0.00841573059787445,0.0363642600524374));
#42466=CARTESIAN_POINT('',(0.0174504761001674,-0.00838269957389024,0.0363401437162083));
#42467=CARTESIAN_POINT('',(0.0173936016377699,-0.00835293382421085,0.0362524158765654));
#42468=CARTESIAN_POINT('',(0.0173944625462095,-0.00835115105051529,0.0361739647082496));
#42469=CARTESIAN_POINT('',(0.0182624515796345,-0.006648377091405,0.0364122382904254));
#42470=CARTESIAN_POINT('',(0.0181923746561503,-0.00662223604375927,0.036387923067016));
#42471=CARTESIAN_POINT('',(0.0181331939085809,-0.00659837938135913,0.0363004203966629));
#42472=CARTESIAN_POINT('',(0.0181338591348402,-0.0065965437312554,0.0362221538738593));
#42473=CARTESIAN_POINT('',(0.0192194486591489,-0.00288751225102433,0.0365077284567637));
#42474=CARTESIAN_POINT('',(0.01914550312317,-0.00287582042360165,0.0364834668324474));
#42475=CARTESIAN_POINT('',(0.0190826491640174,-0.00286423331881863,0.0363959012744127));
#42476=CARTESIAN_POINT('',(0.0190829294130007,-0.00286234891985882,0.0363175830830445));
#42477=CARTESIAN_POINT('',(0.0194098491272683,-0.000982580873600955,0.036553695077945));
#42478=CARTESIAN_POINT('',(0.0193349437255172,-0.000978214703617675,0.0365295661903181));
#42479=CARTESIAN_POINT('',(0.0192710001663832,-0.000972817108818172,0.0364418515882359));
#42480=CARTESIAN_POINT('',(0.0192710989915557,-0.000970861653981333,0.0363634112480515));
#42481=CARTESIAN_POINT('',(0.0192202056017125,0.00287588470824289,0.0366500242217906));
#42482=CARTESIAN_POINT('',(0.0191461244303748,0.00286538714458625,0.0366257326413781));
#42483=CARTESIAN_POINT('',(0.0190826930320087,0.00285808453264583,0.0365382032286708));
#42484=CARTESIAN_POINT('',(0.0190824022057189,0.00286002705453847,0.0364599148108454));
#42485=CARTESIAN_POINT('',(0.0188379106547843,0.0047734665138793,0.0366973166700389));
#42486=CARTESIAN_POINT('',(0.018765251017742,0.00475566014909327,0.036673017774804));
#42487=CARTESIAN_POINT('',(0.0187028830749146,0.00474206184380905,0.0365854946832061));
#42488=CARTESIAN_POINT('',(0.0187024138420233,0.00474391283128575,0.0365072113414088));
#42489=CARTESIAN_POINT('',(0.0175295655931796,0.00838993396492618,0.0367911918806325));
#42490=CARTESIAN_POINT('',(0.0174616178458993,0.00835805890798054,0.0367670802579245));
#42491=CARTESIAN_POINT('',(0.0174028132235672,0.00833229126715749,0.036679344518385));
#42492=CARTESIAN_POINT('',(0.0174019863583542,0.008334018433673,0.0366008867507613));
#42493=CARTESIAN_POINT('',(0.0165984266245079,0.0101061561823627,0.0368394726457053));
#42494=CARTESIAN_POINT('',(0.0165341336245753,0.0100676948925726,0.0368152604792397));
#42495=CARTESIAN_POINT('',(0.0164783622620697,0.0100362923655943,0.0367276411189044));
#42496=CARTESIAN_POINT('',(0.0164773324201164,0.0100379785673599,0.036649278948126));
#42497=CARTESIAN_POINT('',(0.0142905353273534,0.0131684358682503,0.0369348355464337));
#42498=CARTESIAN_POINT('',(0.0142351661563029,0.0131181958780369,0.0369105048728009));
#42499=CARTESIAN_POINT('',(0.0141868524427726,0.0130765746613298,0.0368230189991468));
#42500=CARTESIAN_POINT('',(0.0141855420207472,0.0130779927733353,0.0367447662090692));
#42501=CARTESIAN_POINT('',(0.0128895188291006,0.0145429059113914,0.0369818752438031));
#42502=CARTESIAN_POINT('',(0.0128393736391177,0.0144871840945391,0.0369576976771935));
#42503=CARTESIAN_POINT('',(0.0127953290097661,0.0144406609758556,0.0368700360789205));
#42504=CARTESIAN_POINT('',(0.0127939152942572,0.0144419190605648,0.0367916390825784));
#42505=CARTESIAN_POINT('',(0.00978786991559796,0.0167879924321533,0.0370762585418591));
#42506=CARTESIAN_POINT('',(0.00974958535440995,0.0167235036723632,0.0370521074471736));
#42507=CARTESIAN_POINT('',(0.0097154094364033,0.016669251743918,0.0369644189414872));
#42508=CARTESIAN_POINT('',(0.00971370211163489,0.0166702515276451,0.0368860000449194));
#42509=CARTESIAN_POINT('',(0.00804166596354184,0.0176903828787484,0.0371252845413655));
#42510=CARTESIAN_POINT('',(0.00801018587904991,0.0176225629513854,0.0371009582456875));
#42511=CARTESIAN_POINT('',(0.00798183457162373,0.0175654329761448,0.0370134679189905));
#42512=CARTESIAN_POINT('',(0.00798006309091339,0.0175662353813498,0.0369352115046535));
#42513=CARTESIAN_POINT('',(0.0044163194260252,0.0189242184549924,0.0372192839751649));
#42514=CARTESIAN_POINT('',(0.00439873869692677,0.0188514198959119,0.0371950506017007));
#42515=CARTESIAN_POINT('',(0.0043821463774674,0.0187896490582238,0.0371074527101591));
#42516=CARTESIAN_POINT('',(0.00438029403874385,0.0187900786731213,0.0370291079952339));
#42517=CARTESIAN_POINT('',(0.00248610588398672,0.0192737620343253,0.0372664223567425));
#42518=CARTESIAN_POINT('',(0.00247593541563535,0.0191993875068387,0.0372423237815989));
#42519=CARTESIAN_POINT('',(0.00246558189748319,0.0191360009975268,0.0371545749507012));
#42520=CARTESIAN_POINT('',(0.00246363690390784,0.0191362517585942,0.0370761065326615));
#42521=CARTESIAN_POINT('',(-0.00134787560567592,0.0193860391546447,0.0373622032590154));
#42522=CARTESIAN_POINT('',(-0.00134326448971298,0.01931135295845,0.0373379210285972));
#42523=CARTESIAN_POINT('',(-0.00134099918203681,0.0192475283997314,0.0372503810494137));
#42524=CARTESIAN_POINT('',(-0.00134296270095129,0.0192473917543767,0.0371720839782732));
#42525=CARTESIAN_POINT('',(-0.00328486942927988,0.019153728202705,0.0374099693667313));
#42526=CARTESIAN_POINT('',(-0.00327280431272498,0.0190799067467614,0.0373856637145816));
#42527=CARTESIAN_POINT('',(-0.00326413183658672,0.0190166788604113,0.0372981485277988));
#42528=CARTESIAN_POINT('',(-0.00326601750557292,0.0190163551594814,0.0372198716721568));
#42529=CARTESIAN_POINT('',(-0.00699439582431333,0.0181316033959343,0.0375040151627022));
#42530=CARTESIAN_POINT('',(-0.00696794173589825,0.018061407895021,0.0374798741828622));
#42531=CARTESIAN_POINT('',(-0.0069468685444334,0.018000823563801,0.0373921717860003));
#42532=CARTESIAN_POINT('',(-0.00694865640299855,0.0180001335575965,0.037313741377107));
#42533=CARTESIAN_POINT('',(-0.00876107696796061,0.0173476846701873,0.0375518061498425));
#42534=CARTESIAN_POINT('',(-0.00872784348875839,0.0172805784608766,0.0375275629593083));
#42535=CARTESIAN_POINT('',(-0.00870097863415649,0.0172225469740549,0.0374399787779819));
#42536=CARTESIAN_POINT('',(-0.00870273685794072,0.0172216558340193,0.0373616454492075));
#42537=CARTESIAN_POINT('',(-0.0120213318765713,0.0152701046479567,0.0376477120444383));
#42538=CARTESIAN_POINT('',(-0.0119755279397664,0.0152109928382331,0.0376233891251002));
#42539=CARTESIAN_POINT('',(-0.0119377636830074,0.0151595828288496,0.0375358941828318));
#42540=CARTESIAN_POINT('',(-0.0119392736272278,0.0151583905391748,0.0374576339393092));
#42541=CARTESIAN_POINT('',(-0.0134661942258329,0.0140140920121328,0.0376934022305724));
#42542=CARTESIAN_POINT('',(-0.0134146259061713,0.0139596103567137,0.0376692590059635));
#42543=CARTESIAN_POINT('',(-0.0133717221338478,0.0139119318098514,0.0375815583359552));
#42544=CARTESIAN_POINT('',(-0.0133730874184949,0.0139106261003993,0.037503129276001));
#42545=CARTESIAN_POINT('',(-0.0159800261710854,0.0110622696501474,0.0377890510435331));
#42546=CARTESIAN_POINT('',(-0.0159186701493929,0.0110190736210227,0.0377649234054599));
#42547=CARTESIAN_POINT('',(-0.0158671939734713,0.0109807538574401,0.0376772086356948));
#42548=CARTESIAN_POINT('',(-0.0158683286817252,0.0109791224811712,0.0375987682063429));
#42549=CARTESIAN_POINT('',(-0.0169927014477256,0.00942964358742211,0.0378370711676181));
#42550=CARTESIAN_POINT('',(-0.0169275999860674,0.00939284044147255,0.0378127520470631));
#42551=CARTESIAN_POINT('',(-0.0168729023629467,0.00936000506277512,0.0377252537200097));
#42552=CARTESIAN_POINT('',(-0.0168738459564173,0.00935829903214214,0.0376469907536258));
#42553=CARTESIAN_POINT('',(-0.0185202330766905,0.00588892750320043,0.0379318849520895));
#42554=CARTESIAN_POINT('',(-0.0184490597344988,0.00586569177572236,0.0379076315446938));
#42555=CARTESIAN_POINT('',(-0.0183888161595843,0.00584431082219037,0.03782005659223));
#42556=CARTESIAN_POINT('',(-0.0183893906474437,0.00584249516487678,0.0377417306953401));
#42557=CARTESIAN_POINT('',(-0.0190152816034714,0.00401040540637397,0.0379786358366598));
#42558=CARTESIAN_POINT('',(-0.0189419961223453,0.00399436197687571,0.0379545013168636));
#42559=CARTESIAN_POINT('',(-0.0188797021261493,0.0039790153132323,0.0378667932018171));
#42560=CARTESIAN_POINT('',(-0.0188801063331463,0.00397709655791713,0.0377883581908105));
#42561=CARTESIAN_POINT('',(-0.0194321009153758,0.000192138599558602,0.0380744231692379));
#42562=CARTESIAN_POINT('',(-0.0193573042177216,0.000190819056578032,0.0380501249191978));
#42563=CARTESIAN_POINT('',(-0.0192935315844883,0.000188027198034302,0.0379626030162209));
#42564=CARTESIAN_POINT('',(-0.0192935505188315,0.000186066007663494,0.0378843207510498));
#42565=CARTESIAN_POINT('',(-0.01935245436779,-0.00176338950479553,0.0381221642309786));
#42566=CARTESIAN_POINT('',(-0.0192778947935724,-0.00175718375645641,0.0380978732683488));
#42567=CARTESIAN_POINT('',(-0.0192141536943148,-0.0017535195261046,0.0380103410376233));
#42568=CARTESIAN_POINT('',(-0.0192139807220376,-0.00175541870492419,0.0379320501962032));
#42569=CARTESIAN_POINT('',(-0.0186307898171988,-0.00552669110195807,0.0382157044502257));
#42570=CARTESIAN_POINT('',(-0.0185586670123005,-0.00550590460021261,0.038191599349049));
#42571=CARTESIAN_POINT('',(-0.0184965293375801,-0.00548971177913334,0.0381038563465176));
#42572=CARTESIAN_POINT('',(-0.0184959839749268,-0.00549155049286511,0.0380253926248339));
#42573=CARTESIAN_POINT('',(-0.0179766003326881,-0.00737942712623029,0.0382643900908638));
#42574=CARTESIAN_POINT('',(-0.0179070883556642,-0.00735152506121528,0.0382401675413537));
#42575=CARTESIAN_POINT('',(-0.0178471053992343,-0.00732926072206128,0.0381525599762558));
#42576=CARTESIAN_POINT('',(-0.017846352858866,-0.00733108658494678,0.0380742074777779));
#42577=CARTESIAN_POINT('',(-0.0161849938678833,-0.0107539093268891,0.0383593363237856));
#42578=CARTESIAN_POINT('',(-0.0161224057707,-0.0107130134365234,0.0383350073881844));
#42579=CARTESIAN_POINT('',(-0.0160681417269081,-0.0106795156784479,0.0382475194490954));
#42580=CARTESIAN_POINT('',(-0.0160670723710059,-0.0106811200865827,0.0381692649588679));
#42581=CARTESIAN_POINT('',(-0.0150241786357296,-0.0123287368515955,0.0384061484184165));
#42582=CARTESIAN_POINT('',(-0.0149658519529488,-0.0122816050792086,0.0383819847308958));
#42583=CARTESIAN_POINT('',(-0.0149149959562187,-0.0122425879942847,0.03829430730965));
#42584=CARTESIAN_POINT('',(-0.0149138001047669,-0.0122440523050679,0.0382158973270259));
#42585=CARTESIAN_POINT('',(-0.0122807280456702,-0.0150634424110327,0.0385017879912471));
#42586=CARTESIAN_POINT('',(-0.0122328851481888,-0.0150056988755769,0.0384776241054119));
#42587=CARTESIAN_POINT('',(-0.0121906942167475,-0.0149574409602581,0.0383899504553218));
#42588=CARTESIAN_POINT('',(-0.0121891559707154,-0.014958700716832,0.0383115437663749));
#42589=CARTESIAN_POINT('',(-0.0107387574079005,-0.016197932406738,0.0385494815949886));
#42590=CARTESIAN_POINT('',(-0.0106969473711148,-0.0161359401607028,0.0385251524019803));
#42591=CARTESIAN_POINT('',(-0.0106599200181777,-0.0160840104127377,0.0384376652763639));
#42592=CARTESIAN_POINT('',(-0.0106582997137264,-0.0160850815777654,0.0383594114826556));
#42593=CARTESIAN_POINT('',(-0.00731727827992635,-0.0180045813174106,0.0386443821218688));
#42594=CARTESIAN_POINT('',(-0.00728853974211108,-0.0179354004473274,0.0386201592294896));
#42595=CARTESIAN_POINT('',(-0.00726249647480254,-0.0178769524956158,0.0385325493700246));
#42596=CARTESIAN_POINT('',(-0.00726073440225153,-0.0178776659016483,0.0384541948382906));
#42597=CARTESIAN_POINT('',(-0.00549562993204591,-0.0186409126876467,0.0386908155039891));
#42598=CARTESIAN_POINT('',(-0.0054738544920556,-0.0185690779957131,0.0386667116487949));
#42599=CARTESIAN_POINT('',(-0.00545363064055279,-0.0185081268843176,0.0385789688906636));
#42600=CARTESIAN_POINT('',(-0.00545174652657209,-0.0185086819285558,0.03850050546279));
#42601=CARTESIAN_POINT('',(-0.00171297789558108,-0.0193578808109938,0.0387869685227048));
#42602=CARTESIAN_POINT('',(-0.00170580575094533,-0.0192834050608197,0.0387626779532545));
#42603=CARTESIAN_POINT('',(-0.00169802546614798,-0.0192200301102672,0.0386751473835489));
#42604=CARTESIAN_POINT('',(-0.00169606742719998,-0.0192202029699177,0.0385968580236358));
#42605=CARTESIAN_POINT('',(0.000234326520478524,-0.0194314445656357,0.0388345938678207));
#42606=CARTESIAN_POINT('',(0.000234010164348733,-0.0193566380194836,0.0388102946104787));
#42607=CARTESIAN_POINT('',(0.000235377831076791,-0.0192928221301491,0.0387227720368678));
#42608=CARTESIAN_POINT('',(0.000237288513941407,-0.0192927990424999,0.0386444891190078));
#42609=CARTESIAN_POINT('',(0.00404787155173841,-0.0190071440116824,0.0389283814240497));
#42610=CARTESIAN_POINT('',(0.00403281600376,-0.0189336501553832,0.0389042461039105));
#42611=CARTESIAN_POINT('',(0.00402156009123918,-0.0188704913271033,0.0388165373983829));
#42612=CARTESIAN_POINT('',(0.00402343712348825,-0.0188700915325411,0.0387381018186629));
#42613=CARTESIAN_POINT('',(0.00594205675945055,-0.018501902080374,0.038976946540659));
#42614=CARTESIAN_POINT('',(0.00591972441584579,-0.0184304448473425,0.038952694041197));
#42615=CARTESIAN_POINT('',(0.00590226500799304,-0.0183689513755182,0.0388651204286461));
#42616=CARTESIAN_POINT('',(0.00590413947814813,-0.0183683463522363,0.0387867957647425));
#42617=CARTESIAN_POINT('',(0.00945543378881706,-0.0169768884659516,0.0390718896815281));
#42618=CARTESIAN_POINT('',(0.00941955105645558,-0.0169112809125558,0.0390475705383369));
#42619=CARTESIAN_POINT('',(0.00939038642398818,-0.016854546848796,0.0389600712082809));
#42620=CARTESIAN_POINT('',(0.00939206362974605,-0.0168536094492528,0.0388818073612772));
#42621=CARTESIAN_POINT('',(0.0111223087685258,-0.0159353585344843,0.0391187890482724));
#42622=CARTESIAN_POINT('',(0.0110798312243679,-0.0158735148232922,0.0390946605182411));
#42623=CARTESIAN_POINT('',(0.0110448505119366,-0.0158197280398541,0.0390069433294018));
#42624=CARTESIAN_POINT('',(0.0110464049211253,-0.0158186485540586,0.0389285007223895));
#42625=CARTESIAN_POINT('',(0.0140306587396472,-0.0134454521687635,0.0392134074489147));
#42626=CARTESIAN_POINT('',(0.0139769149734139,-0.013393127998949,0.0391892651849783));
#42627=CARTESIAN_POINT('',(0.0139321645237592,-0.0133471836038336,0.0391015671499933));
#42628=CARTESIAN_POINT('',(0.0139335456449393,-0.0133457487432768,0.0390231404614087));
#42629=CARTESIAN_POINT('',(0.0153155581303857,-0.0119607522408212,0.0392624168290426));
#42630=CARTESIAN_POINT('',(0.0152569911307815,-0.0119142632470286,0.0392380940571982));
#42631=CARTESIAN_POINT('',(0.015208082986905,-0.0118733172212726,0.0391505997737426));
#42632=CARTESIAN_POINT('',(0.0152092788797299,-0.011871781703946,0.0390723401171548));
#42633=CARTESIAN_POINT('',(0.0173657491105147,-0.00872162810886881,0.0393565917639802));
#42634=CARTESIAN_POINT('',(0.0172990962157357,-0.00868750783861493,0.0393323481039219));
#42635=CARTESIAN_POINT('',(0.017242940434333,-0.00865693103776873,0.0392447620183172));
#42636=CARTESIAN_POINT('',(0.017243792561054,-0.00865522864971671,0.039166426990155));
#42637=CARTESIAN_POINT('',(0.0181547615587285,-0.0069335040110206,0.039403733158809));
#42638=CARTESIAN_POINT('',(0.0180848927866211,-0.00690620417209522,0.0393795919178693));
#42639=CARTESIAN_POINT('',(0.0180257763837351,-0.00688131022021618,0.0392918915243171));
#42640=CARTESIAN_POINT('',(0.0180264763251293,-0.00687947534514428,0.0392134628550138));
#42641=CARTESIAN_POINT('',(0.0191637763706284,-0.00322453562887558,0.0394995926897395));
#42642=CARTESIAN_POINT('',(0.0190901121570296,-0.00321155341112151,0.0394752871793574));
#42643=CARTESIAN_POINT('',(0.0190275708723674,-0.00319884217617825,0.0393877734491774));
#42644=CARTESIAN_POINT('',(0.0190278950280094,-0.00319691109165435,0.0393094978793444));
#42645=CARTESIAN_POINT('',(0.019390584562046,-0.00129919113440175,0.0395467820100426));
#42646=CARTESIAN_POINT('',(0.0193159596168944,-0.00129360518917694,0.0395224993996629));
#42647=CARTESIAN_POINT('',(0.0192524133638981,-0.00128721042390899,0.0394349575490327));
#42648=CARTESIAN_POINT('',(0.0192525410891745,-0.00128531010501602,0.0393566588132005));
#42649=CARTESIAN_POINT('',(0.0192654480728298,0.00255902747664352,0.0396410321703988));
#42650=CARTESIAN_POINT('',(0.0191909539952961,0.00254972160441421,0.0396169341992129));
#42651=CARTESIAN_POINT('',(0.0191270342322012,0.00254340177096497,0.0395291832721127));
#42652=CARTESIAN_POINT('',(0.0191267815750555,0.00254530686490345,0.0394507130547643));
#42653=CARTESIAN_POINT('',(0.018920683437361,0.00444305374675822,0.0396885804156549));
#42654=CARTESIAN_POINT('',(0.0188476331628076,0.00442650180934002,0.0396643480409234));
#42655=CARTESIAN_POINT('',(0.0187848919764505,0.00441401055138857,0.0395767516461146));
#42656=CARTESIAN_POINT('',(0.0187844377200531,0.00441593205747535,0.0394984083074891));
#42657=CARTESIAN_POINT('',(0.0176595364392572,0.00811552306226673,0.0397849985133176));
#42658=CARTESIAN_POINT('',(0.0175913513792114,0.00808482042028178,0.0397606712460022));
#42659=CARTESIAN_POINT('',(0.0175325381227602,0.00806013414993144,0.0396731812985189));
#42660=CARTESIAN_POINT('',(0.0175317315447527,0.0080618822515282,0.0395949251539854));
#42661=CARTESIAN_POINT('',(0.0167748459587384,0.00981354181841796,0.0398307170263652));
#42662=CARTESIAN_POINT('',(0.0167098246400574,0.00977615831575187,0.0398065649037819));
#42663=CARTESIAN_POINT('',(0.0166534462708234,0.00974561518644464,0.0397188746507484));
#42664=CARTESIAN_POINT('',(0.0166524910438048,0.00974725586583842,0.0396404541567125));
#42665=CARTESIAN_POINT('',(0.0145036323846716,0.0129360948209068,0.039926190043373));
#42666=CARTESIAN_POINT('',(0.0144472907815484,0.012886636570823,0.0399020137013212));
#42667=CARTESIAN_POINT('',(0.01439803453912,0.0128456564564349,0.0398143541368571));
#42668=CARTESIAN_POINT('',(0.0143967148926182,0.0128471419070078,0.0397359590016802));
#42669=CARTESIAN_POINT('',(0.0131425537235162,0.0143150190215106,0.0399743936492381));
#42670=CARTESIAN_POINT('',(0.0130915539773512,0.01426034540911,0.0399500631806892));
#42671=CARTESIAN_POINT('',(0.0130468557902625,0.0142148597033713,0.0398625773915283));
#42672=CARTESIAN_POINT('',(0.0130454255977014,0.0142161695140225,0.0397843246887073));
#42673=CARTESIAN_POINT('',(0.0100673829200725,0.0166225526528062,0.0400686266341829));
#42674=CARTESIAN_POINT('',(0.0100280785092642,0.0165587699208662,0.0400444133545312));
#42675=CARTESIAN_POINT('',(0.00999312597703867,0.0165051542085715,0.039956792543069));
#42676=CARTESIAN_POINT('',(0.00999149890733325,0.0165061368666732,0.0398784290286423));
#42677=CARTESIAN_POINT('',(0.00834737832249906,0.017549210372631,0.0401157595299874));
#42678=CARTESIAN_POINT('',(0.0083146237018335,0.0174816849729387,0.0400916485526069));
#42679=CARTESIAN_POINT('',(0.00828510636698564,0.0174246703944439,0.040003913952241));
#42680=CARTESIAN_POINT('',(0.00828332989840086,0.0174255146209965,0.0399254572243831));
#42681=CARTESIAN_POINT('',(0.00473953259241176,0.0188458640380989,0.040211512069501));
#42682=CARTESIAN_POINT('',(0.0047207264931358,0.0187734587187308,0.0401872142418862));
#42683=CARTESIAN_POINT('',(0.00470307137359621,0.018712114939268,0.0400996918515199));
#42684=CARTESIAN_POINT('',(0.00470116778765926,0.0187125929642203,0.0400214091930436));
#42685=CARTESIAN_POINT('',(0.00281385362484171,0.0192276739823713,0.0402594115432935));
#42686=CARTESIAN_POINT('',(0.00280244216170432,0.0191537339652338,0.0402351197714317));
#42687=CARTESIAN_POINT('',(0.00279109103467653,0.0190909074196349,0.0401475885704477));
#42688=CARTESIAN_POINT('',(0.00278920281488217,0.019091183988523,0.0400692985725725));
#42689=CARTESIAN_POINT('',(-0.00101085160756184,0.0194066985670039,0.0403530112899306));
#42690=CARTESIAN_POINT('',(-0.00100753201763225,0.0193317466932373,0.0403288812557846));
#42691=CARTESIAN_POINT('',(-0.00100634339435394,0.0192675947719003,0.0402411666875001));
#42692=CARTESIAN_POINT('',(-0.0010082631995002,0.0192674950044555,0.0401627263035939));
#42693=CARTESIAN_POINT('',(-0.00296586699536353,0.0192049596230593,0.0404017829715575));
#42694=CARTESIAN_POINT('',(-0.00295502402753038,0.019130895206498,0.0403775214550599));
#42695=CARTESIAN_POINT('',(-0.00294743051497526,0.0190674417552862,0.040289958079941));
#42696=CARTESIAN_POINT('',(-0.00294937536344791,0.0190671384373783,0.0402116418088512));
#42697=CARTESIAN_POINT('',(-0.00667478459254796,0.0182501325704563,0.0404966423224674));
#42698=CARTESIAN_POINT('',(-0.0066496376241613,0.0181797025697532,0.0404723274623812));
#42699=CARTESIAN_POINT('',(-0.00662973097637039,0.018119087966066,0.0403848231561246));
#42700=CARTESIAN_POINT('',(-0.0066315320520576,0.0181184261421127,0.0403065552228863));
#42701=CARTESIAN_POINT('',(-0.00848057591989537,0.0174853536409583,0.0405433851196045));
#42702=CARTESIAN_POINT('',(-0.00844833575227234,0.0174175882114456,0.0405192688181649));
#42703=CARTESIAN_POINT('',(-0.0084222354928671,0.0173589471688255,0.0404315380802686));
#42704=CARTESIAN_POINT('',(-0.00842394764778655,0.0173581211968173,0.0403530843731059));
#42705=CARTESIAN_POINT('',(-0.0117501648030116,0.0154785718893798,0.0406383502013855));
#42706=CARTESIAN_POINT('',(-0.0117052950541378,0.0154184856025082,0.0406141935740401));
#42707=CARTESIAN_POINT('',(-0.0116683116154951,0.0153661186350555,0.0405265117750975));
#42708=CARTESIAN_POINT('',(-0.0116698995197312,0.0153649181792621,0.0404480984064987));
#42709=CARTESIAN_POINT('',(-0.0132419645360361,0.01422343802526,0.0406869447264834));
#42710=CARTESIAN_POINT('',(-0.0131914477879221,0.0141683084749517,0.0406626190329021));
#42711=CARTESIAN_POINT('',(-0.0131495970747723,0.0141201765420058,0.0405751279738163));
#42712=CARTESIAN_POINT('',(-0.0131510178975401,0.0141188503836186,0.0404968709562312));
#42713=CARTESIAN_POINT('',(-0.0157858403880931,0.011334670738937,0.0407814369533176));
#42714=CARTESIAN_POINT('',(-0.0157253427703919,0.0112905215962408,0.0407572027913683));
#42715=CARTESIAN_POINT('',(-0.0156746531259851,0.0112515127002032,0.0406696058633485));
#42716=CARTESIAN_POINT('',(-0.0156757612826429,0.0112499651602134,0.0405912619422651));
#42717=CARTESIAN_POINT('',(-0.0168337225819455,0.0097128872234943,0.0408280824322182));
#42718=CARTESIAN_POINT('',(-0.0167690424369808,0.00967490186409546,0.0408039349928322));
#42719=CARTESIAN_POINT('',(-0.0167146050123985,0.00964099036924619,0.0407162417069933));
#42720=CARTESIAN_POINT('',(-0.0167155867809466,0.00963928678279519,0.0406378188741549));
#42721=CARTESIAN_POINT('',(-0.018423271651614,0.00618680701624641,0.0409245341856734));
#42722=CARTESIAN_POINT('',(-0.0183525530717912,0.006162448432523,0.0409002225940088));
#42723=CARTESIAN_POINT('',(-0.0182927812174779,0.0061401035270347,0.0408127157048635));
#42724=CARTESIAN_POINT('',(-0.0182934027154407,0.0061382496041647,0.0407344457386575));
#42725=CARTESIAN_POINT('',(-0.0189430547325762,0.0043443461353158,0.0409710362127245));
#42726=CARTESIAN_POINT('',(-0.0188702341171792,0.00432704686481311,0.0409467617589281));
#42727=CARTESIAN_POINT('',(-0.0188084758538503,0.00431069829717667,0.0408592105361161));
#42728=CARTESIAN_POINT('',(-0.0188089018133566,0.00430884403332253,0.0407809041095408));
#42729=CARTESIAN_POINT('',(-0.0194289986128713,0.000499713531233832,0.0410656760686004));
#42730=CARTESIAN_POINT('',(-0.0193539583666749,0.000497198497755513,0.0410415831174496));
#42731=CARTESIAN_POINT('',(-0.0192898275617786,0.000493392807686237,0.0409538266520444));
#42732=CARTESIAN_POINT('',(-0.0192898777469486,0.000491468041456822,0.040875351896354));
#42733=CARTESIAN_POINT('',(-0.0193817406628462,-0.00142299211126438,0.0411135075422031));
#42734=CARTESIAN_POINT('',(-0.0193070170772642,-0.00141809444964756,0.0410892654598308));
#42735=CARTESIAN_POINT('',(-0.019243117359171,-0.00141559108917121,0.0410016800819513));
#42736=CARTESIAN_POINT('',(-0.0192429699175204,-0.00141755853501489,0.040923345775823));
#42737=CARTESIAN_POINT('',(-0.0187193942117811,-0.00522021721159691,0.0412091471935832));
#42738=CARTESIAN_POINT('',(-0.0186472127981405,-0.0052006845494549,0.0411848232168061));
#42739=CARTESIAN_POINT('',(-0.0185852342022787,-0.0051856082833503,0.0410973294412903));
#42740=CARTESIAN_POINT('',(-0.0185847148569473,-0.00518745960300022,0.0410190701522683));
#42741=CARTESIAN_POINT('',(-0.0181039359117161,-0.00706460040595502,0.0412555665134694));
#42742=CARTESIAN_POINT('',(-0.0180338532992189,-0.00703785993463442,0.0412314243596961));
#42743=CARTESIAN_POINT('',(-0.0179733690213254,-0.00701652438380678,0.0411437230827132));
#42744=CARTESIAN_POINT('',(-0.0179726792551525,-0.00701830153821873,0.0410652935604343));
#42745=CARTESIAN_POINT('',(-0.0163613828719178,-0.0104861909729681,0.0413506434124658));
#42746=CARTESIAN_POINT('',(-0.0162979641669806,-0.0104462472372041,0.0413264544004279));
#42747=CARTESIAN_POINT('',(-0.0162428869540188,-0.0104135600110401,0.0412388091539726));
#42748=CARTESIAN_POINT('',(-0.0162418185736249,-0.0104152333392688,0.0411604257625291));
#42749=CARTESIAN_POINT('',(-0.0152223786671565,-0.0120789136020188,0.0413992881003474));
#42750=CARTESIAN_POINT('',(-0.0151634461213869,-0.0120329066992753,0.0413749569533594));
#42751=CARTESIAN_POINT('',(-0.0151121781877566,-0.0119949854999305,0.0412874718141746));
#42752=CARTESIAN_POINT('',(-0.0151109728566117,-0.0119965009218216,0.0412092196393451));
#42753=CARTESIAN_POINT('',(-0.0125568686401054,-0.0148311281959786,0.0414931318161541));
#42754=CARTESIAN_POINT('',(-0.012508011411256,-0.0147743157003177,0.0414689287321229));
#42755=CARTESIAN_POINT('',(-0.0124650463432653,-0.0147268539152569,0.0413812963157667));
#42756=CARTESIAN_POINT('',(-0.0124635942482089,-0.0147280804403202,0.0413029232831929));
#42757=CARTESIAN_POINT('',(-0.010995231801385,-0.0160233379181721,0.0415406428119252));
#42758=CARTESIAN_POINT('',(-0.0109523014847925,-0.0159617922274038,0.0415165240644872));
#42759=CARTESIAN_POINT('',(-0.0109142176058814,-0.0159101249346095,0.0414287983483162));
#42760=CARTESIAN_POINT('',(-0.0109125933109026,-0.0159112383674669,0.0413503489155356));
#42761=CARTESIAN_POINT('',(-0.00764011994476365,-0.0178674958607134,0.0416362600396937));
#42762=CARTESIAN_POINT('',(-0.00761018133565773,-0.017798951100108,0.0416119553101224));
#42763=CARTESIAN_POINT('',(-0.00758312062253375,-0.0177411528083686,0.0415244406939323));
#42764=CARTESIAN_POINT('',(-0.00758131839265829,-0.0177419224038618,0.0414461644041004));
#42765=CARTESIAN_POINT('',(-0.00579698462809434,-0.0185478388243877,0.0416841102526258));
#42766=CARTESIAN_POINT('',(-0.00577410687134877,-0.01847659559011,0.0416598265164387));
#42767=CARTESIAN_POINT('',(-0.00575303316508779,-0.0184163131855544,0.04157228606953));
#42768=CARTESIAN_POINT('',(-0.0057512140507308,-0.0184168822966398,0.0414939884842142));
#42769=CARTESIAN_POINT('',(-0.00204511726705045,-0.0193252414217171,0.0417777971524379));
#42770=CARTESIAN_POINT('',(-0.00203664008434553,-0.0192506900880234,0.0417536717205969));
#42771=CARTESIAN_POINT('',(-0.00202774868857115,-0.019187136766194,0.0416659520810417));
#42772=CARTESIAN_POINT('',(-0.00202583336017481,-0.019187339987148,0.0415875075428947));
#42773=CARTESIAN_POINT('',(-9.05804658936935E-5,-0.0194329094892977,0.0418264478471602));
#42774=CARTESIAN_POINT('',(-8.9642911205528E-5,-0.0193580705522084,0.0418021777740408));
#42775=CARTESIAN_POINT('',(-8.71656546924683E-5,-0.019294227531414,0.0417146241096909));
#42776=CARTESIAN_POINT('',(-8.51986897315877E-5,-0.0192942337059858,0.0416363157991664));
#42777=CARTESIAN_POINT('',(0.00373284185397302,-0.0190711043162353,0.0419214916564631));
#42778=CARTESIAN_POINT('',(0.00371903948671961,-0.0189975958351805,0.0418971816093208));
#42779=CARTESIAN_POINT('',(0.00370887284137344,-0.018934599967898,0.0418096717232319));
#42780=CARTESIAN_POINT('',(0.00371075297471115,-0.0189342289380529,0.0417313992090289));
#42781=CARTESIAN_POINT('',(0.0056195348488219,-0.0186041914397168,0.041967771073828));
#42782=CARTESIAN_POINT('',(0.00559837174197131,-0.0185321764440214,0.0419436646493534));
#42783=CARTESIAN_POINT('',(0.0055818376167325,-0.0184701315167897,0.0418559229912704));
#42784=CARTESIAN_POINT('',(0.00558366573546322,-0.0184695830661741,0.041777460339377));
#42785=CARTESIAN_POINT('',(0.00918111747785819,-0.0171287475784746,0.0420633382769924));
#42786=CARTESIAN_POINT('',(0.00914621849626832,-0.0170623881114195,0.0420391678140263));
#42787=CARTESIAN_POINT('',(0.00911790208787631,-0.0170048972731719,0.0419515016544082));
#42788=CARTESIAN_POINT('',(0.00911965739953659,-0.0170039604386378,0.0418731011158541));
#42789=CARTESIAN_POINT('',(0.0108287157855478,-0.0161383651826623,0.0421111871737686));
#42790=CARTESIAN_POINT('',(0.0107875443681479,-0.0160759437721169,0.0420868590299796));
#42791=CARTESIAN_POINT('',(0.0107538243240508,-0.0160218044754006,0.0419993706635951));
#42792=CARTESIAN_POINT('',(0.0107554348807014,-0.0160207209592401,0.041921115849482));
#42793=CARTESIAN_POINT('',(0.0138163523926375,-0.0136685566777615,0.0422062857606146));
#42794=CARTESIAN_POINT('',(0.0137635062306705,-0.0136154636695298,0.0421820602826808));
#42795=CARTESIAN_POINT('',(0.0137195386676774,-0.0135689798753639,0.0420944534535886));
#42796=CARTESIAN_POINT('',(0.0137208756379874,-0.0135676251147251,0.0420161014120124));
#42797=CARTESIAN_POINT('',(0.0150937991990989,-0.0122429033161526,0.0422526218686467));
#42798=CARTESIAN_POINT('',(0.0150359189264516,-0.0121952115724331,0.0422284654018838));
#42799=CARTESIAN_POINT('',(0.0149875171517796,-0.0121531589775004,0.0421407824163082));
#42800=CARTESIAN_POINT('',(0.0149887556291129,-0.012151630069666,0.0420623680363629));
#42801=CARTESIAN_POINT('',(0.0172184502353371,-0.009012020296029,0.0423490045947479));
#42802=CARTESIAN_POINT('',(0.0171524539800783,-0.00897682604798362,0.042324691488919));
#42803=CARTESIAN_POINT('',(0.0170969498824196,-0.00894534784936932,0.0422371862082005));
#42804=CARTESIAN_POINT('',(0.0170978537102632,-0.0089436182365821,0.0421589175519357));
#42805=CARTESIAN_POINT('',(0.0180274816378425,-0.00725761467570689,0.0423958372533736));
#42806=CARTESIAN_POINT('',(0.0179582537787476,-0.00722911756875251,0.0423715794694566));
#42807=CARTESIAN_POINT('',(0.0178997912496169,-0.00720328948227317,0.0422840092016225));
#42808=CARTESIAN_POINT('',(0.0179005019669257,-0.00720152699125071,0.0422056871496299));
#42809=CARTESIAN_POINT('',(0.0191046950454922,-0.00356301633164709,0.0424898936854717));
#42810=CARTESIAN_POINT('',(0.0190309951402892,-0.00354867574103588,0.0424658045978915));
#42811=CARTESIAN_POINT('',(0.0189682692840251,-0.00353477957180662,0.0423780440089436));
#42812=CARTESIAN_POINT('',(0.0189686243930409,-0.0035328813041711,0.0422995658792278));
#42813=CARTESIAN_POINT('',(0.0193644544292967,-0.00163030860279191,0.0425384839417672));
#42814=CARTESIAN_POINT('',(0.0192899038645396,-0.00162344189871589,0.0425142307870624));
#42815=CARTESIAN_POINT('',(0.0192264252594773,-0.00161590860419999,0.0424266579222541));
#42816=CARTESIAN_POINT('',(0.0192265874470749,-0.0016139458694519,0.0423483338702482));
#42817=CARTESIAN_POINT('',(0.0193072408081446,0.00220542823088705,0.0426334895036402));
#42818=CARTESIAN_POINT('',(0.01923286195712,0.00219751006854614,0.0426091846427798));
#42819=CARTESIAN_POINT('',(0.019169247600259,0.0021923811499423,0.0425216688740683));
#42820=CARTESIAN_POINT('',(0.0191690269526096,0.00219428617542683,0.0424433915393039));
#42821=CARTESIAN_POINT('',(0.0189869068886521,0.00414048987402366,0.0426802037297687));
#42822=CARTESIAN_POINT('',(0.01891345262312,0.00412504746132331,0.0426561010076335));
#42823=CARTESIAN_POINT('',(0.0188502989803406,0.00411343336493398,0.0425683550470634));
#42824=CARTESIAN_POINT('',(0.0188498968568833,0.00411529619648721,0.0424898888595828));
#42825=CARTESIAN_POINT('',(0.0178060736540218,0.0077833268932127,0.0427752115903381));
#42826=CARTESIAN_POINT('',(0.0177371541792912,0.00775384712325843,0.0427510318674556));
#42827=CARTESIAN_POINT('',(0.017677604400204,0.00773022695108189,0.0426633764366052));
#42828=CARTESIAN_POINT('',(0.0176768086339158,0.00773205734716713,0.0425849847137418));
#42829=CARTESIAN_POINT('',(0.0169282222197374,0.00954199709281463,0.0428242133111679));
#42830=CARTESIAN_POINT('',(0.0168628218514916,0.00950581417344825,0.0427998657441485));
#42831=CARTESIAN_POINT('',(0.0168062687037002,0.00947642024545496,0.0427123993667165));
#42832=CARTESIAN_POINT('',(0.0168053156255896,0.0094781059476651,0.0426341625770041));
#42833=CARTESIAN_POINT('',(0.0152787301216398,0.0118928357701172,0.0428944730874302));
#42834=CARTESIAN_POINT('',(0.0152195044455773,0.0118474598128942,0.0428702336640911));
#42835=CARTESIAN_POINT('',(0.0151679575922512,0.0118100113144053,0.0427826428309556));
#42836=CARTESIAN_POINT('',(0.0151667907386638,0.0118115087985106,0.0427043039122707));
#42837=CARTESIAN_POINT('',(0.0146717483068224,0.0126350518476812,0.0429176501654895));
#42838=CARTESIAN_POINT('',(0.0146147700280014,0.0125867335795153,0.0428934842250373));
#42839=CARTESIAN_POINT('',(0.0145650311406933,0.0125466826050009,0.0428058098733814));
#42840=CARTESIAN_POINT('',(0.0145637933589508,0.0125481208887642,0.0427274024400431));
#42841=CARTESIAN_POINT('',(0.0133400624183863,0.0140340131728593,0.0429650606966497));
#42842=CARTESIAN_POINT('',(0.0132881303661509,0.0139802216821325,0.0429409428302006));
#42843=CARTESIAN_POINT('',(0.0132425288710425,0.0139353796424642,0.0428532155792548));
#42844=CARTESIAN_POINT('',(0.013241122291298,0.0139367175227223,0.0427747648303184));
#42845=CARTESIAN_POINT('',(0.0126150983580388,0.0146866171639263,0.042989652595112));
#42846=CARTESIAN_POINT('',(0.0125664024074084,0.0146304267516039,0.0429647923161076));
#42847=CARTESIAN_POINT('',(0.0125248389268988,0.0145834093453335,0.0428775280838563));
#42848=CARTESIAN_POINT('',(0.0125244674148037,0.0145837132205409,0.042799403358162));
#42849=CARTESIAN_POINT('',(0.0118641087128433,0.0152851839160009,0.0429958229345714));
#42850=CARTESIAN_POINT('',(0.0118157461105819,0.0152229742289092,0.0429751567186458));
#42851=CARTESIAN_POINT('',(0.0117723227925367,0.0151674788982722,0.0428837874796227));
#42852=CARTESIAN_POINT('',(0.0117721272428104,0.015167630671238,0.04280232572374));
#42853=CARTESIAN_POINT('',(0.0136941102546716,0.013457761490415,0.0337585246215808));
#42854=CARTESIAN_POINT('',(0.0135895474492647,0.013564160655447,0.0337622503149065));
#42855=CARTESIAN_POINT('',(0.01334654683062,0.0138064699816532,0.0337708464888983));
#42856=CARTESIAN_POINT('',(0.0128765937054183,0.0142481009367531,0.0337870668407993));
#42857=CARTESIAN_POINT('',(0.0123812852719009,0.0146790102787035,0.0338036262209131));
#42858=CARTESIAN_POINT('',(0.011936906974365,0.0150409981913683,0.0338181036860316));
#42859=CARTESIAN_POINT('',(0.0115301573081769,0.0153545232374545,0.0338310925608864));
#42860=CARTESIAN_POINT('',(0.0112446290788422,0.015564003170425,0.0338400407264213));
#42861=CARTESIAN_POINT('',(0.0108253784832943,0.0158609026048407,0.0338529843428364));
#42862=CARTESIAN_POINT('',(0.010324636018273,0.0161929424871847,0.0338680560525854));
#42863=CARTESIAN_POINT('',(0.00972406948175458,0.0165597766514572,0.0338856035628603));
#42864=CARTESIAN_POINT('',(0.0091724403886533,0.0168718086851734,0.0339012951499738));
#42865=CARTESIAN_POINT('',(0.00852858148303964,0.0172069826354789,0.0339191663943377));
#42866=CARTESIAN_POINT('',(0.00789371996930137,0.0175068391635713,0.0339363895649794));
#42867=CARTESIAN_POINT('',(0.007353800789958,0.017738735947024,0.0339507482859093));
#42868=CARTESIAN_POINT('',(0.00696670183591407,0.0178920847815684,0.0339608928198493));
#42869=CARTESIAN_POINT('',(0.00675326239252082,0.0179734876172019,0.033966451706429));
#42870=CARTESIAN_POINT('',(0.00656721188965184,0.0180421563621817,0.0339712701462319));
#42871=CARTESIAN_POINT('',(0.00647774007262375,0.018074345239179,0.0339735851140953));
#42872=CARTESIAN_POINT('',(0.00631178123728991,0.0181332991798986,0.0339778913305606));
#42873=CARTESIAN_POINT('',(0.00601080715784662,0.0182365193187258,0.0339857151080177));
#42874=CARTESIAN_POINT('',(0.00549520048212785,0.0184015890871872,0.0339991324785569));
#42875=CARTESIAN_POINT('',(0.00486734732829062,0.01857623817052,0.0340154149159029));
#42876=CARTESIAN_POINT('',(0.00431522273416663,0.018710900877931,0.0340296727710237));
#42877=CARTESIAN_POINT('',(0.00382175659852987,0.0188175153011505,0.0340423767830938));
#42878=CARTESIAN_POINT('',(0.00347079643802958,0.0188847748277211,0.034051372586562));
#42879=CARTESIAN_POINT('',(0.00295799950639641,0.018973974806623,0.0340644528912556));
#42880=CARTESIAN_POINT('',(0.00209444891561219,0.0190965256364289,0.0340863242877525));
#42881=CARTESIAN_POINT('',(0.00088264967494292,0.0191971690537947,0.0341166697948567));
#42882=CARTESIAN_POINT('',(-0.000265183527458678,0.0192075069895004,0.0341451369917628));
#42883=CARTESIAN_POINT('',(-0.00104676910514645,0.019173434339615,0.0341644461903466));
#42884=CARTESIAN_POINT('',(-0.00146947003827434,0.0191447694438164,0.0341748775932301));
#42885=CARTESIAN_POINT('',(-0.00182217380906955,0.0191140171311492,0.0341835724100592));
#42886=CARTESIAN_POINT('',(-0.00201525877505204,0.0190942941612785,0.0341883416702004));
#42887=CARTESIAN_POINT('',(-0.00235530901830927,0.0190564618912583,0.0341967754294064));
#42888=CARTESIAN_POINT('',(-0.00297748392721909,0.0189740593513065,0.0342122985383287));
#42889=CARTESIAN_POINT('',(-0.00403678940420134,0.0187887784475889,0.034239022591207));
#42890=CARTESIAN_POINT('',(-0.0052889441035157,0.0184721107348805,0.0342712683636976));
#42891=CARTESIAN_POINT('',(-0.00625355214601337,0.0181576172995491,0.0342966798883434));
#42892=CARTESIAN_POINT('',(-0.00676271658551289,0.0179706639211776,0.0343102840321073));
#42893=CARTESIAN_POINT('',(-0.00704946142295342,0.0178596671197241,0.0343179998365711));
#42894=CARTESIAN_POINT('',(-0.00729501792534726,0.0177605771205138,0.0343246478509529));
#42895=CARTESIAN_POINT('',(-0.00743702325795866,0.0177013632470171,0.0343285094384181));
#42896=CARTESIAN_POINT('',(-0.00766141934138433,0.0176059659993698,0.0343346234804498));
#42897=CARTESIAN_POINT('',(-0.00803514983488992,0.0174404794253086,0.0343448579947234));
#42898=CARTESIAN_POINT('',(-0.0087850330542926,0.0170838852172053,0.0343655931162305));
#42899=CARTESIAN_POINT('',(-0.00961358323222665,0.0166315511648749,0.0343890271514878));
#42900=CARTESIAN_POINT('',(-0.010417114523336,0.0161335564903514,0.0344123822255873));
#42901=CARTESIAN_POINT('',(-0.0109074208000341,0.015803970647621,0.0344269254265874));
#42902=CARTESIAN_POINT('',(-0.0112919160733621,0.0155298062326985,0.0344385204583214));
#42903=CARTESIAN_POINT('',(-0.0115772453337043,0.0153182329300907,0.0344472264029292));
#42904=CARTESIAN_POINT('',(-0.0118091588638532,0.0151396810220304,0.0344543871753119));
#42905=CARTESIAN_POINT('',(-0.0119747865130799,0.0150083073640502,0.0344595520977263));
#42906=CARTESIAN_POINT('',(-0.0120610264990449,0.0149390577059178,0.0344622528669767));
#42907=CARTESIAN_POINT('',(-0.0121476861584109,0.0148686064259165,0.0344649779294458));
#42908=CARTESIAN_POINT('',(-0.0121490871942248,0.0148673937526884,0.0344650244436881));
#42909=CARTESIAN_POINT('',(-0.012185961924089,0.0148372383407356,0.0344661941039101));
#42910=CARTESIAN_POINT('',(-0.0122470677776355,0.0147869320183904,0.0344681504822471));
#42911=CARTESIAN_POINT('',(-0.0124227600987986,0.0146407236228182,0.0344738288083486));
#42912=CARTESIAN_POINT('',(-0.012715495880542,0.0143895546814955,0.0344834696544062));
#42913=CARTESIAN_POINT('',(-0.0130990369149521,0.014039692277915,0.0344964829696457));
#42914=CARTESIAN_POINT('',(-0.0134260848981876,0.013728183831799,0.0345078184723691));
#42915=CARTESIAN_POINT('',(-0.0137360546234464,0.0134168816015701,0.0345188546161402));
#42916=CARTESIAN_POINT('',(-0.0139882906799606,0.0131530959686775,0.0345280281181907));
#42917=CARTESIAN_POINT('',(-0.0142201817272134,0.0129015418221073,0.034536631612315));
#42918=CARTESIAN_POINT('',(-0.0143266064427612,0.0127826328112155,0.0345406433614217));
#42919=CARTESIAN_POINT('',(-0.0145066481029053,0.0125790201543027,0.0345474706117571));
#42920=CARTESIAN_POINT('',(-0.0147902746456681,0.0122471231614338,0.0345584219683724));
#42921=CARTESIAN_POINT('',(-0.015174778428772,0.0117700082232991,0.034573750880059));
#42922=CARTESIAN_POINT('',(-0.0155127292111199,0.0113174191605092,0.0345878245341603));
#42923=CARTESIAN_POINT('',(-0.0157362681348944,0.0110011849494621,0.0345974416553844));
#42924=CARTESIAN_POINT('',(-0.0158496869700815,0.0108369266575419,0.0346023906521781));
#42925=CARTESIAN_POINT('',(-0.0159571868772797,0.0106777061651138,0.0346071463999587));
#42926=CARTESIAN_POINT('',(-0.0159663462936758,0.0106637422864074,0.0346075577231221));
#42927=CARTESIAN_POINT('',(-0.0160276561327147,0.0105717118602376,0.0346102871836528));
#42928=CARTESIAN_POINT('',(-0.0161476069176707,0.0103888001327877,0.0346156758069228));
#42929=CARTESIAN_POINT('',(-0.0163581974103101,0.0100574369270042,0.0346253353556078));
#42930=CARTESIAN_POINT('',(-0.0166217923490061,0.00961328317443536,0.0346380332767143));
#42931=CARTESIAN_POINT('',(-0.0168446227175717,0.00921819835684225,0.0346491817224154));
#42932=CARTESIAN_POINT('',(-0.0170456288458299,0.00884020300519206,0.0346597012247684));
#42933=CARTESIAN_POINT('',(-0.0171960295178942,0.00854112137700337,0.0346679264580525));
#42934=CARTESIAN_POINT('',(-0.0172790049411183,0.00837171883319988,0.0346725610105133));
#42935=CARTESIAN_POINT('',(-0.0173547950476286,0.00821319909425432,0.0346768775789744));
#42936=CARTESIAN_POINT('',(-0.0173820928307441,0.00815499207037812,0.0346784576900277));
#42937=CARTESIAN_POINT('',(-0.0174348258340047,0.00804203806109061,0.0346815237131564));
#42938=CARTESIAN_POINT('',(-0.0175180723128191,0.00785997902884154,0.0346864537280027));
#42939=CARTESIAN_POINT('',(-0.0176376136993543,0.00758925941223894,0.0346937581407388));
#42940=CARTESIAN_POINT('',(-0.0177736098997301,0.00726500599075267,0.0347024643405804));
#42941=CARTESIAN_POINT('',(-0.0179481211417278,0.00682648423236474,0.0347141867892852));
#42942=CARTESIAN_POINT('',(-0.0181095832063446,0.00638655283579656,0.0347258777552459));
#42943=CARTESIAN_POINT('',(-0.0182627011614772,0.00592868581523455,0.0347379790976535));
#42944=CARTESIAN_POINT('',(-0.0183620783579825,0.00561489817091336,0.0347462570227646));
#42945=CARTESIAN_POINT('',(-0.0184911675089137,0.00517537833237663,0.0347577897996903));
#42946=CARTESIAN_POINT('',(-0.018633074967421,0.00464483147881868,0.034771595644462));
#42947=CARTESIAN_POINT('',(-0.0188493565307284,0.00372059112093591,0.0347954200936349));
#42948=CARTESIAN_POINT('',(-0.0190550954247574,0.00249158709200293,0.0348265651563859));
#42949=CARTESIAN_POINT('',(-0.0191790575163336,0.00115543871336813,0.0348599221754414));
#42950=CARTESIAN_POINT('',(-0.0192,0.000367624981005561,0.0348793718366157));
#42951=CARTESIAN_POINT('',(-0.0192,0.,0.0348884087721565));
#42952=CARTESIAN_POINT('',(0.0136941126101477,0.0134577620508462,0.0337585747238691));
#42953=CARTESIAN_POINT('',(-0.0192,1.85786059226098E-19,0.0348884087721565));
#42954=CARTESIAN_POINT('',(0.0136941154444571,0.0134577621240347,0.0337586248089782));
#42955=CARTESIAN_POINT('',(0.0136826371269313,0.0134694418914976,0.0337617141202682));
#42956=CARTESIAN_POINT('',(0.0136430578016153,0.013509394949222,0.0337721504615356));
#42957=CARTESIAN_POINT('',(0.0134399334786531,0.0137221538478718,0.0338277048930865));
#42958=CARTESIAN_POINT('',(0.0133538196812112,0.0138190636682607,0.0338522664919164));
#42959=CARTESIAN_POINT('',(0.0133075373500049,0.0138718845916857,0.0338655904181358));
#42960=CARTESIAN_POINT('',(0.0129669874288091,0.0143467767916369,0.0339772843973612));
#42961=CARTESIAN_POINT('',(0.0115713800653362,0.0156079658614213,0.0340242546179052));
#42962=CARTESIAN_POINT('',(0.00917172797759027,0.0172065231735504,0.0340957211296002));
#42963=CARTESIAN_POINT('',(0.00565700559390481,0.0185655378803378,0.0341863739834551));
#42964=CARTESIAN_POINT('',(0.00286356960593685,0.0191945939613825,0.0342580305967084));
#42965=CARTESIAN_POINT('',(6.00390298951636E-5,0.0194071967834707,0.0343276084462218));
#42966=CARTESIAN_POINT('',(-0.00280547377715355,0.0192040953034031,0.0343972796574007));
#42967=CARTESIAN_POINT('',(-0.00555104901130441,0.0185964846565865,0.0344666190124259));
#42968=CARTESIAN_POINT('',(-0.00911660442038569,0.0172386681088485,0.0345620081421828));
#42969=CARTESIAN_POINT('',(-0.0122793980430035,0.0151500481911074,0.0346526132888181));
#42970=CARTESIAN_POINT('',(-0.0149232917304808,0.0124063671395135,0.0347478780396232));
#42971=CARTESIAN_POINT('',(-0.0165616126372687,0.0101175449752386,0.0348171161399589));
#42972=CARTESIAN_POINT('',(-0.0178737227091099,0.00756282226843125,0.0348866382876858));
#42973=CARTESIAN_POINT('',(-0.0187779015622702,0.00490239274816994,0.0349565395549962));
#42974=CARTESIAN_POINT('',(-0.0192952846344691,0.00208222391132934,0.035027924969667));
#42975=CARTESIAN_POINT('',(-0.0194268294272506,-0.00167922858791242,0.0351192514716495));
#42976=CARTESIAN_POINT('',(-0.0187196013062885,-0.00545527351177937,0.0352143794552229));
#42977=CARTESIAN_POINT('',(-0.0172399183781032,-0.00891304084397672,0.0353065595114178));
#42978=CARTESIAN_POINT('',(-0.0157375834854316,-0.0113573828877688,0.0353761580765403));
#42979=CARTESIAN_POINT('',(-0.0139325142252646,-0.0135103121249464,0.0354464263275229));
#42980=CARTESIAN_POINT('',(-0.0117870130508438,-0.0154180328418685,0.0355175145555988));
#42981=CARTESIAN_POINT('',(-0.00943081487800948,-0.0169618553426991,0.0355857575287973));
#42982=CARTESIAN_POINT('',(-0.0059780389972534,-0.0185615634550717,0.0356801290647163));
#42983=CARTESIAN_POINT('',(-0.00227155551396098,-0.0193687118024069,0.0357728320835663));
#42984=CARTESIAN_POINT('',(0.00154447697031841,-0.0193459848972831,0.0358658407634035));
#42985=CARTESIAN_POINT('',(0.0043234624990737,-0.0189197123559901,0.0359362675419697));
#42986=CARTESIAN_POINT('',(0.0070686233449079,-0.0180743485664414,0.0360069893486505));
#42987=CARTESIAN_POINT('',(0.00960729763734257,-0.0168625579867165,0.0360751939385716));
#42988=CARTESIAN_POINT('',(0.0119817385251178,-0.0152679901260296,0.036146398333989));
#42989=CARTESIAN_POINT('',(0.0140751032296404,-0.0133602052681052,0.0362165935557949));
#42990=CARTESIAN_POINT('',(0.0158720725358971,-0.0111697360825902,0.0362853008234503));
#42991=CARTESIAN_POINT('',(0.017339924630644,-0.00871616399730907,0.0363556492418429));
#42992=CARTESIAN_POINT('',(0.01841839670659,-0.00611632933404608,0.0364260662584277));
#42993=CARTESIAN_POINT('',(0.0191193204551073,-0.00333208225338983,0.0364963626431574));
#42994=CARTESIAN_POINT('',(0.0194001577826843,-0.000534679403752089,0.0365647528474457));
#42995=CARTESIAN_POINT('',(0.0192236717854676,0.00327853672896307,0.0366602725835808));
#42996=CARTESIAN_POINT('',(0.018224829179944,0.00693697048911509,0.0367513080216613));
#42997=CARTESIAN_POINT('',(0.0164475669963537,0.0103015758611845,0.0368454846683361));
#42998=CARTESIAN_POINT('',(0.0147828163275645,0.0125743553559636,0.0369157664930877));
#42999=CARTESIAN_POINT('',(0.0127662795816731,0.0146175804468894,0.036985696406264));
#43000=CARTESIAN_POINT('',(0.010521926670691,0.0163078537119878,0.0370544310064815));
#43001=CARTESIAN_POINT('',(0.00800300191271364,0.0176804927319421,0.0371262210936272));
#43002=CARTESIAN_POINT('',(0.00447259200101117,0.0189788791549912,0.0372181259863815));
#43003=CARTESIAN_POINT('',(0.000664909643921832,0.0194877876118655,0.0373117878618414));
#43004=CARTESIAN_POINT('',(-0.00308456505535271,0.0191606283485715,0.0374054362510788));
#43005=CARTESIAN_POINT('',(-0.00587409426056678,0.0184972029882785,0.0374750047751963));
#43006=CARTESIAN_POINT('',(-0.00848360455853172,0.0174551515786284,0.0375442942774273));
#43007=CARTESIAN_POINT('',(-0.0109666974490278,0.0160118766280472,0.0376159401009681));
#43008=CARTESIAN_POINT('',(-0.0131672264635854,0.0142568604798726,0.0376845401175858));
#43009=CARTESIAN_POINT('',(-0.0157688169313013,0.0114739692250601,0.0377774471690446));
#43010=CARTESIAN_POINT('',(-0.0176905845230479,0.00820506762897047,0.0378720135163756));
#43011=CARTESIAN_POINT('',(-0.0188604585521843,0.00457496739751311,0.0379643254507625));
#43012=CARTESIAN_POINT('',(-0.0193238678886162,0.00180099601517996,0.038034217719475));
#43013=CARTESIAN_POINT('',(-0.0193776974386726,-0.00107110904910607,0.0381055592469513));
#43014=CARTESIAN_POINT('',(-0.0190194600004675,-0.0038596155043962,0.0381738069591164));
#43015=CARTESIAN_POINT('',(-0.0182460090102748,-0.00661678492586967,0.0382440393960188));
#43016=CARTESIAN_POINT('',(-0.017087926902402,-0.00919618802446331,0.0383148490752953));
#43017=CARTESIAN_POINT('',(-0.0155783506063201,-0.0115757708632551,0.0383839682823852));
#43018=CARTESIAN_POINT('',(-0.0130632358203733,-0.0144816519499531,0.0384773950900149));
#43019=CARTESIAN_POINT('',(-0.010025782979492,-0.0167255305076173,0.0385715559135774));
#43020=CARTESIAN_POINT('',(-0.00653620922525659,-0.0182738357125707,0.038663894601552));
#43021=CARTESIAN_POINT('',(-0.00382731274404074,-0.0190266288203552,0.0387334537957832));
#43022=CARTESIAN_POINT('',(-0.000976733981174734,-0.0193826570182263,0.0388051700031889));
#43023=CARTESIAN_POINT('',(0.00183431259761074,-0.0193202229377954,0.0388737808129606));
#43024=CARTESIAN_POINT('',(0.00465688500635297,-0.0188410216106093,0.0389436412511739));
#43025=CARTESIAN_POINT('',(0.00824013858898105,-0.0176721532478986,0.0390380543124924));
#43026=CARTESIAN_POINT('',(0.0115444908180822,-0.0157139654073397,0.0391299297625707));
#43027=CARTESIAN_POINT('',(0.014282567866367,-0.0131403805311297,0.0392233974621493));
#43028=CARTESIAN_POINT('',(0.0160642150400973,-0.0108892151776004,0.0392947924092649));
#43029=CARTESIAN_POINT('',(0.0174689157689923,-0.00845486378107598,0.0393630514512943));
#43030=CARTESIAN_POINT('',(0.0185240980053153,-0.00579015455245212,0.0394335621023632));
#43031=CARTESIAN_POINT('',(0.0191668143900673,-0.00304030331008378,0.039504060297298));
#43032=CARTESIAN_POINT('',(0.0194070059599408,-0.00020585768527927,0.0395735746428004));
#43033=CARTESIAN_POINT('',(0.0192272197225004,0.00263703515499631,0.0396428116900019));
#43034=CARTESIAN_POINT('',(0.018642647445271,0.00539604189027514,0.0397133466396609));
#43035=CARTESIAN_POINT('',(0.0176426254569399,0.00808509465012985,0.0397842936399775));
#43036=CARTESIAN_POINT('',(0.016290883612116,0.0105484058535663,0.0398523810041133));
#43037=CARTESIAN_POINT('',(0.0145569267682256,0.0128356891429286,0.0399235328516493));
#43038=CARTESIAN_POINT('',(0.0118723213903701,0.0154668195912942,0.0400169915385569));
#43039=CARTESIAN_POINT('',(0.00861024551575036,0.0174959563819991,0.040108902747744));
#43040=CARTESIAN_POINT('',(0.00505465403671454,0.0187375722405681,0.0402032500102804));
#43041=CARTESIAN_POINT('',(0.0022406078308495,0.0192773142856526,0.0402736766567547));
#43042=CARTESIAN_POINT('',(-0.000567815702499361,0.0193996097737672,0.0403419104891806));
#43043=CARTESIAN_POINT('',(-0.00342343385126204,0.019103229646225,0.040413410340871));
#43044=CARTESIAN_POINT('',(-0.00615038409441286,0.0184065111805356,0.0404831263946253));
#43045=CARTESIAN_POINT('',(-0.0096686184475022,0.0169361375016966,0.0405754200348359));
#43046=CARTESIAN_POINT('',(-0.0127612579722979,0.014745466048664,0.0406696667323146));
#43047=CARTESIAN_POINT('',(-0.0153174985528208,0.0119167439622277,0.0407630226618228));
#43048=CARTESIAN_POINT('',(-0.0168803478268236,0.00957730141101147,0.0408314952578956));
#43049=CARTESIAN_POINT('',(-0.0181084201448125,0.00698073191123133,0.040903316503968));
#43050=CARTESIAN_POINT('',(-0.0189264976843559,0.00429183545878377,0.040972517770357));
#43051=CARTESIAN_POINT('',(-0.0193532395078142,0.00145820300039777,0.0410418486064576));
#43052=CARTESIAN_POINT('',(-0.0193620320611151,-0.00230749915773812,0.0411356242159793));
#43053=CARTESIAN_POINT('',(-0.0185332483892014,-0.00605879754200571,0.0412293706720468));
#43054=CARTESIAN_POINT('',(-0.016943283271981,-0.00946543418309202,0.0413213013145344));
#43055=CARTESIAN_POINT('',(-0.015361383898717,-0.011860165190698,0.0413930810113919));
#43056=CARTESIAN_POINT('',(-0.0134878684246655,-0.0139539968664765,0.041461859993234));
#43057=CARTESIAN_POINT('',(-0.011283505722983,-0.0157915277757609,0.041531474060057));
#43058=CARTESIAN_POINT('',(-0.00887573630878226,-0.0172579423885106,0.0416019244936904));
#43059=CARTESIAN_POINT('',(-0.00625374805766054,-0.0183727273844134,0.0416725169175158));
#43060=CARTESIAN_POINT('',(-0.0035009432514515,-0.0190884916581397,0.0417415286098294));
#43061=CARTESIAN_POINT('',(-0.000694024097694391,-0.0193957179364182,0.041811277677145));
#43062=CARTESIAN_POINT('',(0.00217039459611988,-0.0192850364083003,0.0418827211420678));
#43063=CARTESIAN_POINT('',(0.00493306079849546,-0.0187701014847105,0.0419511700517889));
#43064=CARTESIAN_POINT('',(0.00764936514413544,-0.017837231574939,0.0420211945202578));
#43065=CARTESIAN_POINT('',(0.0101479004136944,-0.016541940153591,0.0420917118837952));
#43066=CARTESIAN_POINT('',(0.0124680747395051,-0.0148733882123723,0.0421621302592813));
#43067=CARTESIAN_POINT('',(0.0145011247329489,-0.012897360404977,0.0422308513194342));
#43068=CARTESIAN_POINT('',(0.0162238523411861,-0.0106518911739671,0.0423012625647974));
#43069=CARTESIAN_POINT('',(0.0176125742791933,-0.00814946075124356,0.0423722297397302));
#43070=CARTESIAN_POINT('',(0.0186067193865136,-0.00551875898010681,0.042440438355834));
#43071=CARTESIAN_POINT('',(0.0192174809116328,-0.00271201785770265,0.0425110817790405));
#43072=CARTESIAN_POINT('',(0.0194065096006142,9.34149747220036E-5,0.0425814604532221));
#43073=CARTESIAN_POINT('',(0.0191081892507249,0.00389774562463771,0.0426745473591831));
#43074=CARTESIAN_POINT('',(0.0179919903563871,0.007520895965826,0.042767400870812));
#43075=CARTESIAN_POINT('',(0.0161048328482777,0.0108289039411657,0.0428618782301824));
#43076=CARTESIAN_POINT('',(0.0149474287891037,0.0123060965833487,0.0429072185458034));
#43077=CARTESIAN_POINT('',(0.0143115152723113,0.0130059180970762,0.0429303525689935));
#43078=CARTESIAN_POINT('',(0.0138344501175927,0.013346906106166,0.0428477190027887));
#43079=CARTESIAN_POINT('',(0.0137810933123524,0.0133933759157219,0.0428378817273722));
#43080=CARTESIAN_POINT('',(0.0136815110794371,0.0134813833724383,0.0428194391764527));
#43081=CARTESIAN_POINT('',(0.0134677269994354,0.0136841748462814,0.0427787288709304));
#43082=CARTESIAN_POINT('',(0.0134262957679323,0.0137249207015359,0.0427708801730808));
#43083=CARTESIAN_POINT('',(0.0134137957134195,0.0137371265036079,0.0427684701217644));
#43084=CARTESIAN_POINT('',(0.0134138302057369,0.01373715900257,0.0427684304783987));
#43085=CARTESIAN_POINT('',(0.0192,6.20369116582113E-17,0.0423886526967672));
#43086=CARTESIAN_POINT('',(0.0192,8.41105296097433E-5,0.0423907560454785));
#43087=CARTESIAN_POINT('',(0.0191993101561165,0.000354898460622047,0.0423974844836466));
#43088=CARTESIAN_POINT('',(0.0191766387333424,0.00106850340612669,0.042415143749824));
#43089=CARTESIAN_POINT('',(0.0191112650346421,0.00191748446063122,0.0424361618456873));
#43090=CARTESIAN_POINT('',(0.019019580056546,0.00264245869365634,0.0424541897576075));
#43091=CARTESIAN_POINT('',(0.0189503569894495,0.00309282029534998,0.0424654289275442));
#43092=CARTESIAN_POINT('',(0.0188887797036297,0.00344944824861375,0.0424743542717575));
#43093=CARTESIAN_POINT('',(0.0188293966922826,0.00375842442754358,0.0424821124849691));
#43094=CARTESIAN_POINT('',(0.0187745744306113,0.00402076367859953,0.0424887206147141));
#43095=CARTESIAN_POINT('',(0.0187412404233969,0.00417342550003737,0.0424925731883303));
#43096=CARTESIAN_POINT('',(0.0187050520437726,0.00433168203525138,0.0424965755168272));
#43097=CARTESIAN_POINT('',(0.018696728057649,0.0043671315616813,0.0424974734143471));
#43098=CARTESIAN_POINT('',(0.0186766311706155,0.00445296219600791,0.0424996493623985));
#43099=CARTESIAN_POINT('',(0.0186366467243465,0.00461866745151867,0.0425038653622425));
#43100=CARTESIAN_POINT('',(0.0185680752589999,0.00488971898546871,0.0425108015077658));
#43101=CARTESIAN_POINT('',(0.0184688432623808,0.00525306123742752,0.0425201772806294));
#43102=CARTESIAN_POINT('',(0.0183491800792793,0.00565803440009305,0.042530716283468));
#43103=CARTESIAN_POINT('',(0.0181591486606039,0.00625031568604568,0.0425462733093148));
#43104=CARTESIAN_POINT('',(0.0179166470931237,0.00692068257031733,0.0425641419122045));
#43105=CARTESIAN_POINT('',(0.0176486931774257,0.00756587072340413,0.0425816911154129));
#43106=CARTESIAN_POINT('',(0.0174753152043798,0.00795521723283759,0.0425924075624996));
#43107=CARTESIAN_POINT('',(0.0173638688662241,0.00819524077046688,0.0425990644098585));
#43108=CARTESIAN_POINT('',(0.0172585053153977,0.00841378634159452,0.0426051703025579));
#43109=CARTESIAN_POINT('',(0.0171905663695672,0.00855179612008063,0.0426090415422495));
#43110=CARTESIAN_POINT('',(0.0170630931485617,0.0088055843917611,0.0426161809727479));
#43111=CARTESIAN_POINT('',(0.0168032065498494,0.00929884274092558,0.0426301691842053));
#43112=CARTESIAN_POINT('',(0.0164032373516879,0.00999415034658874,0.0426502129902482));
#43113=CARTESIAN_POINT('',(0.0157098656135333,0.0110705284649427,0.0426820419855479));
#43114=CARTESIAN_POINT('',(0.0147433274768177,0.0123493775949883,0.0427215469906524));
#43115=CARTESIAN_POINT('',(0.0138719316916315,0.0132898260649551,0.0427528145663577));
#43116=CARTESIAN_POINT('',(0.013413822225715,0.013737153027353,0.04276836728379));
#43117=CARTESIAN_POINT('',(0.0192,2.94926899266343E-17,0.0423886526967672));
#43118=CARTESIAN_POINT('',(-0.0192,8.05624845824862E-17,0.0408877752241749));
#43119=CARTESIAN_POINT('',(-0.0192,-0.000790229530708466,0.0409075953257136));
#43120=CARTESIAN_POINT('',(-0.0191024902357828,-0.00228924689105798,0.0409451529412056));
#43121=CARTESIAN_POINT('',(-0.0187518434727255,-0.00426572061081252,0.0409951852764988));
#43122=CARTESIAN_POINT('',(-0.0183528464081777,-0.00568448980504592,0.0410317662955944));
#43123=CARTESIAN_POINT('',(-0.0180088712099482,-0.00667252564303641,0.0410576537661434));
#43124=CARTESIAN_POINT('',(-0.0177787547011939,-0.00725516830706239,0.041073083335469));
#43125=CARTESIAN_POINT('',(-0.0176157987395533,-0.00763941139942041,0.0410833716631891));
#43126=CARTESIAN_POINT('',(-0.0174129376544513,-0.00809625754586341,0.0410957602633943));
#43127=CARTESIAN_POINT('',(-0.0171024529019984,-0.00874270830779054,0.0411136159336686));
#43128=CARTESIAN_POINT('',(-0.0166971635643165,-0.00949179650613317,0.0411349193872462));
#43129=CARTESIAN_POINT('',(-0.0163498797803306,-0.0100690098818459,0.0411518194785876));
#43130=CARTESIAN_POINT('',(-0.0161395567634752,-0.0104015023515241,0.0411617007389796));
#43131=CARTESIAN_POINT('',(-0.0159536165111858,-0.0106840701655911,0.041170204502041));
#43132=CARTESIAN_POINT('',(-0.0158288589915724,-0.010867525782549,0.0411757802417608));
#43133=CARTESIAN_POINT('',(-0.0156381862076702,-0.0111417113858313,0.0411841617472069));
#43134=CARTESIAN_POINT('',(-0.0153088209143396,-0.0115955027701945,0.0411982061191146));
#43135=CARTESIAN_POINT('',(-0.0149156448029552,-0.0120969775242192,0.041214101827745));
#43136=CARTESIAN_POINT('',(-0.0145132329713727,-0.0125728662887122,0.0412295875973739));
#43137=CARTESIAN_POINT('',(-0.0142075465558633,-0.0129173407929886,0.0412409994982153));
#43138=CARTESIAN_POINT('',(-0.0139460919157739,-0.0131978402099629,0.0412504731750429));
#43139=CARTESIAN_POINT('',(-0.0137678276758751,-0.0133828035863834,0.0412568064688921));
#43140=CARTESIAN_POINT('',(-0.0136555424293172,-0.0134969516717746,0.0412607492974457));
#43141=CARTESIAN_POINT('',(-0.0135992418411063,-0.0135539684744944,0.0412627210283634));
#43142=CARTESIAN_POINT('',(-0.0134352302934178,-0.0137168263728138,0.0412684062842928));
#43143=CARTESIAN_POINT('',(-0.0132579373716275,-0.0138885323308974,0.0412744781844828));
#43144=CARTESIAN_POINT('',(-0.0129382859541697,-0.0141897428025687,0.0412852846022242));
#43145=CARTESIAN_POINT('',(-0.0125174989864431,-0.0145631192702491,0.0412991295585662));
#43146=CARTESIAN_POINT('',(-0.0120576161914113,-0.0149451644540537,0.0413138536796516));
#43147=CARTESIAN_POINT('',(-0.0115178594071772,-0.0153674208124418,0.0413307452470723));
#43148=CARTESIAN_POINT('',(-0.0110975504615446,-0.0156700975264825,0.0413435336219379));
#43149=CARTESIAN_POINT('',(-0.0108386028116304,-0.0158484284729733,0.0413513286388253));
#43150=CARTESIAN_POINT('',(-0.0107453006271399,-0.0159116649237077,0.0413541314074882));
#43151=CARTESIAN_POINT('',(-0.0106893122950504,-0.0159492375281496,0.0413558140584502));
#43152=CARTESIAN_POINT('',(-0.0106829773279673,-0.0159535901620855,0.0413560053224019));
#43153=CARTESIAN_POINT('',(-0.0105608308634261,-0.0160348201908378,0.0413596787486931));
#43154=CARTESIAN_POINT('',(-0.0104376987303638,-0.0161153027447725,0.0413633632280166));
#43155=CARTESIAN_POINT('',(-0.0102020901654385,-0.0162666296622881,0.0413703793371311));
#43156=CARTESIAN_POINT('',(-0.00987146528891982,-0.0164701572903933,0.0413801137315337));
#43157=CARTESIAN_POINT('',(-0.00946462300536958,-0.0167073407298974,0.0413919325677006));
#43158=CARTESIAN_POINT('',(-0.00905315557312621,-0.016933798059228,0.0414037310715287));
#43159=CARTESIAN_POINT('',(-0.0086362788082987,-0.0171501887172174,0.0414155414712359));
#43160=CARTESIAN_POINT('',(-0.00821314098066917,-0.0173567373186424,0.0414273927491726));
#43161=CARTESIAN_POINT('',(-0.00786004973653656,-0.0175187131933612,0.0414371794146286));
#43162=CARTESIAN_POINT('',(-0.00760371557950614,-0.0176304334168209,0.0414442297417697));
#43163=CARTESIAN_POINT('',(-0.00746780894372702,-0.0176883667470539,0.0414479558176956));
#43164=CARTESIAN_POINT('',(-0.00733422672753375,-0.0177440740139076,0.0414516077630015));
#43165=CARTESIAN_POINT('',(-0.00732029263468191,-0.0177497329616383,0.0414519857541695));
#43166=CARTESIAN_POINT('',(-0.00725241481445632,-0.0177776665645231,0.041453829820565));
#43167=CARTESIAN_POINT('',(-0.00713795877204129,-0.0178241126689765,0.0414569192176163));
#43168=CARTESIAN_POINT('',(-0.00683112228250598,-0.0179457285808909,0.041465138017541));
#43169=CARTESIAN_POINT('',(-0.00633866199453227,-0.0181284176211699,0.0414781382628205));
#43170=CARTESIAN_POINT('',(-0.00569108838309847,-0.0183399452812841,0.0414949514488509));
#43171=CARTESIAN_POINT('',(-0.00512558263153796,-0.0185066345675347,0.041509481554257));
#43172=CARTESIAN_POINT('',(-0.00459315438703795,-0.018645292370458,0.0415230262911801));
#43173=CARTESIAN_POINT('',(-0.00417429553018401,-0.0187413310068665,0.0415335997738542));
#43174=CARTESIAN_POINT('',(-0.00394144610689307,-0.0187915288929255,0.0415394593793895));
#43175=CARTESIAN_POINT('',(-0.00371467452763229,-0.0188374569165726,0.0415451495876443));
#43176=CARTESIAN_POINT('',(-0.00366253993579643,-0.0188474385517718,0.0415464559038186));
#43177=CARTESIAN_POINT('',(-0.00352911882355083,-0.0188731229249262,0.0415498025895469));
#43178=CARTESIAN_POINT('',(-0.00331806670210132,-0.0189117969030331,0.0415550971105512));
#43179=CARTESIAN_POINT('',(-0.00298368362996883,-0.0189683135558426,0.0415634879824173));
#43180=CARTESIAN_POINT('',(-0.00256021784043124,-0.0190302474353696,0.0415741144451643));
#43181=CARTESIAN_POINT('',(-0.0019545748860709,-0.0191046696787996,0.0415893112575738));
#43182=CARTESIAN_POINT('',(-0.00129443594121435,-0.0191621433397765,0.0416058729550482));
#43183=CARTESIAN_POINT('',(-0.000660783499350027,-0.0191900885905044,0.0416217826982338));
#43184=CARTESIAN_POINT('',(-0.00029379549353288,-0.0191985486823184,0.0416310035722329));
#43185=CARTESIAN_POINT('',(1.40969858954864E-5,-0.0192006090827728,0.0416387469016346));
#43186=CARTESIAN_POINT('',(0.000230767535956538,-0.0191990147952285,0.0416441958506577));
#43187=CARTESIAN_POINT('',(0.000551430994764053,-0.0191932906497573,0.0416522519772854));
#43188=CARTESIAN_POINT('',(0.00109754635716764,-0.0191730128969162,0.0416659594214273));
#43189=CARTESIAN_POINT('',(0.00219831591572031,-0.0190920329812718,0.0416935604210137));
#43190=CARTESIAN_POINT('',(0.00344269095661963,-0.0189071248749801,0.0417248119050316));
#43191=CARTESIAN_POINT('',(0.00467056968104334,-0.0186312321044329,0.0417559255019949));
#43192=CARTESIAN_POINT('',(0.00542835809864762,-0.0184213500639201,0.041775291034865));
#43193=CARTESIAN_POINT('',(0.00602803088987008,-0.018231204772277,0.0417907434711645));
#43194=CARTESIAN_POINT('',(0.00639947443283039,-0.0181033265332761,0.0418003742150108));
#43195=CARTESIAN_POINT('',(0.00669540002907382,-0.017995266731838,0.0418080867822258));
#43196=CARTESIAN_POINT('',(0.00691435280541358,-0.0179123329850677,0.0418138133375932));
#43197=CARTESIAN_POINT('',(0.00710224597756983,-0.0178383401471856,0.0418187471727468));
#43198=CARTESIAN_POINT('',(0.00723788769643847,-0.0177836975605415,0.041822318358613));
#43199=CARTESIAN_POINT('',(0.00737796793752131,-0.0177259326582208,0.0418260148286403));
#43200=CARTESIAN_POINT('',(0.0073703491011212,-0.017728999212047,0.0418258185554632));
#43201=CARTESIAN_POINT('',(0.00743026231646231,-0.0177040593575576,0.0418274239460156));
#43202=CARTESIAN_POINT('',(0.00754768102226501,-0.0176545807589192,0.041830607865276));
#43203=CARTESIAN_POINT('',(0.00783884407870035,-0.0175289244893563,0.0418385612409421));
#43204=CARTESIAN_POINT('',(0.0082639897540754,-0.0173331423334386,0.0418503368030392));
#43205=CARTESIAN_POINT('',(0.00863903075263067,-0.0171473802473699,0.0418608782810132));
#43206=CARTESIAN_POINT('',(0.00886440003866057,-0.017031697285228,0.0418672614475087));
#43207=CARTESIAN_POINT('',(0.00906697043761888,-0.0169245981571955,0.0418730369652154));
#43208=CARTESIAN_POINT('',(0.00918762193876269,-0.016859220837623,0.0418764956962864));
#43209=CARTESIAN_POINT('',(0.00936854790080353,-0.0167597604756134,0.0418816979611583));
#43210=CARTESIAN_POINT('',(0.00965533299718655,-0.0165973437622871,0.0418899987202618));
#43211=CARTESIAN_POINT('',(0.0100214704002119,-0.0163794430472246,0.0419007186943628));
#43212=CARTESIAN_POINT('',(0.0103877158294851,-0.0161487428082167,0.0419115893350397));
#43213=CARTESIAN_POINT('',(0.0106637416343302,-0.0159673771450731,0.041919864041294));
#43214=CARTESIAN_POINT('',(0.0109375808148649,-0.0157813619886028,0.0419281253609799));
#43215=CARTESIAN_POINT('',(0.0113503752868312,-0.0154896219760115,0.0419406986626162));
#43216=CARTESIAN_POINT('',(0.0118123120155717,-0.0151422408651364,0.04195501523734));
#43217=CARTESIAN_POINT('',(0.012321491356983,-0.0147277402482593,0.0419712326504712));
#43218=CARTESIAN_POINT('',(0.0127219740779942,-0.0143838846105524,0.0419842492362208));
#43219=CARTESIAN_POINT('',(0.0130767671369701,-0.0140604932018218,0.0419960700187888));
#43220=CARTESIAN_POINT('',(0.013355291689487,-0.0137954574858325,0.0420055296132992));
#43221=CARTESIAN_POINT('',(0.0136034679287909,-0.013550264566355,0.0420141060557007));
#43222=CARTESIAN_POINT('',(0.0137183204603457,-0.0134333925954473,0.0420181372468344));
#43223=CARTESIAN_POINT('',(0.0139202883167972,-0.0132251853682298,0.0420252874232371));
#43224=CARTESIAN_POINT('',(0.0142560638446756,-0.0128664058736527,0.042037432434279));
#43225=CARTESIAN_POINT('',(0.0147580408957158,-0.0122936740432925,0.0420563435082996));
#43226=CARTESIAN_POINT('',(0.0153593761017835,-0.0115358160474499,0.0420804895382233));
#43227=CARTESIAN_POINT('',(0.0161783030162588,-0.0103826008409574,0.0421160151729955));
#43228=CARTESIAN_POINT('',(0.0168705072963708,-0.00920355864864432,0.0421502634638184));
#43229=CARTESIAN_POINT('',(0.0173388672004359,-0.00825584890076573,0.0421765361369678));
#43230=CARTESIAN_POINT('',(0.0175802225602196,-0.00772204446789762,0.0421910420818898));
#43231=CARTESIAN_POINT('',(0.0177351449178442,-0.00736001958369804,0.0422007585431764));
#43232=CARTESIAN_POINT('',(0.01791839444369,-0.00690302681829382,0.042212887415959));
#43233=CARTESIAN_POINT('',(0.0181347032683639,-0.00631970574701028,0.0422282156781225));
#43234=CARTESIAN_POINT('',(0.0184813777085925,-0.00527075533504568,0.0422554367547435));
#43235=CARTESIAN_POINT('',(0.0188626401710491,-0.00374447320016042,0.0422940505032));
#43236=CARTESIAN_POINT('',(0.0191384476936898,-0.00188190996108592,0.0423407335796704));
#43237=CARTESIAN_POINT('',(0.0192,-0.000627225603661956,0.0423725857024158));
#43238=CARTESIAN_POINT('',(0.0192,6.20369116582113E-17,0.0423886526967672));
#43239=CARTESIAN_POINT('',(-0.0192,-4.87313518597996E-17,0.0408877752241749));
#43240=CARTESIAN_POINT('',(0.0192,6.20369116582113E-17,0.0393882658116679));
#43241=CARTESIAN_POINT('',(0.0192,0.000628663193716255,0.0394036918705302));
#43242=CARTESIAN_POINT('',(0.0191536423955705,0.0015716580957445,0.0394269245338009));
#43243=CARTESIAN_POINT('',(0.0189995988018166,0.00281988974234687,0.0394580882726883));
#43244=CARTESIAN_POINT('',(0.0188382414158924,0.0037492807809807,0.0394815550949727));
#43245=CARTESIAN_POINT('',(0.0186314785348052,0.00466956151336681,0.0395051135719536));
#43246=CARTESIAN_POINT('',(0.0184216424502334,0.00542728908450856,0.0395248294007126));
#43247=CARTESIAN_POINT('',(0.0182318091544692,0.00602626968437309,0.0395406357785295));
#43248=CARTESIAN_POINT('',(0.0180778993213337,0.0064731679978757,0.0395525495916115));
#43249=CARTESIAN_POINT('',(0.0179422772508365,0.00683820558017339,0.0395623838627851));
#43250=CARTESIAN_POINT('',(0.0178392386001615,0.00710000322913891,0.0395695006067997));
#43251=CARTESIAN_POINT('',(0.0177842888139774,0.00723642379621665,0.0395732227865096));
#43252=CARTESIAN_POINT('',(0.0177275516131133,0.00737407443096096,0.0395769946656179));
#43253=CARTESIAN_POINT('',(0.0177269279017841,0.00737533546334951,0.0395770266010384));
#43254=CARTESIAN_POINT('',(0.0176992843382282,0.00744166518141708,0.0395788274065915));
#43255=CARTESIAN_POINT('',(0.0176452703809674,0.00756948390581538,0.0395822756645362));
#43256=CARTESIAN_POINT('',(0.017517855835472,0.00786387574531342,0.0395902105782316));
#43257=CARTESIAN_POINT('',(0.017321086347921,0.00828838647033772,0.0396017401937472));
#43258=CARTESIAN_POINT('',(0.0171201982418748,0.00869426237509275,0.0396128858976038));
#43259=CARTESIAN_POINT('',(0.0168655170512065,0.00918235348971352,0.039626424154774));
#43260=CARTESIAN_POINT('',(0.0166105763192255,0.00963499190879102,0.0396391957627629));
#43261=CARTESIAN_POINT('',(0.0163311842889985,0.0100998698300814,0.0396525411880442));
#43262=CARTESIAN_POINT('',(0.0161191538370153,0.010433383372431,0.0396622723989714));
#43263=CARTESIAN_POINT('',(0.0159700558475872,0.0106584357566633,0.039668931065234));
#43264=CARTESIAN_POINT('',(0.0159357098178215,0.0107095327692222,0.0396704576416785));
#43265=CARTESIAN_POINT('',(0.0158650123930345,0.0108143449383736,0.0396736008722819));
#43266=CARTESIAN_POINT('',(0.0157044098910281,0.0110484126310998,0.0396806832073905));
#43267=CARTESIAN_POINT('',(0.0154068004321202,0.0114651914171696,0.0396934916850739));
#43268=CARTESIAN_POINT('',(0.0149838701362527,0.0120095870647659,0.0397107595447022));
#43269=CARTESIAN_POINT('',(0.0145960079631043,0.0124793728908199,0.0397260280724261));
#43270=CARTESIAN_POINT('',(0.0142137041808713,0.0129122412610384,0.0397405073037401));
#43271=CARTESIAN_POINT('',(0.0139027461904543,0.013243082345973,0.0397518953020944));
#43272=CARTESIAN_POINT('',(0.0137258318462371,0.013426086445793,0.0397582801568527));
#43273=CARTESIAN_POINT('',(0.0135552914776017,0.0135979434580184,0.0397643542839402));
#43274=CARTESIAN_POINT('',(0.0135029522520794,0.013649591158744,0.0397661981766909));
#43275=CARTESIAN_POINT('',(0.0133905476680313,0.013760289378962,0.0397701517285016));
#43276=CARTESIAN_POINT('',(0.0132102734430134,0.0139342468568727,0.0397764216682764));
#43277=CARTESIAN_POINT('',(0.0129342562559308,0.0141920912041413,0.039785854447427));
#43278=CARTESIAN_POINT('',(0.0125936292504082,0.0144951868826209,0.0397972070581682));
#43279=CARTESIAN_POINT('',(0.0121198149179599,0.0148970802968096,0.0398126338858884));
#43280=CARTESIAN_POINT('',(0.0116161623327904,0.0152933219081227,0.0398284776193318));
#43281=CARTESIAN_POINT('',(0.0111553360265177,0.0156285127776966,0.0398425153838518));
#43282=CARTESIAN_POINT('',(0.0108767891599144,0.0158225340169491,0.0398508631983172));
#43283=CARTESIAN_POINT('',(0.0106865851100706,0.0159519407358001,0.0398565124117519));
#43284=CARTESIAN_POINT('',(0.0104072495475043,0.0161358272498322,0.0398647230396787));
#43285=CARTESIAN_POINT('',(0.0100754118146885,0.0163459399928608,0.0398743760764964));
#43286=CARTESIAN_POINT('',(0.00950035678502807,0.0166922082094278,0.0398908926449025));
#43287=CARTESIAN_POINT('',(0.00875384603134648,0.0170968957843418,0.039911845817925));
#43288=CARTESIAN_POINT('',(0.0081020794439293,0.0174100301198974,0.0399297884925825));
#43289=CARTESIAN_POINT('',(0.00770950994118586,0.0175849253891927,0.0399405133593165));
#43290=CARTESIAN_POINT('',(0.00749339191535072,0.0176775567923482,0.0399464022709833));
#43291=CARTESIAN_POINT('',(0.00736437907546044,0.0177318263720311,0.0399499177644167));
#43292=CARTESIAN_POINT('',(0.0071505137327307,0.0178193106408842,0.0399557283252957));
#43293=CARTESIAN_POINT('',(0.00689113359732511,0.0179216425000948,0.0399627320417996));
#43294=CARTESIAN_POINT('',(0.0064158681706289,0.0181004635162985,0.039975474323709));
#43295=CARTESIAN_POINT('',(0.00572142024949732,0.0183349322075204,0.0399938233931462));
#43296=CARTESIAN_POINT('',(0.00484975661297025,0.018584983346868,0.0400164652467346));
#43297=CARTESIAN_POINT('',(0.00394456205902514,0.0187982938011497,0.0400396261985757));
#43298=CARTESIAN_POINT('',(0.003006227135957,0.0189714005540031,0.040063332061757));
#43299=CARTESIAN_POINT('',(0.00219800533447482,0.0190787682971744,0.0400835415569089));
#43300=CARTESIAN_POINT('',(0.00153726200154088,0.0191405638311173,0.0400999677726655));
#43301=CARTESIAN_POINT('',(0.00103334736169756,0.019174358785584,0.0401124554130579));
#43302=CARTESIAN_POINT('',(0.000612060895325595,0.0191916623121909,0.0401228699838319));
#43303=CARTESIAN_POINT('',(0.000306057472550829,0.0191978340427517,0.0401304243073443));
#43304=CARTESIAN_POINT('',(0.000143407820939696,0.019199668352477,0.0401344378939259));
#43305=CARTESIAN_POINT('',(-1.55348747597567E-5,0.0192000906241528,0.0401383581666904));
#43306=CARTESIAN_POINT('',(-3.50474507310864E-5,0.0191999598784769,0.0401388403847884));
#43307=CARTESIAN_POINT('',(-0.000117118793954894,0.0191997380722673,0.040140870006623));
#43308=CARTESIAN_POINT('',(-0.000252801557641752,0.0191986224620844,0.0401442349505813));
#43309=CARTESIAN_POINT('',(-0.000502949885347162,0.0191943818004722,0.0401504580233786));
#43310=CARTESIAN_POINT('',(-0.000868273907348215,0.0191817450963066,0.0401595785306492));
#43311=CARTESIAN_POINT('',(-0.00130522815659472,0.0191575157563828,0.0401705187836643));
#43312=CARTESIAN_POINT('',(-0.00181110824690881,0.0191169756635091,0.0401832238751875));
#43313=CARTESIAN_POINT('',(-0.00238718143541817,0.0190542461966417,0.0401977465083337));
#43314=CARTESIAN_POINT('',(-0.00291965608528364,0.0189792585649219,0.0402112333996222));
#43315=CARTESIAN_POINT('',(-0.003328880733356,0.0189097999105468,0.0402216509659764));
#43316=CARTESIAN_POINT('',(-0.00355883570920757,0.018867675527702,0.0402275196565659));
#43317=CARTESIAN_POINT('',(-0.0037690470698942,0.0188266518728038,0.0402328975287772));
#43318=CARTESIAN_POINT('',(-0.00385425562783366,0.0188092215396048,0.0402350806262347));
#43319=CARTESIAN_POINT('',(-0.00401163409480545,0.0187765591117627,0.0402391123289397));
#43320=CARTESIAN_POINT('',(-0.00426703497988582,0.0187208549725118,0.0402456615128404));
#43321=CARTESIAN_POINT('',(-0.00464336103854244,0.0186320121818119,0.0402553284273964));
#43322=CARTESIAN_POINT('',(-0.00509133262757738,0.0185145999405918,0.0402668729231654));
#43323=CARTESIAN_POINT('',(-0.00569142929801448,0.0183417067157091,0.0402823966614816));
#43324=CARTESIAN_POINT('',(-0.00643953417939225,0.0180964887623544,0.0403018892620983));
#43325=CARTESIAN_POINT('',(-0.00764861293056902,0.0176311781153509,0.0403337429361392));
#43326=CARTESIAN_POINT('',(-0.00877194968886215,0.0170989890752868,0.0403643029732516));
#43327=CARTESIAN_POINT('',(-0.00986916205567748,0.0164784446199987,0.0403955414276563));
#43328=CARTESIAN_POINT('',(-0.0106659087537477,0.0159741691064759,0.0404189859021889));
#43329=CARTESIAN_POINT('',(-0.0114375703211447,0.0154311005462077,0.0404425334656104));
#43330=CARTESIAN_POINT('',(-0.0120574296139266,0.0149476262149671,0.0404622204711009));
#43331=CARTESIAN_POINT('',(-0.0125387719179605,0.014542803094461,0.0404780172609407));
#43332=CARTESIAN_POINT('',(-0.0128330350716999,0.014282749792635,0.0404878980331269));
#43333=CARTESIAN_POINT('',(-0.0130651746463766,0.0140697956508291,0.0404958352900833));
#43334=CARTESIAN_POINT('',(-0.0132356200633878,0.0139096531159513,0.0405017329760987));
#43335=CARTESIAN_POINT('',(-0.0133813667192793,0.0137690609604139,0.0405068445971381));
#43336=CARTESIAN_POINT('',(-0.0134849038273407,0.013667644115147,0.0405105047798711));
#43337=CARTESIAN_POINT('',(-0.0135949724049001,0.0135580215410906,0.040514430961611));
#43338=CARTESIAN_POINT('',(-0.0135788562738796,0.0135740196044398,0.0405138554096467));
#43339=CARTESIAN_POINT('',(-0.013609156462397,0.0135437116544659,0.0405149294725554));
#43340=CARTESIAN_POINT('',(-0.0136570287270167,0.013495503255589,0.0405166155567645));
#43341=CARTESIAN_POINT('',(-0.0137821312605483,0.0133684574799683,0.0405210328193024));
#43342=CARTESIAN_POINT('',(-0.0139980125105175,0.0131430334155296,0.0405287431765659));
#43343=CARTESIAN_POINT('',(-0.0142819294060527,0.0128351046817623,0.0405390791679773));
#43344=CARTESIAN_POINT('',(-0.0146270316308284,0.0124418613087138,0.0405519808968963));
#43345=CARTESIAN_POINT('',(-0.0149605400689078,0.0120380099651769,0.0405648901144448));
#43346=CARTESIAN_POINT('',(-0.0152502893023969,0.0116667906790124,0.0405764949136099));
#43347=CARTESIAN_POINT('',(-0.0154787029801495,0.0113622029530943,0.0405858757901543));
#43348=CARTESIAN_POINT('',(-0.0156742762892487,0.0110902740411778,0.0405941279021359));
#43349=CARTESIAN_POINT('',(-0.0158190296671483,0.0108814243134223,0.0406003880676495));
#43350=CARTESIAN_POINT('',(-0.0158955177767126,0.0107693260506697,0.0406037312400238));
#43351=CARTESIAN_POINT('',(-0.015973223957531,0.0106535845062456,0.0406071653818326));
#43352=CARTESIAN_POINT('',(-0.0159750842603848,0.0106506429498373,0.0406072513485023));
#43353=CARTESIAN_POINT('',(-0.016004737302427,0.0106061332989109,0.0406085702173757));
#43354=CARTESIAN_POINT('',(-0.0160457097484964,0.0105440997393347,0.0406104062489303));
#43355=CARTESIAN_POINT('',(-0.0161148626127109,0.0104383749009219,0.0406135316770759));
#43356=CARTESIAN_POINT('',(-0.0162014277246918,0.0103035414653994,0.0406175054280723));
#43357=CARTESIAN_POINT('',(-0.0163259042259946,0.0101059387085917,0.0406233082728591));
#43358=CARTESIAN_POINT('',(-0.0164954813766009,0.00982841814386152,0.0406314083422509));
#43359=CARTESIAN_POINT('',(-0.0167940372935135,0.00931475059235479,0.0406462432390558));
#43360=CARTESIAN_POINT('',(-0.0171243037635479,0.00869933678641187,0.0406637235619664));
#43361=CARTESIAN_POINT('',(-0.0174326121245624,0.00805075025151385,0.0406817399808592));
#43362=CARTESIAN_POINT('',(-0.0176037375735768,0.00766769660920411,0.040692273678032));
#43363=CARTESIAN_POINT('',(-0.0177512447249361,0.00731870166664532,0.0407017937408365));
#43364=CARTESIAN_POINT('',(-0.0178257021606035,0.00713418591542377,0.0407067907165703));
#43365=CARTESIAN_POINT('',(-0.0179457861347056,0.00682926329932022,0.0407150093377251));
#43366=CARTESIAN_POINT('',(-0.0180804566090405,0.00646589981592569,0.0407247063574043));
#43367=CARTESIAN_POINT('',(-0.0182344250697825,0.00601837778077936,0.0407365179454826));
#43368=CARTESIAN_POINT('',(-0.0183761369999105,0.00557053872483966,0.0407482083695427));
#43369=CARTESIAN_POINT('',(-0.018506876712944,0.00511941055385669,0.0407598657682243));
#43370=CARTESIAN_POINT('',(-0.0186260344845876,0.00466745886331707,0.0407714339154503));
#43371=CARTESIAN_POINT('',(-0.0187166031178119,0.00428585199186025,0.0407811136333159));
#43372=CARTESIAN_POINT('',(-0.0187737468316163,0.00402480727004834,0.0407876954822791));
#43373=CARTESIAN_POINT('',(-0.0188070377234321,0.00386494732693353,0.0407917129301286));
#43374=CARTESIAN_POINT('',(-0.0188255327189833,0.00377460196925392,0.0407939801464488));
#43375=CARTESIAN_POINT('',(-0.0188653714524608,0.00357091425566207,0.0407990812380753));
#43376=CARTESIAN_POINT('',(-0.0189069061487365,0.00334517738421681,0.0408047240798885));
#43377=CARTESIAN_POINT('',(-0.0189753331557474,0.00294439963429444,0.0408147220664482));
#43378=CARTESIAN_POINT('',(-0.0190499661576845,0.00242043706186934,0.0408277441621779));
#43379=CARTESIAN_POINT('',(-0.019113129789702,0.00185089177339893,0.040841859237278));
#43380=CARTESIAN_POINT('',(-0.0191684223934121,0.00117913314761158,0.0408584844592615));
#43381=CARTESIAN_POINT('',(-0.0191973269841242,0.00050253555781279,0.0408752334091669));
#43382=CARTESIAN_POINT('',(-0.0192,0.00013801990587612,0.0408843134849681));
#43383=CARTESIAN_POINT('',(-0.0192,0.,0.0408877752241749));
#43384=CARTESIAN_POINT('',(0.0192,2.03021822078784E-17,0.0393882658116679));
#43385=CARTESIAN_POINT('',(-0.0192,8.05624845824862E-17,0.0378887293230132));
#43386=CARTESIAN_POINT('',(-0.0192,-0.00022193889075637,0.0378942721115581));
#43387=CARTESIAN_POINT('',(-0.0191924320556616,-0.000711426082709432,0.0379064517956354));
#43388=CARTESIAN_POINT('',(-0.0191421970582481,-0.00158317381499541,0.037928054835619));
#43389=CARTESIAN_POINT('',(-0.0190535124946304,-0.0024167203864713,0.0379487073148984));
#43390=CARTESIAN_POINT('',(-0.0189554945574285,-0.00306401165003696,0.0379648016378798));
#43391=CARTESIAN_POINT('',(-0.0188907175093251,-0.00343731284693225,0.0379741079256706));
#43392=CARTESIAN_POINT('',(-0.0188290752177871,-0.00375905421228844,0.0379821470681816));
#43393=CARTESIAN_POINT('',(-0.0187880008954488,-0.00395782378144535,0.0379871310075943));
#43394=CARTESIAN_POINT('',(-0.0187212406658431,-0.00426626724610465,0.0379948956222375));
#43395=CARTESIAN_POINT('',(-0.0185978997077452,-0.00478734166477267,0.038008106411531));
#43396=CARTESIAN_POINT('',(-0.0183088332462928,-0.00584298996768977,0.0380352271895157));
#43397=CARTESIAN_POINT('',(-0.0177620834674924,-0.00737366341407103,0.0380759865548395));
#43398=CARTESIAN_POINT('',(-0.0170941518681076,-0.00878135287379402,0.0381151560081176));
#43399=CARTESIAN_POINT('',(-0.0164736157016148,-0.00987719356066384,0.0381465879808454));
#43400=CARTESIAN_POINT('',(-0.0159690984896644,-0.0106734882760038,0.0381700383824134));
#43401=CARTESIAN_POINT('',(-0.0154259711799453,-0.0114444880981995,0.0381934093609142));
#43402=CARTESIAN_POINT('',(-0.0149422694824126,-0.0120640331314217,0.0382128149599319));
#43403=CARTESIAN_POINT('',(-0.0145377336262114,-0.0125446797662033,0.0382282849050756));
#43404=CARTESIAN_POINT('',(-0.0142246821957469,-0.0128984848324273,0.0382398960222624));
#43405=CARTESIAN_POINT('',(-0.0139594876570885,-0.0131840329444294,0.0382494563292828));
#43406=CARTESIAN_POINT('',(-0.0137646375498219,-0.0133859425920867,0.0382563300866765));
#43407=CARTESIAN_POINT('',(-0.0136609215342739,-0.0134916929024351,0.0382599567853406));
#43408=CARTESIAN_POINT('',(-0.0135582188102546,-0.0135947690861585,0.0382635161110624));
#43409=CARTESIAN_POINT('',(-0.0135482786278759,-0.0136045543424977,0.038263860599836));
#43410=CARTESIAN_POINT('',(-0.0134907445988545,-0.0136617534019531,0.0382658629222794));
#43411=CARTESIAN_POINT('',(-0.0133811059120139,-0.0137695767183726,0.0382696851256903));
#43412=CARTESIAN_POINT('',(-0.013143861328283,-0.0139983997136955,0.0382779202854849));
#43413=CARTESIAN_POINT('',(-0.0128035734119893,-0.0143102267404934,0.0382895007109755));
#43414=CARTESIAN_POINT('',(-0.0124719007318678,-0.0145992794240946,0.0383005570957964));
#43415=CARTESIAN_POINT('',(-0.0120678051379103,-0.0149372183515959,0.0383138096678115));
#43416=CARTESIAN_POINT('',(-0.0116643371150943,-0.0152540441969734,0.0383267146451698));
#43417=CARTESIAN_POINT('',(-0.011234855509977,-0.0155722024727821,0.0383401487233681));
#43418=CARTESIAN_POINT('',(-0.0109586912674793,-0.0157661723475873,0.0383486214441619));
#43419=CARTESIAN_POINT('',(-0.0107718438041718,-0.0158937935027922,0.0383542934085894));
#43420=CARTESIAN_POINT('',(-0.0106822323133276,-0.015954248644862,0.0383570000856446));
#43421=CARTESIAN_POINT('',(-0.0105115727459199,-0.0160673909813946,0.0383621161608581));
#43422=CARTESIAN_POINT('',(-0.0103011824439216,-0.0162034830854251,0.0383683646498227));
#43423=CARTESIAN_POINT('',(-0.00989711393134361,-0.0164566986763136,0.0383802284704803));
#43424=CARTESIAN_POINT('',(-0.00925876527977091,-0.0168290521393271,0.0383985326419782));
#43425=CARTESIAN_POINT('',(-0.00851434895537478,-0.0172148696100751,0.0384192037589066));
#43426=CARTESIAN_POINT('',(-0.00787277575534994,-0.017514944145597,0.0384366231604828));
#43427=CARTESIAN_POINT('',(-0.00732122560114219,-0.0177521031293637,0.03845135591687));
#43428=CARTESIAN_POINT('',(-0.00688808195711684,-0.0179238650748241,0.0384627985294625));
#43429=CARTESIAN_POINT('',(-0.00627170063586758,-0.0181520498765417,0.0384789986618317));
#43430=CARTESIAN_POINT('',(-0.00552184479124476,-0.0183967910996496,0.0384985269826806));
#43431=CARTESIAN_POINT('',(-0.00477249712507726,-0.0186015961593812,0.0385178912002506));
#43432=CARTESIAN_POINT('',(-0.00426399640441388,-0.018721709547373,0.0385309854245854));
#43433=CARTESIAN_POINT('',(-0.00396222747631565,-0.0187870343587279,0.0385387451876652));
#43434=CARTESIAN_POINT('',(-0.00377408530146284,-0.0188260665630228,0.0385435837484251));
#43435=CARTESIAN_POINT('',(-0.00344526112599039,-0.018889306769233,0.0385520214470724));
#43436=CARTESIAN_POINT('',(-0.00306918572988036,-0.0189546724649684,0.0385616310948113));
#43437=CARTESIAN_POINT('',(-0.00241500810887963,-0.0190538501414187,0.0385782724945357));
#43438=CARTESIAN_POINT('',(-0.00157722589308354,-0.0191428040566018,0.0385994059960559));
#43439=CARTESIAN_POINT('',(-0.000846127191215844,-0.0191844243705943,0.0386177049419109));
#43440=CARTESIAN_POINT('',(-0.000404458241607011,-0.0191964896371516,0.0386287047575351));
#43441=CARTESIAN_POINT('',(-0.000158060393806309,-0.0191995331018626,0.0386348240862482));
#43442=CARTESIAN_POINT('',(-1.50190681013459E-5,-0.0192003620780359,0.0386383701305568));
#43443=CARTESIAN_POINT('',(0.000244723469544005,-0.0191990155180333,0.0386448002721589));
#43444=CARTESIAN_POINT('',(0.000550291329664181,-0.0191931325629526,0.0386523616897328));
#43445=CARTESIAN_POINT('',(0.00110375867659713,-0.0191728691077525,0.0386660513662283));
#43446=CARTESIAN_POINT('',(0.00188303616742212,-0.0191150910945949,0.0386853227006194));
#43447=CARTESIAN_POINT('',(0.00281814553053024,-0.018999839334807,0.0387085138769124));
#43448=CARTESIAN_POINT('',(0.00374445115215519,-0.0188391721881906,0.0387315538826043));
#43449=CARTESIAN_POINT('',(0.00466542500010175,-0.0186325272534402,0.0387547875710639));
#43450=CARTESIAN_POINT('',(0.00542285114301209,-0.0184229471939061,0.0387743875269876));
#43451=CARTESIAN_POINT('',(0.00602185387965969,-0.0182332651742008,0.0387901842335238));
#43452=CARTESIAN_POINT('',(0.00646854041601569,-0.0180795624022548,0.0388021279840688));
#43453=CARTESIAN_POINT('',(0.00683407280218434,-0.0179438377921012,0.0388120392734974));
#43454=CARTESIAN_POINT('',(0.007094917691237,-0.0178412714741173,0.0388191948946996));
#43455=CARTESIAN_POINT('',(0.00723282418127284,-0.0177857444077235,0.038822996836939));
#43456=CARTESIAN_POINT('',(0.00736587173888015,-0.0177309618253466,0.0388266838892492));
#43457=CARTESIAN_POINT('',(0.0073843861896102,-0.0177231669849029,0.0388271966167576));
#43458=CARTESIAN_POINT('',(0.00745604326299315,-0.0176932376117725,0.0388291735852158));
#43459=CARTESIAN_POINT('',(0.00757674482354925,-0.0176420940691219,0.0388324878733712));
#43460=CARTESIAN_POINT('',(0.00788956992636278,-0.0175063459502744,0.0388410446583097));
#43461=CARTESIAN_POINT('',(0.0083708008458124,-0.0172843204463115,0.0388542055739615));
#43462=CARTESIAN_POINT('',(0.00897491977693818,-0.0169761806590531,0.0388709566428017));
#43463=CARTESIAN_POINT('',(0.00948599593134554,-0.0166967382374707,0.0388853067707876));
#43464=CARTESIAN_POINT('',(0.00995430881721385,-0.0164210055546526,0.0388986682361985));
#43465=CARTESIAN_POINT('',(0.0103086527523722,-0.0161986113824786,0.0389089420525471));
#43466=CARTESIAN_POINT('',(0.0105092558920236,-0.0160689024824901,0.0389148057763633));
#43467=CARTESIAN_POINT('',(0.0106842952236901,-0.0159529058029027,0.0389199577600312));
#43468=CARTESIAN_POINT('',(0.0107789322017483,-0.0158889481787481,0.0389227606204501));
#43469=CARTESIAN_POINT('',(0.0109307821699586,-0.0157852344189826,0.0389272762278964));
#43470=CARTESIAN_POINT('',(0.0111788075288396,-0.0156116926899071,0.0389347168123635));
#43471=CARTESIAN_POINT('',(0.0116644283329899,-0.0152572781880804,0.038949522325062));
#43472=CARTESIAN_POINT('',(0.0122999567309008,-0.0147526441473697,0.0389695900374676));
#43473=CARTESIAN_POINT('',(0.0128656892406923,-0.0142571188912635,0.0389883073357696));
#43474=CARTESIAN_POINT('',(0.0132332312914574,-0.0139122800421054,0.0390009248073013));
#43475=CARTESIAN_POINT('',(0.0134250463387246,-0.0137268244149825,0.0390076227416391));
#43476=CARTESIAN_POINT('',(0.0135893314577,-0.0135639102791304,0.039013446818175));
#43477=CARTESIAN_POINT('',(0.0136534342910137,-0.0134991239603666,0.0390157417561474));
#43478=CARTESIAN_POINT('',(0.0137815513931907,-0.0133688156365421,0.0390203345378987));
#43479=CARTESIAN_POINT('',(0.0140042813904065,-0.0131370514035129,0.0390283972628939));
#43480=CARTESIAN_POINT('',(0.0143735057578032,-0.0127362066135043,0.0390420251019215));
#43481=CARTESIAN_POINT('',(0.014870950316987,-0.012154021192521,0.0390611145754916));
#43482=CARTESIAN_POINT('',(0.0154161360185727,-0.0114576829812737,0.0390831115195838));
#43483=CARTESIAN_POINT('',(0.0159938597301856,-0.0106400137371051,0.039107969709061));
#43484=CARTESIAN_POINT('',(0.0164889532961113,-0.00985023681927002,0.0391310804854158));
#43485=CARTESIAN_POINT('',(0.0168834212994582,-0.00914971785465512,0.0391510025966153));
#43486=CARTESIAN_POINT('',(0.0171270921483327,-0.00868241353400955,0.0391640558797881));
#43487=CARTESIAN_POINT('',(0.0173187007840868,-0.0082909231800945,0.0391748488202584));
#43488=CARTESIAN_POINT('',(0.0174607893482642,-0.00798736678856053,0.0391831464550681));
#43489=CARTESIAN_POINT('',(0.0175760751256471,-0.00772958500855156,0.0391901360047796));
#43490=CARTESIAN_POINT('',(0.0176578178690573,-0.0075396375228582,0.0391952537705549));
#43491=CARTESIAN_POINT('',(0.0177006367356661,-0.00743849845576918,0.0391979717800081));
#43492=CARTESIAN_POINT('',(0.0177564184460363,-0.00730445903356114,0.0392015643443123));
#43493=CARTESIAN_POINT('',(0.0177309029613751,-0.00736575644533109,0.039199922157795));
#43494=CARTESIAN_POINT('',(0.0177479902368498,-0.00732461983040761,0.0392010291412403));
#43495=CARTESIAN_POINT('',(0.0177576742445014,-0.00730107002858475,0.0392016708340031));
#43496=CARTESIAN_POINT('',(0.0177881389222152,-0.00722669586283352,0.0392036829298165));
#43497=CARTESIAN_POINT('',(0.0178400515667169,-0.00709805311807092,0.0392071590793552));
#43498=CARTESIAN_POINT('',(0.0179312400113604,-0.00686674521496964,0.0392133889812832));
#43499=CARTESIAN_POINT('',(0.0180758020447088,-0.00647910650840098,0.0392237562464804));
#43500=CARTESIAN_POINT('',(0.0182488639014487,-0.00597777556167481,0.039237046499586));
#43501=CARTESIAN_POINT('',(0.0184090657290274,-0.00546301808203981,0.0392505556512843));
#43502=CARTESIAN_POINT('',(0.0185409846123923,-0.00499208265195435,0.0392628120525489));
#43503=CARTESIAN_POINT('',(0.0186403729145296,-0.00460775037080017,0.0392727607731072));
#43504=CARTESIAN_POINT('',(0.0187212541907411,-0.00426555219765061,0.0392815728714641));
#43505=CARTESIAN_POINT('',(0.0187776536559985,-0.00400599730873853,0.0392882297681019));
#43506=CARTESIAN_POINT('',(0.0188072882778651,-0.00386419551343452,0.039291860457865));
#43507=CARTESIAN_POINT('',(0.0188349231018114,-0.00372676217679712,0.0392953739293965));
#43508=CARTESIAN_POINT('',(0.0188403362303185,-0.00369887407573525,0.039296085710669));
#43509=CARTESIAN_POINT('',(0.0188551437332107,-0.00362307015227261,0.0392980203865328));
#43510=CARTESIAN_POINT('',(0.0188771176710835,-0.00350740461657399,0.0393009673583189));
#43511=CARTESIAN_POINT('',(0.0189093718726891,-0.00333040862608833,0.0393054655665473));
#43512=CARTESIAN_POINT('',(0.0189455248915272,-0.00311812090203791,0.0393108409863942));
#43513=CARTESIAN_POINT('',(0.0189915174784813,-0.0028285052248755,0.0393181500561142));
#43514=CARTESIAN_POINT('',(0.0190439300027691,-0.0024572895851176,0.0393274732938753));
#43515=CARTESIAN_POINT('',(0.0191158601377365,-0.00184258518610987,0.0393428220638243));
#43516=CARTESIAN_POINT('',(0.019180683030258,-0.00103622452335621,0.0393628021022237));
#43517=CARTESIAN_POINT('',(0.0192,-0.000351678025297538,0.0393796363802441));
#43518=CARTESIAN_POINT('',(0.0192,6.20369116582113E-17,0.0393882658116679));
#43519=CARTESIAN_POINT('',(-0.0192,-7.15606202600399E-16,0.0378887293230132));
#43520=CARTESIAN_POINT('',(0.0192,-4.02812422912431E-17,0.0363879628538316));
#43521=CARTESIAN_POINT('',(0.0192,0.0025132741228718,0.0364504947900475));
#43522=CARTESIAN_POINT('',(0.0182002919343753,0.00753865073535335,0.0365755586624793));
#43523=CARTESIAN_POINT('',(0.0139299003749868,0.0139299426504137,0.0367631544711271));
#43524=CARTESIAN_POINT('',(0.00753880775836791,0.0182002798556818,0.0369507502797747));
#43525=CARTESIAN_POINT('',(2.09173148415435E-17,0.0196998600721591,0.0371383460884224));
#43526=CARTESIAN_POINT('',(-0.00753880775836788,0.0182002798556819,0.0373259418970701));
#43527=CARTESIAN_POINT('',(-0.0139299003749868,0.0139299426504138,0.0375135377057178));
#43528=CARTESIAN_POINT('',(-0.0182002919343753,0.00753865073535338,0.0377011335143655));
#43529=CARTESIAN_POINT('',(-0.0192,0.00251327412287184,0.0378261973867973));
#43530=CARTESIAN_POINT('',(-0.0192,0.,0.0378887293230132));
#43531=CARTESIAN_POINT('',(0.0192,-1.66086175294244E-17,0.0363879628538316));
#43532=CARTESIAN_POINT('',(-0.0192,8.05624845824862E-17,0.0348884087721565));
#43533=CARTESIAN_POINT('',(-0.0192,-0.00251327412287176,0.0349508901922263));
#43534=CARTESIAN_POINT('',(-0.0182002919343753,-0.00753865073535332,0.0350758530323659));
#43535=CARTESIAN_POINT('',(-0.0139299003749868,-0.0139299426504137,0.0352632972925753));
#43536=CARTESIAN_POINT('',(-0.00753880775836796,-0.0182002798556818,0.0354507415527847));
#43537=CARTESIAN_POINT('',(-6.58895417508622E-17,-0.0196998600721591,0.0356381858129941));
#43538=CARTESIAN_POINT('',(0.00753880775836784,-0.0182002798556819,0.0358256300732035));
#43539=CARTESIAN_POINT('',(0.0139299003749867,-0.0139299426504138,0.0360130743334129));
#43540=CARTESIAN_POINT('',(0.0182002919343753,-0.00753865073535341,0.0362005185936222));
#43541=CARTESIAN_POINT('',(0.0192,-0.00251327412287188,0.0363254814337619));
#43542=CARTESIAN_POINT('',(0.0192,-4.02812422912431E-17,0.0363879628538316));
#43543=CARTESIAN_POINT('',(0.0135622971600913,0.0138716519279114,0.0432540773782661));
#43544=CARTESIAN_POINT('',(0.0135274210106397,0.0136559761133728,0.0446813017670343));
#43545=CARTESIAN_POINT('',(0.0135093917909034,0.0136603263905846,0.0447968672191863));
#43546=CARTESIAN_POINT('',(0.0134827517892629,0.0136695662613628,0.0449835750428777));
#43547=CARTESIAN_POINT('',(0.013457778662072,0.0136941188033885,0.0452414242721579));
#43548=CARTESIAN_POINT('',(0.0134577620230351,0.0136941126402747,0.0452414232474944));
#43549=CARTESIAN_POINT('',(0.0134577729136188,0.013694124453173,0.0452414232598564));
#43550=CARTESIAN_POINT('',(0.0134431358506774,0.013708481346275,0.0444170923559122));
#43551=CARTESIAN_POINT('',(0.0134284989859897,0.0137228384410837,0.0435927614519608));
#43552=CARTESIAN_POINT('',(0.0134138623189673,0.0137371957381755,0.0427684305480228));
#43553=CARTESIAN_POINT('',(0.0134138694653129,0.0137371887554162,0.0427684291163815));
#43554=CARTESIAN_POINT('',(0.0134483181858801,0.0137035122742865,0.0430257467298376));
#43555=CARTESIAN_POINT('',(0.0134818447172915,0.0136878125844233,0.0432118318925806));
#43556=CARTESIAN_POINT('',(0.0135040830062574,0.0136794957015745,0.0433266841502101));
#43557=CARTESIAN_POINT('',(0.0138452187948272,0.013589183021651,0.0342442501353452));
#43558=CARTESIAN_POINT('',(0.013694112126519,0.0134577608686323,0.0337585747113245));
#43559=CARTESIAN_POINT('',(0.0137084811428348,0.0134431356876894,0.0345829056064801));
#43560=CARTESIAN_POINT('',(0.0137228503168215,0.0134285106616982,0.0354072365016364));
#43561=CARTESIAN_POINT('',(0.0137372196488776,0.0134138857902519,0.0362315673967792));
#43562=CARTESIAN_POINT('',(0.0137371716111379,0.0134138422538494,0.0362315674617482));
#43563=CARTESIAN_POINT('',(0.0137372123221964,0.0134138932845458,0.0362315689613074));
#43564=CARTESIAN_POINT('',(0.0137035340125068,0.0134483202299136,0.0359743257853847));
#43565=CARTESIAN_POINT('',(0.013687850265109,0.0134818048026976,0.0357884360374105));
#43566=CARTESIAN_POINT('',(0.01367954401169,0.0135039705136105,0.0356739006949439));
#43567=CARTESIAN_POINT('',(0.0136559727524296,0.0135274261730626,0.0343187419075685));
#43568=CARTESIAN_POINT('',(0.0136603243690877,0.0135093775412914,0.0342030569645028));
#43569=CARTESIAN_POINT('',(0.013669568440656,0.0134827363571335,0.0340163339693225));
#43570=CARTESIAN_POINT('',(0.0136941065780828,0.0134577665146654,0.0337585737172107));
#43571=CARTESIAN_POINT('',(0.0119111171034194,0.0152484668621677,0.0451224137724094));
#43572=CARTESIAN_POINT('',(0.0118633605503285,0.0151858282583754,0.0451430883500229));
#43573=CARTESIAN_POINT('',(0.0118233321519909,0.0151277503647984,0.0452343265114968));
#43574=CARTESIAN_POINT('',(0.0118263099903143,0.0151254220441274,0.0453156741150844));
#43575=CARTESIAN_POINT('',(0.0134200668536559,0.0140382472338094,0.0450388374046298));
#43576=CARTESIAN_POINT('',(0.013371916547268,0.0139873876325758,0.0450679237332757));
#43577=CARTESIAN_POINT('',(0.0133349840844563,0.0139462943878066,0.0451509479553486));
#43578=CARTESIAN_POINT('',(0.0133370200672889,0.0139442235544884,0.0452256332373079));
#43579=CARTESIAN_POINT('',(0.0147477564958791,0.0126583308748199,0.0450103900077387));
#43580=CARTESIAN_POINT('',(0.0146912735976177,0.0126090804528248,0.0450345912790446));
#43581=CARTESIAN_POINT('',(0.0146441359577131,0.0125657399351169,0.0451222194837998));
#43582=CARTESIAN_POINT('',(0.0146454248516105,0.01256423370876,0.0452005895299071));
#43583=CARTESIAN_POINT('',(0.0169675628741187,0.00947696062870603,0.0449137425318125));
#43584=CARTESIAN_POINT('',(0.0169025856234469,0.00944001123116975,0.0449380908423935));
#43585=CARTESIAN_POINT('',(0.016848005170986,0.00940708560671004,0.0450255531783573));
#43586=CARTESIAN_POINT('',(0.0168489449892251,0.00940539688277867,0.0451037872947182));
#43587=CARTESIAN_POINT('',(0.0178192095346987,0.00775672168733615,0.0448678738535445));
#43588=CARTESIAN_POINT('',(0.0177507059561247,0.00772628217992625,0.044892055106076));
#43589=CARTESIAN_POINT('',(0.0176928356180264,0.00769880283204781,0.0449797095415211));
#43590=CARTESIAN_POINT('',(0.01769359091967,0.00769707801660105,0.0450581013158372));
#43591=CARTESIAN_POINT('',(0.0190005468345018,0.0040841515008905,0.0447730868019316));
#43592=CARTESIAN_POINT('',(0.0189272846560822,0.00406779723084781,0.044797187650629));
#43593=CARTESIAN_POINT('',(0.0188649943920347,0.00405215796587943,0.0448849298806516));
#43594=CARTESIAN_POINT('',(0.0188654132776149,0.00405022857269431,0.0449633935072848));
#43595=CARTESIAN_POINT('',(0.0193117423498795,0.00216840122592053,0.0447245118621838));
#43596=CARTESIAN_POINT('',(0.0192374781351968,0.00215946733845291,0.0447488154351232));
#43597=CARTESIAN_POINT('',(0.0191743301485486,0.00215018981994738,0.0448363280115777));
#43598=CARTESIAN_POINT('',(0.0191745452466472,0.00214824821757985,0.0449146032877846));
#43599=CARTESIAN_POINT('',(0.0193610639046287,-0.00167360848793416,0.0446299517719903));
#43600=CARTESIAN_POINT('',(0.0192864296756519,-0.00166773435971748,0.0446542054557712));
#43601=CARTESIAN_POINT('',(0.0192225964002094,-0.00166434381837124,0.044741776704796));
#43602=CARTESIAN_POINT('',(0.019222429495433,-0.00166624131300508,0.0448201001988356));
#43603=CARTESIAN_POINT('',(0.0190948154609097,-0.00361133873910463,0.0445831374115228));
#43604=CARTESIAN_POINT('',(0.0190209425032217,-0.00359794761588151,0.0446072259517545));
#43605=CARTESIAN_POINT('',(0.0189574517013896,-0.00358812839235511,0.0446949830741052));
#43606=CARTESIAN_POINT('',(0.0189570896738194,-0.00359004606659571,0.0447734589594669));
#43607=CARTESIAN_POINT('',(0.0180142500641535,-0.00728829745566222,0.0444875269798807));
#43608=CARTESIAN_POINT('',(0.0179446383345139,-0.00726076166462538,0.0445117827641695));
#43609=CARTESIAN_POINT('',(0.0178846058775381,-0.00723881986642369,0.0445993492826507));
#43610=CARTESIAN_POINT('',(0.0178838660778194,-0.00724065009319846,0.0446776687439555));
#43611=CARTESIAN_POINT('',(0.0171862112204154,-0.00906930077004769,0.0444392374123103));
#43612=CARTESIAN_POINT('',(0.0171197971849369,-0.00903491858731672,0.0444635498466536));
#43613=CARTESIAN_POINT('',(0.0170623984036047,-0.00900705497327935,0.0445510536791123));
#43614=CARTESIAN_POINT('',(0.0170615018148729,-0.00900875217054671,0.0446293218452303));
#43615=CARTESIAN_POINT('',(0.0150748765585205,-0.0122631930816844,0.0443456129679493));
#43616=CARTESIAN_POINT('',(0.015016340754005,-0.0122163239260077,0.044369770376547));
#43617=CARTESIAN_POINT('',(0.0149652869581169,-0.0121775475694233,0.0444574509420824));
#43618=CARTESIAN_POINT('',(0.0149640799859765,-0.0121790299294539,0.0445358640882813));
#43619=CARTESIAN_POINT('',(0.0137592188484159,-0.0137228537103216,0.0442972160453779));
#43620=CARTESIAN_POINT('',(0.0137057758160768,-0.0136703779924722,0.0443214412859766));
#43621=CARTESIAN_POINT('',(0.0136589637681864,-0.0136267677645398,0.0444090425264624));
#43622=CARTESIAN_POINT('',(0.0136575692787798,-0.0136281622625707,0.0444873904791982));
#43623=CARTESIAN_POINT('',(0.0107998076932649,-0.0161550011326311,0.0442020536744408));
#43624=CARTESIAN_POINT('',(0.0107577781165153,-0.0160931658584387,0.0442263805387302));
#43625=CARTESIAN_POINT('',(0.0107205811206235,-0.016041360017213,0.0443138674388793));
#43626=CARTESIAN_POINT('',(0.0107189757689592,-0.0160424301065671,0.0443921217071986));
#43627=CARTESIAN_POINT('',(0.00911836794955619,-0.0171612888614804,0.044155115293634));
#43628=CARTESIAN_POINT('',(0.00908268800265674,-0.0170953497707791,0.044179284848013));
#43629=CARTESIAN_POINT('',(0.00905077697408364,-0.0170397763631208,0.044266952283579));
#43630=CARTESIAN_POINT('',(0.00904910958776107,-0.0170406664206737,0.044345354710046));
#43631=CARTESIAN_POINT('',(0.00556774916588638,-0.018618877334691,0.0440607028803731));
#43632=CARTESIAN_POINT('',(0.00554567972638056,-0.0185471405914764,0.0440848091125059));
#43633=CARTESIAN_POINT('',(0.00552519027181333,-0.0184862872185166,0.0441725453038299));
#43634=CARTESIAN_POINT('',(0.00552330159985229,-0.0184868557583233,0.044251003979556));
#43635=CARTESIAN_POINT('',(0.0036769985003576,-0.0190825297688914,0.0440119757378991));
#43636=CARTESIAN_POINT('',(0.00366226667577984,-0.0190092018617648,0.0440362856120546));
#43637=CARTESIAN_POINT('',(0.00364806490597945,-0.0189469874336672,0.0441237909427346));
#43638=CARTESIAN_POINT('',(0.00364614500367027,-0.0189473544278605,0.0442020602752495));
#43639=CARTESIAN_POINT('',(-0.000159073605862996,-0.0194330427739331,0.0439171161419455));
#43640=CARTESIAN_POINT('',(-0.000159036489398663,-0.0193581966471054,0.0439413856283332));
#43641=CARTESIAN_POINT('',(-0.000160633593426761,-0.0192943231817672,0.0440289388180418));
#43642=CARTESIAN_POINT('',(-0.000162539587570898,-0.0192943047059287,0.0441072474983732));
#43643=CARTESIAN_POINT('',(-0.00208280092412028,-0.0193232197787198,0.0438709143474731));
#43644=CARTESIAN_POINT('',(-0.00207532883784003,-0.0192485545634404,0.0438950384420773));
#43645=CARTESIAN_POINT('',(-0.00207059657791085,-0.0191845471658223,0.0439827552249456));
#43646=CARTESIAN_POINT('',(-0.00207254002817534,-0.0191843378177612,0.0440611980015088));
#43647=CARTESIAN_POINT('',(-0.00587164608183915,-0.0185264228724639,0.0437743901481076));
#43648=CARTESIAN_POINT('',(-0.00584959280964872,-0.0184549155034643,0.0437986739161329));
#43649=CARTESIAN_POINT('',(-0.00583237431302894,-0.0183934126817911,0.043886208785472));
#43650=CARTESIAN_POINT('',(-0.00583424921587975,-0.0183928185920857,0.0439645023066169));
#43651=CARTESIAN_POINT('',(-0.00766578626947044,-0.0178587914359639,0.0437275445893659));
#43652=CARTESIAN_POINT('',(-0.00763682180113842,-0.0177898231337236,0.043751850190935));
#43653=CARTESIAN_POINT('',(-0.00761362812625151,-0.0177303616851066,0.0438393621803527));
#43654=CARTESIAN_POINT('',(-0.00761538499953849,-0.0177296070688981,0.043917637045953));
#43655=CARTESIAN_POINT('',(-0.0110535926085533,-0.0159857022185186,0.0436330501225642));
#43656=CARTESIAN_POINT('',(-0.0110113900601718,-0.0159236454139806,0.0436571679642768));
#43657=CARTESIAN_POINT('',(-0.0109766613811024,-0.0158696554354374,0.0437448934060955));
#43658=CARTESIAN_POINT('',(-0.0109782340290061,-0.0158685674562356,0.0438233433689821));
#43659=CARTESIAN_POINT('',(-0.012581921556096,-0.0148111897659011,0.0435854931721957));
#43660=CARTESIAN_POINT('',(-0.0125338535684551,-0.0147537037166466,0.0436096942173712));
#43661=CARTESIAN_POINT('',(-0.0124940860684927,-0.0147035206656104,0.0436973228579851));
#43662=CARTESIAN_POINT('',(-0.0124955907346439,-0.0147022390336426,0.0437756932755677));
#43663=CARTESIAN_POINT('',(-0.0152554428038941,-0.0120387297395458,0.0434896423948305));
#43664=CARTESIAN_POINT('',(-0.015197109256151,-0.0119919639285616,0.0435139736236071));
#43665=CARTESIAN_POINT('',(-0.0151483977361707,-0.0119508055167351,0.0436014554263285));
#43666=CARTESIAN_POINT('',(-0.0151495935693689,-0.0119492859658235,0.0436797055035351));
#43667=CARTESIAN_POINT('',(-0.0163834997393635,-0.0104514186411031,0.0434429162689194));
#43668=CARTESIAN_POINT('',(-0.0163206232990258,-0.0104106326306365,0.0434671064785535));
#43669=CARTESIAN_POINT('',(-0.0162677931645333,-0.0103744327157288,0.0435547503556089));
#43670=CARTESIAN_POINT('',(-0.0162688141254918,-0.0103728386843743,0.043633133449291));
#43671=CARTESIAN_POINT('',(-0.0181180948755052,-0.00702795123329128,0.0433484458948482));
#43672=CARTESIAN_POINT('',(-0.018048377725369,-0.00700027368810441,0.0433725863307973));
#43673=CARTESIAN_POINT('',(-0.0179894049063615,-0.00697504552157947,0.0434602838245048));
#43674=CARTESIAN_POINT('',(-0.0179901210666772,-0.00697320868955981,0.043538710748284));
#43675=CARTESIAN_POINT('',(-0.0187328845045549,-0.00516713373106079,0.0432995252600545));
#43676=CARTESIAN_POINT('',(-0.0186609634707438,-0.0051466812890816,0.0433238478766118));
#43677=CARTESIAN_POINT('',(-0.0186000862209964,-0.0051276387903171,0.0434113389351564));
#43678=CARTESIAN_POINT('',(-0.0186006014453895,-0.00512576067388384,0.0434895965769441));
#43679=CARTESIAN_POINT('',(-0.0193827832507852,-0.00139217716998413,0.0432054268717574));
#43680=CARTESIAN_POINT('',(-0.0193081422241517,-0.00138623853652184,0.0432296697167476));
#43681=CARTESIAN_POINT('',(-0.0192445508952148,-0.00137954617751035,0.0433172534279926));
#43682=CARTESIAN_POINT('',(-0.0192446844798051,-0.00137764868123542,0.0433955871469998));
#43683=CARTESIAN_POINT('',(-0.019424673673698,0.000572591618044089,0.0431582858933068));
#43684=CARTESIAN_POINT('',(-0.0193496215132889,0.000570950790978695,0.0431823790926352));
#43685=CARTESIAN_POINT('',(-0.019285385811491,0.000571214061864182,0.0432701307623699));
#43686=CARTESIAN_POINT('',(-0.0192853283305864,0.000573170648562909,0.0433486021590327));
#43687=CARTESIAN_POINT('',(-0.0189348462154845,0.0043697410562523,0.0430627037786195));
#43688=CARTESIAN_POINT('',(-0.0188617966919163,0.00435347921143666,0.0430869761208192));
#43689=CARTESIAN_POINT('',(-0.0187990971022846,0.0043412371042362,0.0431745239086082));
#43690=CARTESIAN_POINT('',(-0.0187986540804816,0.00434315762703661,0.0432528280125303));
#43691=CARTESIAN_POINT('',(-0.0183971591744498,0.00625864624530665,0.0430145251915811));
#43692=CARTESIAN_POINT('',(-0.0183261678659743,0.00623511581432621,0.0430388357585548));
#43693=CARTESIAN_POINT('',(-0.0182651033996267,0.00621660486642616,0.0431263418765282));
#43694=CARTESIAN_POINT('',(-0.0182644858625964,0.00621841834748833,0.0432046119233684));
#43695=CARTESIAN_POINT('',(-0.0168114255453012,0.00974796456580604,0.0429208416185235));
#43696=CARTESIAN_POINT('',(-0.0167462529616046,0.00971084725244702,0.0429449893189298));
#43697=CARTESIAN_POINT('',(-0.0166897322456514,0.00968054832275472,0.0430326808335318));
#43698=CARTESIAN_POINT('',(-0.0166887718492012,0.00968220350615855,0.0431111029581461));
#43699=CARTESIAN_POINT('',(-0.015746810917611,0.0113882759971328,0.042872577634837));
#43700=CARTESIAN_POINT('',(-0.0156857861843996,0.0113448650330417,0.0428968114659125));
#43701=CARTESIAN_POINT('',(-0.0156327093668857,0.0113091695906071,0.0429844029331076));
#43702=CARTESIAN_POINT('',(-0.0156315516997354,0.0113107656680076,0.0430627428710397));
#43703=CARTESIAN_POINT('',(-0.0131979043879043,0.014263893099291,0.0427771799842653));
#43704=CARTESIAN_POINT('',(-0.0131467027239952,0.014209402593538,0.0428015048391955));
#43705=CARTESIAN_POINT('',(-0.0131018458953999,0.0141640584913093,0.0428889941244775));
#43706=CARTESIAN_POINT('',(-0.0131004299615031,0.0141653649215906,0.0429672503551503));
#43707=CARTESIAN_POINT('',(-0.0117104749854287,0.0155099910721682,0.0427307831768934));
#43708=CARTESIAN_POINT('',(-0.0116648346754129,0.0154504833966338,0.0427549392219934));
#43709=CARTESIAN_POINT('',(-0.0116245459516405,0.0154006105196224,0.0428426219902237));
#43710=CARTESIAN_POINT('',(-0.0116230404391685,0.0154017523029656,0.0429210369991081));
#43711=CARTESIAN_POINT('',(-0.0084157282397445,0.0175178646338017,0.0426357398842286));
#43712=CARTESIAN_POINT('',(-0.00838269791797529,0.0174504784084052,0.0426598557148911));
#43713=CARTESIAN_POINT('',(-0.00835293155804294,0.017393602493656,0.0427475807684539));
#43714=CARTESIAN_POINT('',(-0.00835114882150384,0.0173944633838914,0.0428260302906322));
#43715=CARTESIAN_POINT('',(-0.00664836906391361,0.0182624542001285,0.0425877615007644));
#43716=CARTESIAN_POINT('',(-0.00662222859555788,0.0181923787365993,0.0426120762142147));
#43717=CARTESIAN_POINT('',(-0.00659837148802767,0.0181331964817291,0.0426995761106777));
#43718=CARTESIAN_POINT('',(-0.00659653587630465,0.0181338616931928,0.042777840991438));
#43719=CARTESIAN_POINT('',(-0.00288750944558111,0.0192194487952228,0.0424922714769732));
#43720=CARTESIAN_POINT('',(-0.00287581787416988,0.0191455048095414,0.0425165325920182));
#43721=CARTESIAN_POINT('',(-0.00286423061226027,0.0190826492860442,0.0426040953733314));
#43722=CARTESIAN_POINT('',(-0.00286234625282073,0.0190829295288795,0.0426824119219572));
#43723=CARTESIAN_POINT('',(-0.000982578319707736,0.0194098494847792,0.0424463048591522));
#43724=CARTESIAN_POINT('',(-0.000978212251171632,0.0193349456530662,0.0424704332406481));
#43725=CARTESIAN_POINT('',(-0.000972814655148193,0.0192710005170299,0.0425581450577104));
#43726=CARTESIAN_POINT('',(-0.000970859241194737,0.0192710993398717,0.0426365837522657));
#43727=CARTESIAN_POINT('',(0.00287589180009033,0.0192202047701144,0.042349975600319));
#43728=CARTESIAN_POINT('',(0.00286539442935202,0.0191461251563339,0.0423742666714731));
#43729=CARTESIAN_POINT('',(0.00285809149226027,0.0190826922186695,0.042461793308621));
#43730=CARTESIAN_POINT('',(0.00286003397322915,0.0190824013977643,0.04254008008374));
#43731=CARTESIAN_POINT('',(0.00477346897214909,0.0188379101962389,0.0423026832697597));
#43732=CARTESIAN_POINT('',(0.00475566297139454,0.0187652520850334,0.0423269816551104));
#43733=CARTESIAN_POINT('',(0.0047420642066681,0.0187028826386092,0.0424145019720467));
#43734=CARTESIAN_POINT('',(0.00474391515520207,0.0187024134153455,0.0424927836716811));
#43735=CARTESIAN_POINT('',(0.00838993916839794,0.0175295632799056,0.0422088079806907));
#43736=CARTESIAN_POINT('',(0.00835806475986436,0.0174616169665215,0.0422329190972985));
#43737=CARTESIAN_POINT('',(0.008332296360323,0.0174028109599628,0.0423206520511072));
#43738=CARTESIAN_POINT('',(0.00833402349045457,0.0174019841115548,0.0423991081730488));
#43739=CARTESIAN_POINT('',(0.0101061585086325,0.0165984253158094,0.042160527287686));
#43740=CARTESIAN_POINT('',(0.010067698016863,0.0165341336698658,0.0421847389464463));
#43741=CARTESIAN_POINT('',(0.0100362946046989,0.0164783610062004,0.0422723555266183));
#43742=CARTESIAN_POINT('',(0.0100379807709512,0.0164773311856172,0.0423507160532588));
#43743=CARTESIAN_POINT('',(0.0131684392679074,0.0142905323206982,0.0420651643418744));
#43744=CARTESIAN_POINT('',(0.0131182003184821,0.014235164322694,0.0420894945050713));
#43745=CARTESIAN_POINT('',(0.0130765779767723,0.0141868495121099,0.0421769776058639));
#43746=CARTESIAN_POINT('',(0.0130779960586654,0.0141855391172854,0.0422552287543061));
#43747=CARTESIAN_POINT('',(0.0145429079810099,0.01288951653784,0.042018124682087));
#43748=CARTESIAN_POINT('',(0.0144871873247645,0.0128393724084036,0.0420423017411972));
#43749=CARTESIAN_POINT('',(0.0144406629767885,0.0127953267933943,0.0421299605576955));
#43750=CARTESIAN_POINT('',(0.0144419210348758,0.0127939131073594,0.0422083559096465));
#43751=CARTESIAN_POINT('',(0.0167879942968906,0.00978786677143619,0.0419237413668511));
#43752=CARTESIAN_POINT('',(0.016723506882985,0.00974958302562206,0.0419478919551198));
#43753=CARTESIAN_POINT('',(0.0166692535536996,0.00971540638638223,0.0420355776769293));
#43754=CARTESIAN_POINT('',(0.0166702533162291,0.00971369909710044,0.0421139949281423));
#43755=CARTESIAN_POINT('',(0.0176903844021271,0.00804166252515399,0.0418747153658528));
#43756=CARTESIAN_POINT('',(0.0176225658916305,0.00801018311428441,0.0418990411512617));
#43757=CARTESIAN_POINT('',(0.0175654344546478,0.00798183123197196,0.0419865287048129));
#43758=CARTESIAN_POINT('',(0.0175662368426482,0.00798005978833373,0.0420647834773854));
#43759=CARTESIAN_POINT('',(0.0189242191104922,0.00441631646227505,0.0417807159516119));
#43760=CARTESIAN_POINT('',(0.0188514220757375,0.00439873611332809,0.0418049488164648));
#43761=CARTESIAN_POINT('',(0.0187896496899181,0.00438214351233717,0.0418925439295008));
#43762=CARTESIAN_POINT('',(0.0187900792955159,0.00438029121242141,0.0419708870010681));
#43763=CARTESIAN_POINT('',(0.0192737625347307,0.00248610121336098,0.0417335775265417));
#43764=CARTESIAN_POINT('',(0.0191993895656811,0.00247593097639031,0.0417576755962962));
#43765=CARTESIAN_POINT('',(0.0191360014837637,0.0024655773417966,0.0418454216402157));
#43766=CARTESIAN_POINT('',(0.0191362522391118,0.00246363238888985,0.041923888411933));
#43767=CARTESIAN_POINT('',(0.0193860388687333,-0.0013478782594415,0.0416377966747266));
#43768=CARTESIAN_POINT('',(0.0193113542405968,-0.00134326722999368,0.0416620783959207));
#43769=CARTESIAN_POINT('',(0.0192475281217665,-0.00134100173440581,0.0417496155991939));
#43770=CARTESIAN_POINT('',(0.019247391478997,-0.00134296521202914,0.0418279110276031));
#43771=CARTESIAN_POINT('',(0.0191537270400506,-0.00328487522397506,0.0415900304891562));
#43772=CARTESIAN_POINT('',(0.0190799071367699,-0.00327281033809035,0.0416143356311441));
#43773=CARTESIAN_POINT('',(0.0190166777180566,-0.00326413751039363,0.0417018480438158));
#43774=CARTESIAN_POINT('',(0.0190163540233799,-0.00326602313964124,0.0417801232575495));
#43775=CARTESIAN_POINT('',(0.018131602323943,-0.00699439813966341,0.0414959847757827));
#43776=CARTESIAN_POINT('',(0.0180614082995736,-0.00696794459720087,0.0415201252490797));
#43777=CARTESIAN_POINT('',(0.0180008225277482,-0.00694687076797024,0.0416078248617962));
#43778=CARTESIAN_POINT('',(0.0180001325357559,-0.00694865858899434,0.0416862536254287));
#43779=CARTESIAN_POINT('',(0.0173476811165876,-0.00876108347613509,0.0414481936654002));
#43780=CARTESIAN_POINT('',(0.0172805763289672,-0.00872785066917969,0.0414724363477006));
#43781=CARTESIAN_POINT('',(0.0172225434833428,-0.00870098502212939,0.0415600177505497));
#43782=CARTESIAN_POINT('',(0.0172216523613874,-0.00870274320862069,0.0416383494356615));
#43783=CARTESIAN_POINT('',(0.0152701028102562,-0.0120213338287211,0.0413522878914658));
#43784=CARTESIAN_POINT('',(0.0152109922474703,-0.0119755308451478,0.0413766103003943));
#43785=CARTESIAN_POINT('',(0.0151595810536061,-0.0119377655573325,0.0414641024695183));
#43786=CARTESIAN_POINT('',(0.0151583887887771,-0.0119392754696399,0.041542361071393));
#43787=CARTESIAN_POINT('',(0.0140140902539154,-0.0134661964537371,0.0413065977037004));
#43788=CARTESIAN_POINT('',(0.0139596097477583,-0.0134146292067217,0.0413307404212872));
#43789=CARTESIAN_POINT('',(0.0139119301176914,-0.0133717242869215,0.0414184383077074));
#43790=CARTESIAN_POINT('',(0.0139106244354892,-0.0133730895427255,0.0414968657228129));
#43791=CARTESIAN_POINT('',(0.0110622629856551,-0.0159800311161299,0.0412109487492704));
#43792=CARTESIAN_POINT('',(0.0110190678886151,-0.0159186763628627,0.0412350758816643));
#43793=CARTESIAN_POINT('',(0.0109807473090292,-0.015867198836065,0.0413227878658976));
#43794=CARTESIAN_POINT('',(0.0109791159661971,-0.0158683335200576,0.041401226649222));
#43795=CARTESIAN_POINT('',(0.00942964141615498,-0.0169927028834982,0.0411629287682235));
#43796=CARTESIAN_POINT('',(0.00939283905067548,-0.0169276027821737,0.0411872473787582));
#43797=CARTESIAN_POINT('',(0.00936000297860796,-0.0168729037490331,0.0412747429321204));
#43798=CARTESIAN_POINT('',(0.00935829698368026,-0.0168738473224675,0.0413530042565083));
#43799=CARTESIAN_POINT('',(0.00588892122224943,-0.0185202352873659,0.0410681148857522));
#43800=CARTESIAN_POINT('',(0.00586568600622161,-0.0184490634292052,0.0410923677840248));
#43801=CARTESIAN_POINT('',(0.00584430466162974,-0.0183888183285153,0.0411799399593064));
#43802=CARTESIAN_POINT('',(0.00584248904222944,-0.0183893928036825,0.041258264213322));
#43803=CARTESIAN_POINT('',(0.00401040287879892,-0.0190152822736237,0.0410213640989462));
#43804=CARTESIAN_POINT('',(0.00399435979562309,-0.0189419983273946,0.0410454981125339));
#43805=CARTESIAN_POINT('',(0.00397901288415929,-0.0188797027745045,0.0411332034428664));
#43806=CARTESIAN_POINT('',(0.003977094168951,-0.0188801069727624,0.0412116368083255));
#43807=CARTESIAN_POINT('',(0.00019213328247138,-0.0194321011015831,0.0409255766983548));
#43808=CARTESIAN_POINT('',(0.000190813787669677,-0.0193573059724893,0.0409498744388859));
#43809=CARTESIAN_POINT('',(0.000188022001281524,-0.0192935317685946,0.0410373935668177));
#43810=CARTESIAN_POINT('',(0.000186060852112889,-0.0192935507020084,0.0411156741895074));
#43811=CARTESIAN_POINT('',(-0.00176339237332431,-0.0193524541760977,0.0408778356995182));
#43812=CARTESIAN_POINT('',(-0.00175718674408749,-0.019277896166484,0.0409021261523958));
#43813=CARTESIAN_POINT('',(-0.00175352229433959,-0.0192141535103437,0.0409896556080293));
#43814=CARTESIAN_POINT('',(-0.0017554214332428,-0.0192139805414387,0.041067944807168));
#43815=CARTESIAN_POINT('',(-0.00552669521047183,-0.0186307886709499,0.0407842954458791));
#43816=CARTESIAN_POINT('',(-0.00550590912885297,-0.0185586673831611,0.0408084000411789));
#43817=CARTESIAN_POINT('',(-0.00548971578084918,-0.0184965282212371,0.0408961402574824));
#43818=CARTESIAN_POINT('',(-0.0054915544559697,-0.0184959828695907,0.0409746023332713));
#43819=CARTESIAN_POINT('',(-0.00737943021860454,-0.0179765988957228,0.0407356098240556));
#43820=CARTESIAN_POINT('',(-0.00735152872707246,-0.0179070883826029,0.0407598318655682));
#43821=CARTESIAN_POINT('',(-0.00732926371575064,-0.0178471040041725,0.0408474366511579));
#43822=CARTESIAN_POINT('',(-0.00733108954015883,-0.0178463514792928,0.0409257875057461));
#43823=CARTESIAN_POINT('',(-0.0107539094744667,-0.0161849935846676,0.0406406636701057));
#43824=CARTESIAN_POINT('',(-0.0107130144414301,-0.0161224068015081,0.0406649920952624));
#43825=CARTESIAN_POINT('',(-0.0106795157575241,-0.0160681414903697,0.0407524772614855));
#43826=CARTESIAN_POINT('',(-0.0106811201319611,-0.0160670721568958,0.0408307301101068));
#43827=CARTESIAN_POINT('',(-0.0123287371074195,-0.0150241784256509,0.0405938515736219));
#43828=CARTESIAN_POINT('',(-0.0122816063227758,-0.0149658529672547,0.0406180147541832));
#43829=CARTESIAN_POINT('',(-0.0122425881867603,-0.0149149957976942,0.0407056893925126));
#43830=CARTESIAN_POINT('',(-0.0122440524668192,-0.0149137999712962,0.0407840977302332));
#43831=CARTESIAN_POINT('',(-0.015063442617279,-0.0122807277922009,0.0404982120005546));
#43832=CARTESIAN_POINT('',(-0.0150057002924285,-0.0122328858993998,0.0405223753795027));
#43833=CARTESIAN_POINT('',(-0.0149574411122037,-0.0121906940296751,0.0406100462467542));
#43834=CARTESIAN_POINT('',(-0.01495870084232,-0.0121891558158891,0.0406884512908035));
#43835=CARTESIAN_POINT('',(-0.0161979325896151,-0.0107387571335358,0.0404505183968822));
#43836=CARTESIAN_POINT('',(-0.0161359416433861,-0.0106969479749206,0.0404748470795084));
#43837=CARTESIAN_POINT('',(-0.0160840105493353,-0.0106599198137374,0.0405623314322008));
#43838=CARTESIAN_POINT('',(-0.0160850816918558,-0.0106582995432656,0.0406405835842443));
#43839=CARTESIAN_POINT('',(-0.0180045814485912,-0.00731727795952108,0.0403556178697589));
#43840=CARTESIAN_POINT('',(-0.0179354020292857,-0.00728854002582057,0.0403798402539448));
#43841=CARTESIAN_POINT('',(-0.0178769525958173,-0.00726249623056953,0.0404674473340524));
#43842=CARTESIAN_POINT('',(-0.017877665986857,-0.00726073419497197,0.0405458002220391));
#43843=CARTESIAN_POINT('',(-0.0186409127840566,-0.00549562960728315,0.0403091844876066));
#43844=CARTESIAN_POINT('',(-0.0185690795987422,-0.00547385462536609,0.0403332878371306));
#43845=CARTESIAN_POINT('',(-0.0185081269567373,-0.0054536303971612,0.0404210278087886));
#43846=CARTESIAN_POINT('',(-0.0185086819893113,-0.0054517463226931,0.0404994895905958));
#43847=CARTESIAN_POINT('',(-0.0193578808426837,-0.00171297754448892,0.0402130314685225));
#43848=CARTESIAN_POINT('',(-0.0192834066548136,-0.00170580555167016,0.0402373215284279));
#43849=CARTESIAN_POINT('',(-0.019220030134504,-0.00169802519972375,0.0403248493228966));
#43850=CARTESIAN_POINT('',(-0.01922020299048,-0.001696067201853,0.040403137040384));
#43851=CARTESIAN_POINT('',(-0.0194314445620402,0.000234326868795167,0.0401654061237091));
#43852=CARTESIAN_POINT('',(-0.0193566395852132,0.000234010517959497,0.0401897048712735));
#43853=CARTESIAN_POINT('',(-0.0192928221274484,0.000235378096732732,0.040277224670129));
#43854=CARTESIAN_POINT('',(-0.0192927990402418,0.000237288739506294,0.0403555059457344));
#43855=CARTESIAN_POINT('',(-0.0190071439374079,0.00404787190329747,0.0400716185672009));
#43856=CARTESIAN_POINT('',(-0.0189336516231657,0.00403281666980165,0.0400957533809963));
#43857=CARTESIAN_POINT('',(-0.0188704912700394,0.00402156036151489,0.0401834593019227));
#43858=CARTESIAN_POINT('',(-0.0188700914838369,0.00402343735438757,0.0402618932361842));
#43859=CARTESIAN_POINT('',(-0.0185019019710979,0.00594205710077393,0.040023053450417));
#43860=CARTESIAN_POINT('',(-0.0184304462375758,0.00591972522436116,0.0400473054411028));
#43861=CARTESIAN_POINT('',(-0.0183689512924275,0.00590226526823803,0.0401348762761194));
#43862=CARTESIAN_POINT('',(-0.0183683462818142,0.00590413969905943,0.0402131992968648));
#43863=CARTESIAN_POINT('',(-0.0169768882879332,0.00945543410936856,0.0399281103095153));
#43864=CARTESIAN_POINT('',(-0.0169112821115633,0.00941955212853585,0.0399524289425286));
#43865=CARTESIAN_POINT('',(-0.0168545467113079,0.00939038667184233,0.0400399254990433));
#43866=CARTESIAN_POINT('',(-0.0168536093313915,0.00939206384238749,0.0401181877041794));
#43867=CARTESIAN_POINT('',(-0.01593535832353,0.0111223090713971,0.0398812109428551));
#43868=CARTESIAN_POINT('',(-0.0158735159105026,0.0110798324171594,0.0399053389666608));
#43869=CARTESIAN_POINT('',(-0.0158197278755644,0.0110448507473462,0.0399930533704728));
#43870=CARTESIAN_POINT('',(-0.0158186484123805,0.0110464051239283,0.0400714943318944));
#43871=CARTESIAN_POINT('',(-0.0134454518985074,0.0140306589988565,0.0397865925416715));
#43872=CARTESIAN_POINT('',(-0.0133931288274549,0.013976916359118,0.0398107342991805));
#43873=CARTESIAN_POINT('',(-0.0133471833957635,0.0139321647231977,0.0398984295500356));
#43874=CARTESIAN_POINT('',(-0.0133457485652741,0.0139335458153675,0.0399768545933033));
#43875=CARTESIAN_POINT('',(-0.011960751940929,0.0153155583646799,0.0397375831615763));
#43876=CARTESIAN_POINT('',(-0.0119142639235653,0.0152569925928259,0.0397619054231763));
#43877=CARTESIAN_POINT('',(-0.0118733169879335,0.0152080831693273,0.0398493969333267));
#43878=CARTESIAN_POINT('',(-0.0118717815028061,0.0152092790370377,0.0399276549481262));
#43879=CARTESIAN_POINT('',(-0.00872162776691554,0.0173657492824739,0.0396434082267646));
#43880=CARTESIAN_POINT('',(-0.00868750821375636,0.0172990977852855,0.039667651378194));
#43881=CARTESIAN_POINT('',(-0.00865693076962195,0.0172429405691964,0.0397552346856925));
#43882=CARTESIAN_POINT('',(-0.00865522841726458,0.0172437926779991,0.0398335680705144));
#43883=CARTESIAN_POINT('',(-0.00693350364422637,0.0181547616987217,0.0395962668314319));
#43884=CARTESIAN_POINT('',(-0.00690620437943324,0.0180848943918416,0.0396204075659489));
#43885=CARTESIAN_POINT('',(-0.00688130993302412,0.018025776493363,0.0397081051752782));
#43886=CARTESIAN_POINT('',(-0.00687947509641899,0.0180264764200233,0.0397865321992344));
#43887=CARTESIAN_POINT('',(-0.00322453524254062,0.0191637764355218,0.0395004073005348));
#43888=CARTESIAN_POINT('',(-0.00321155329862424,0.019090113767052,0.0395247123010259));
#43889=CARTESIAN_POINT('',(-0.00319884187363129,0.0190275709231919,0.0396122232568542));
#43890=CARTESIAN_POINT('',(-0.00319691082962554,0.0190278950720074,0.0396904971845612));
#43891=CARTESIAN_POINT('',(-0.00129919072967843,0.0193905845890196,0.0394532179801282));
#43892=CARTESIAN_POINT('',(-0.00129360490319829,0.0193159612092455,0.0394775000810617));
#43893=CARTESIAN_POINT('',(-0.00128721010180883,0.0192524133851804,0.0395650391559288));
#43894=CARTESIAN_POINT('',(-0.00128530982278602,0.0192525411077439,0.0396433362491825));
#43895=CARTESIAN_POINT('',(0.00255902787432145,0.0192654480198307,0.0393589678198288));
#43896=CARTESIAN_POINT('',(0.00254972219577876,0.0191909555052613,0.0393830652854638));
#43897=CARTESIAN_POINT('',(0.00254340208585965,0.0191270341900853,0.0394708134257302));
#43898=CARTESIAN_POINT('',(0.00254530713983667,0.0191267815381943,0.0395492819968932));
#43899=CARTESIAN_POINT('',(0.00444305415507311,0.018920683340969,0.0393114195738665));
#43900=CARTESIAN_POINT('',(0.0044265025633268,0.018847634599306,0.0393356514402658));
#43901=CARTESIAN_POINT('',(0.00441401087617363,0.0187848918998344,0.0394232450563293));
#43902=CARTESIAN_POINT('',(0.00441593234193343,0.0187844376529192,0.0395015867513894));
#43903=CARTESIAN_POINT('',(0.0081155234358224,0.017659536267152,0.0392150014766233));
#43904=CARTESIAN_POINT('',(0.0080848214364896,0.0175913526381763,0.0392393282335753));
#43905=CARTESIAN_POINT('',(0.00806013444744089,0.0175325379856509,0.0393268154080085));
#43906=CARTESIAN_POINT('',(0.0080618825123445,0.0175317314245367,0.0394050699108451));
#43907=CARTESIAN_POINT('',(0.00981354217592872,0.0167748457507326,0.0391692829636585));
#43908=CARTESIAN_POINT('',(0.00977615945611022,0.0167098257968652,0.0391934345795327));
#43909=CARTESIAN_POINT('',(0.0097456154724898,0.0166534461042345,0.0392811220489701));
#43910=CARTESIAN_POINT('',(0.00974725611746331,0.0166524908972105,0.0393595408978778));
#43911=CARTESIAN_POINT('',(0.0129360951432808,0.0145036320981578,0.0390738099458165));
#43912=CARTESIAN_POINT('',(0.0128866379295421,0.0144472916781401,0.0390979857807174));
#43913=CARTESIAN_POINT('',(0.0128456567142085,0.0143980343100778,0.0391856425630789));
#43914=CARTESIAN_POINT('',(0.0128471421335855,0.0143967146912262,0.0392640360535999));
#43915=CARTESIAN_POINT('',(0.0143150193080017,0.0131425534125171,0.0390256063403529));
#43916=CARTESIAN_POINT('',(0.0142603468414684,0.0130915547374476,0.0390499362984668));
#43917=CARTESIAN_POINT('',(0.0142148599328177,0.0130468555414553,0.0391374193147547));
#43918=CARTESIAN_POINT('',(0.0142161697159497,0.0130454253788721,0.0392156703759364));
#43919=CARTESIAN_POINT('',(0.0166225528799177,0.010067382546611,0.038931373355256));
#43920=CARTESIAN_POINT('',(0.0165587714851361,0.0100280789617687,0.0389555861269347));
#43921=CARTESIAN_POINT('',(0.016505154392705,0.00999312567443186,0.0390432041584913));
#43922=CARTESIAN_POINT('',(0.0165061370301603,0.0099914986388418,0.0391215660289867));
#43923=CARTESIAN_POINT('',(0.0175492105589036,0.00834737793199038,0.0388842404592576));
#43924=CARTESIAN_POINT('',(0.0174816865750995,0.00831462399998431,0.0389083509308422));
#43925=CARTESIAN_POINT('',(0.017424670543974,0.00828510605380299,0.0389960827451585));
#43926=CARTESIAN_POINT('',(0.0174255147527736,0.00828332962245758,0.0390745378270751));
#43927=CARTESIAN_POINT('',(0.0188458641467242,0.00473953216237909,0.0387884879194788));
#43928=CARTESIAN_POINT('',(0.0187734603459155,0.00472072645929015,0.0388127852373821));
#43929=CARTESIAN_POINT('',(0.018712115027066,0.00470307102651411,0.0389003048529412));
#43930=CARTESIAN_POINT('',(0.018712593041949,0.00470116748051165,0.0389785858691391));
#43931=CARTESIAN_POINT('',(0.019227674046985,0.00281385318638663,0.0387405884459633));
#43932=CARTESIAN_POINT('',(0.0191537355807173,0.00280244196433158,0.0387648797081903));
#43933=CARTESIAN_POINT('',(0.0190909074720484,0.00279109067856667,0.0388524081339661));
#43934=CARTESIAN_POINT('',(0.0190911840350891,0.00278920249838559,0.0389306964894435));
#43935=CARTESIAN_POINT('',(0.019406698543977,-0.00101085205758943,0.0386469886990866));
#43936=CARTESIAN_POINT('',(0.0193317482426553,-0.00100753253556381,0.0386711182270064));
#43937=CARTESIAN_POINT('',(0.0192675947531134,-0.00100634376061779,0.0387588300103844));
#43938=CARTESIAN_POINT('',(0.0192674949877194,-0.0010082635254978,0.0388372687487328));
#43939=CARTESIAN_POINT('',(0.019204959553772,-0.00296586744453016,0.0385982170171152));
#43940=CARTESIAN_POINT('',(0.0191308966912634,-0.00295502470244232,0.0386224780246699));
#43941=CARTESIAN_POINT('',(0.0190674416992468,-0.00294743087934119,0.0387100386227964));
#43942=CARTESIAN_POINT('',(0.0190671383876761,-0.00294937568700589,0.0387883532508879));
#43943=CARTESIAN_POINT('',(0.0182501324132737,-0.00667478502307092,0.0385033576663385));
#43944=CARTESIAN_POINT('',(0.018179703890677,-0.0066496385805664,0.0385276720163145));
#43945=CARTESIAN_POINT('',(0.0181190878376674,-0.00662973132821225,0.0386151735487677));
#43946=CARTESIAN_POINT('',(0.0181184260275392,-0.00663153236608867,0.0386934398400686));
#43947=CARTESIAN_POINT('',(0.0174853534374695,-0.00848057633974107,0.0384566148691321));
#43948=CARTESIAN_POINT('',(0.0174175894303183,-0.00844833684682815,0.0384807306646094));
#43949=CARTESIAN_POINT('',(0.0173589470012821,-0.00842223583780885,0.0385684586167564));
#43950=CARTESIAN_POINT('',(0.0173581210465426,-0.00842394795680733,0.0386469106780912));
#43951=CARTESIAN_POINT('',(0.0154785716070732,-0.0117501651746574,0.0383616497868883));
#43952=CARTESIAN_POINT('',(0.015418486581854,-0.0117052963656775,0.0383858059075054));
#43953=CARTESIAN_POINT('',(0.0153661184052046,-0.0116683119178918,0.0384734849231699));
#43954=CARTESIAN_POINT('',(0.0153649179745633,-0.0116698997887883,0.0385518966467288));
#43955=CARTESIAN_POINT('',(0.0142234376982746,-0.0132419648869437,0.0383130552616885));
#43956=CARTESIAN_POINT('',(0.0141683093057633,-0.0131914491972484,0.0383373804449651));
#43957=CARTESIAN_POINT('',(0.0141201762729626,-0.0131495973635277,0.0384248687309179));
#43958=CARTESIAN_POINT('',(0.0141188501423668,-0.0131510181564485,0.0385031241067679));
#43959=CARTESIAN_POINT('',(0.0113346703524442,-0.0157858406654838,0.0382185630351736));
#43960=CARTESIAN_POINT('',(0.0112905221373944,-0.0157253443158286,0.0382427966886846));
#43961=CARTESIAN_POINT('',(0.0112515123813048,-0.0156746533547692,0.0383303908380344));
#43962=CARTESIAN_POINT('',(0.0112499648737552,-0.0156757614881421,0.0384087331156003));
#43963=CARTESIAN_POINT('',(0.00971288679571012,-0.0168337228282251,0.0381719175555109));
#43964=CARTESIAN_POINT('',(0.00967490223484882,-0.0167690440392301,0.0381960644883469));
#43965=CARTESIAN_POINT('',(0.00964099001599442,-0.0167146052157371,0.0382837549903342));
#43966=CARTESIAN_POINT('',(0.00963928646524814,-0.0167155869636415,0.0383621761779478));
#43967=CARTESIAN_POINT('',(0.00618680655579516,-0.0184232718057472,0.0380754658022996));
#43968=CARTESIAN_POINT('',(0.00616244848485818,-0.0183525547089153,0.0380997768839514));
#43969=CARTESIAN_POINT('',(0.00614010314766136,-0.0182927813444199,0.0381872809991016));
#43970=CARTESIAN_POINT('',(0.00613824926368048,-0.0182934028293015,0.0382655493232916));
#43971=CARTESIAN_POINT('',(0.00434434565899893,-0.0189430548430776,0.0380289637754413));
#43972=CARTESIAN_POINT('',(0.00432704675323807,-0.0188702357548829,0.0380532377199637));
#43973=CARTESIAN_POINT('',(0.00431069790203453,-0.0188084759455217,0.0381407861665265));
#43974=CARTESIAN_POINT('',(0.00430884367707529,-0.0188089018960293,0.038219090950365));
#43975=CARTESIAN_POINT('',(0.00049971302025047,-0.019428998627159,0.0379343239189305));
#43976=CARTESIAN_POINT('',(0.000497198041504029,-0.0193539599551106,0.0379584163646268));
#43977=CARTESIAN_POINT('',(0.000493392381103726,-0.0192898275737404,0.0380461700429039));
#43978=CARTESIAN_POINT('',(0.000491467655240249,-0.0192898777578237,0.0381246431523179));
#43979=CARTESIAN_POINT('',(-0.00142299260754889,-0.0193817406272071,0.0378864924453864));
#43980=CARTESIAN_POINT('',(-0.00141809504677111,-0.0193070186093912,0.0379107340192279));
#43981=CARTESIAN_POINT('',(-0.00141559149936843,-0.0192431173300155,0.0379983166189465));
#43982=CARTESIAN_POINT('',(-0.00141755890393027,-0.0192429698914113,0.0380766492816992));
#43983=CARTESIAN_POINT('',(-0.00522021770879957,-0.0187193940741252,0.0377908527938189));
#43984=CARTESIAN_POINT('',(-0.00520068545450459,-0.0186472141752514,0.037815176260299));
#43985=CARTESIAN_POINT('',(-0.00518560869929645,-0.0185852340872855,0.0379026672625595));
#43986=CARTESIAN_POINT('',(-0.00518745998008488,-0.0185847147527988,0.0379809249098162));
#43987=CARTESIAN_POINT('',(-0.00706460087853033,-0.0181039357281884,0.0377444334742754));
#43988=CARTESIAN_POINT('',(-0.00703786096634784,-0.0180338545865875,0.0377685751215507));
#43989=CARTESIAN_POINT('',(-0.00701652477839413,-0.017973368867882,0.0378562736143509));
#43990=CARTESIAN_POINT('',(-0.00701830189552598,-0.017972679116116,0.0379347014913153));
#43991=CARTESIAN_POINT('',(-0.0104861914121819,-0.0163613825910883,0.0376493565744482));
#43992=CARTESIAN_POINT('',(-0.0104462485127058,-0.0162979652177063,0.0376735450790744));
#43993=CARTESIAN_POINT('',(-0.0104135603769271,-0.0162428867200877,0.0377611875441761));
#43994=CARTESIAN_POINT('',(-0.0104152336700229,-0.0162418183620689,0.0378395692912002));
#43995=CARTESIAN_POINT('',(-0.01207891400749,-0.0152223783460422,0.037600711886929));
#43996=CARTESIAN_POINT('',(-0.012032908068334,-0.0151634470378172,0.0376250425234767));
#43997=CARTESIAN_POINT('',(-0.0119949858388776,-0.0151121779194518,0.0377125248898505));
#43998=CARTESIAN_POINT('',(-0.0119965012289499,-0.0151109726135702,0.0377907754230611));
#43999=CARTESIAN_POINT('',(-0.0148311285373011,-0.0125568682379528,0.0375068681710913));
#44000=CARTESIAN_POINT('',(-0.0147743172321318,-0.0125080120355757,0.0375310707473459));
#44001=CARTESIAN_POINT('',(-0.0147268542025376,-0.0124650460047888,0.0376187003831675));
#44002=CARTESIAN_POINT('',(-0.0147280807018185,-0.0124635939401517,0.0376970717716093));
#44003=CARTESIAN_POINT('',(-0.016023338217248,-0.0109952313659276,0.0374593571749295));
#44004=CARTESIAN_POINT('',(-0.0159617938164897,-0.0109523019516451,0.0374834754164168));
#44005=CARTESIAN_POINT('',(-0.0159101251848468,-0.01091421724169,0.0375711983470121));
#44006=CARTESIAN_POINT('',(-0.0159112385943021,-0.0109125929807456,0.037649646134008));
#44007=CARTESIAN_POINT('',(-0.0178674960710242,-0.00764011945348385,0.0373637399470384));
#44008=CARTESIAN_POINT('',(-0.0177989527475963,-0.00761018147434739,0.037388044166753));
#44009=CARTESIAN_POINT('',(-0.0177411529848847,-0.00758312021038884,0.0374755560085341));
#44010=CARTESIAN_POINT('',(-0.0177419225641817,-0.00758131801831355,0.0375538306562103));
#44011=CARTESIAN_POINT('',(-0.018547838985748,-0.00579698411247787,0.0373158897342672));
#44012=CARTESIAN_POINT('',(-0.018476597245384,-0.00577410683765023,0.0373401729609822));
#44013=CARTESIAN_POINT('',(-0.0184163133217148,-0.00575303272943732,0.0374277106322001));
#44014=CARTESIAN_POINT('',(-0.0184168824207991,-0.00575121365323234,0.0375060065749605));
#44015=CARTESIAN_POINT('',(-0.0193252414788857,-0.00204511672800822,0.0372222028343277));
#44016=CARTESIAN_POINT('',(-0.0192506917089206,-0.00203663972521744,0.037246327760038));
#44017=CARTESIAN_POINT('',(-0.0191871368143089,-0.00202774823372296,0.0373340446144194));
#44018=CARTESIAN_POINT('',(-0.0191873400309585,-0.00202583294549132,0.0374124875069261));
#44019=CARTESIAN_POINT('',(-0.0194329094916537,-9.05799127225192E-5,0.0371735521390737));
#44020=CARTESIAN_POINT('',(-0.0193580721245975,-8.96423798313532E-5,0.037197821703061));
#44021=CARTESIAN_POINT('',(-0.0192942275335136,-8.71651879981286E-5,0.0372853725909127));
#44022=CARTESIAN_POINT('',(-0.0192942337078952,-8.51982643077479E-5,0.0373636792586044));
#44023=CARTESIAN_POINT('',(-0.0190711042104053,0.00373284239430641,0.0370785083301443));
#44024=CARTESIAN_POINT('',(-0.0189975972718238,0.00371904031452049,0.0371028178672844));
#44025=CARTESIAN_POINT('',(-0.0189345998782528,0.00370887329893731,0.0371903249792992));
#44026=CARTESIAN_POINT('',(-0.0189342288561442,0.00371075339281345,0.0372685958514727));
#44027=CARTESIAN_POINT('',(-0.0186041912754882,0.00561953539167989,0.0370322289124419));
#44028=CARTESIAN_POINT('',(-0.0185321777911545,0.00559837272669547,0.0370563348311793));
#44029=CARTESIAN_POINT('',(-0.0184701313765664,0.0055818380789744,0.0371440737029468));
#44030=CARTESIAN_POINT('',(-0.0184695829373792,0.00558366615936054,0.0372225347088254));
#44031=CARTESIAN_POINT('',(-0.0171287473134776,0.00918111797110836,0.0369366617089299));
#44032=CARTESIAN_POINT('',(-0.0170623892396143,0.00914621971976329,0.0369608316648687));
#44033=CARTESIAN_POINT('',(-0.0170048970494583,0.00911790250396981,0.0370484950420105));
#44034=CARTESIAN_POINT('',(-0.0170039602345416,0.00911965777877905,0.0371268939357847));
#44035=CARTESIAN_POINT('',(-0.0161383648576022,0.0108287162688267,0.0368888128118898));
#44036=CARTESIAN_POINT('',(-0.0160759447578151,0.0107875457132842,0.0369131404453162));
#44037=CARTESIAN_POINT('',(-0.0160218041980741,0.0107538247362759,0.0370006260387094));
#44038=CARTESIAN_POINT('',(-0.0160207207046064,0.0107554352591012,0.0370788792111389));
#44039=CARTESIAN_POINT('',(-0.0136685562721545,0.0138163527932191,0.036793714225605));
#44040=CARTESIAN_POINT('',(-0.0136154643792597,0.013763507738302,0.0368179391952823));
#44041=CARTESIAN_POINT('',(-0.0135689795293521,0.0137195390091569,0.0369055432451919));
#44042=CARTESIAN_POINT('',(-0.0135676247970923,0.0137208759513757,0.0369838936430815));
#44043=CARTESIAN_POINT('',(-0.0122429028720005,0.015093799560696,0.0367473781171091));
#44044=CARTESIAN_POINT('',(-0.0121952121305115,0.0150359205009187,0.0367715340771391));
#44045=CARTESIAN_POINT('',(-0.0121531586006765,0.0149875174588499,0.0368592142794031));
#44046=CARTESIAN_POINT('',(-0.0121516297248808,0.0149887559101737,0.0369376270142908));
#44047=CARTESIAN_POINT('',(-0.00901201976866163,0.0172184505126157,0.0366509953904922));
#44048=CARTESIAN_POINT('',(-0.00897682626097934,0.0171524556408082,0.0366753079862759));
#44049=CARTESIAN_POINT('',(-0.00894534739833079,0.0170969501197653,0.0367628104930834));
#44050=CARTESIAN_POINT('',(-0.00894361782180382,0.0170978539285752,0.0368410775073646));
#44051=CARTESIAN_POINT('',(-0.00725761413657459,0.0180274818560194,0.0366041627325707));
#44052=CARTESIAN_POINT('',(-0.00722911762950855,0.0179582554483319,0.0366284200075637));
#44053=CARTESIAN_POINT('',(-0.00720328902087814,0.0178997914362247,0.036715987498159));
#44054=CARTESIAN_POINT('',(-0.00720152656681416,0.0179005021385607,0.0367943079070936));
#44055=CARTESIAN_POINT('',(-0.00356301574194221,0.0191046951564421,0.0365101062998508));
#44056=CARTESIAN_POINT('',(-0.00354867545444478,0.0190309967968961,0.0365341948820525));
#44057=CARTESIAN_POINT('',(-0.00353477906593163,0.0189682693791576,0.0366219526836391));
#44058=CARTESIAN_POINT('',(-0.00353288083809403,0.018968624480678,0.0367004291670056));
#44059=CARTESIAN_POINT('',(-0.00163030801356091,0.0193644544794528,0.0364615160434953));
#44060=CARTESIAN_POINT('',(-0.00162344145580831,0.0192899054784977,0.0364857686894514));
#44061=CARTESIAN_POINT('',(-0.00161590810152796,0.0192264253025067,0.0365733387767667));
#44062=CARTESIAN_POINT('',(-0.00161394540795644,0.0192265874866579,0.0366516611856013));
#44063=CARTESIAN_POINT('',(0.00220542883222762,0.0193072407402312,0.0363665104815927));
#44064=CARTESIAN_POINT('',(0.00219751083367931,0.019232863449794,0.0363908148325363));
#44065=CARTESIAN_POINT('',(0.00219238166704181,0.0191692475419351,0.0364783278268363));
#44066=CARTESIAN_POINT('',(0.0021942866525446,0.0191690268988398,0.0365566035194738));
#44067=CARTESIAN_POINT('',(0.00414051581960644,0.0189869253580856,0.0363198423738946));
#44068=CARTESIAN_POINT('',(0.00412506819282153,0.0189134636193086,0.0363439366760617));
#44069=CARTESIAN_POINT('',(0.00411344152877879,0.0188502961119186,0.0364316890676605));
#44070=CARTESIAN_POINT('',(0.00411529796524559,0.0188498963213753,0.0365101611861028));
#44071=CARTESIAN_POINT('',(0.00778328794413445,0.0178060518634451,0.0362247298311951));
#44072=CARTESIAN_POINT('',(0.00775381675083955,0.0177371450529443,0.0362489191090306));
#44073=CARTESIAN_POINT('',(0.00773021475367226,0.0176776085770064,0.0363365599232303));
#44074=CARTESIAN_POINT('',(0.00773205627627711,0.0176768089430711,0.0364149402666696));
#44075=CARTESIAN_POINT('',(0.00954191235829089,0.0169280969611422,0.0361755156541392));
#44076=CARTESIAN_POINT('',(0.00950576273114558,0.0168627489131564,0.0361999086999894));
#44077=CARTESIAN_POINT('',(0.00947641473143195,0.0168062726093583,0.0362873196956842));
#44078=CARTESIAN_POINT('',(0.00947809970864682,0.0168053194180008,0.0363655117092009));
#44079=CARTESIAN_POINT('',(0.0118927992392535,0.0152786627980386,0.0361053928098151));
#44080=CARTESIAN_POINT('',(0.011847441887544,0.0152194627746643,0.0361296548029672));
#44081=CARTESIAN_POINT('',(0.0118100144218005,0.0151679553925195,0.0362172168520969));
#44082=CARTESIAN_POINT('',(0.0118115059446032,0.0151667930370143,0.0362955328114932));
#44083=CARTESIAN_POINT('',(0.0126350496435506,0.0146717197127624,0.0360823098046397));
#44084=CARTESIAN_POINT('',(0.0125867368716098,0.0146147506638112,0.0361064821793622));
#44085=CARTESIAN_POINT('',(0.0125466876309365,0.0145650265432641,0.0361941461617745));
#44086=CARTESIAN_POINT('',(0.0125481200948318,0.0145637940948934,0.0362725457412689));
#44087=CARTESIAN_POINT('',(0.0140340189138294,0.0133400741878172,0.0360349618928478));
#44088=CARTESIAN_POINT('',(0.0139802254604343,0.0132881392002742,0.0360590753278414));
#44089=CARTESIAN_POINT('',(0.0139353786065701,0.0132425296678159,0.036146804178451));
#44090=CARTESIAN_POINT('',(0.0139367178904866,0.0132411219612905,0.0362252568760622));
#44091=CARTESIAN_POINT('',(0.0146866155034336,0.0126151004153065,0.0360103473893038));
#44092=CARTESIAN_POINT('',(0.0146304266947731,0.0125664053612895,0.0360352070928211));
#44093=CARTESIAN_POINT('',(0.0145834087095037,0.0125248397387306,0.0361224688604089));
#44094=CARTESIAN_POINT('',(0.0145837132301085,0.012524467394925,0.0362005916858531));
#44095=CARTESIAN_POINT('',(0.0152851838289805,0.0118641087528759,0.0360041770055195));
#44096=CARTESIAN_POINT('',(0.0152229754605671,0.011815747174396,0.0360248428028356));
#44097=CARTESIAN_POINT('',(0.0151674788425261,0.0117723228643604,0.0361162090430061));
#44098=CARTESIAN_POINT('',(0.0151676306139985,0.0117721273165599,0.0361976690778631));
#44099=CARTESIAN_POINT('',(0.0143467680811991,0.0129670203653367,0.0450227433592973));
#44100=CARTESIAN_POINT('',(0.0156080128040208,0.0115714355419396,0.0449758659317047));
#44101=CARTESIAN_POINT('',(0.0172066386543741,0.00917185028715237,0.0449045572620493));
#44102=CARTESIAN_POINT('',(0.0185655005786739,0.00565703064731983,0.0448135755705688));
#44103=CARTESIAN_POINT('',(0.0191945950678217,0.00286361278847597,0.0447419841407263));
#44104=CARTESIAN_POINT('',(0.0194071949470191,6.00777136899667E-5,0.044672388798418));
#44105=CARTESIAN_POINT('',(0.0192041015517058,-0.0028054344836469,0.0446027222502955));
#44106=CARTESIAN_POINT('',(0.0185964962403323,-0.0055510102664849,0.0445333817125042));
#44107=CARTESIAN_POINT('',(0.0172386864719429,-0.00911657052892957,0.0444379929122851));
#44108=CARTESIAN_POINT('',(0.0151500718616308,-0.0122793685668817,0.0443473875819632));
#44109=CARTESIAN_POINT('',(0.0124063985660361,-0.0149232657153125,0.0442521229497016));
#44110=CARTESIAN_POINT('',(0.010117578367962,-0.0165615924118944,0.0441828847762095));
#44111=CARTESIAN_POINT('',(0.00756285891478142,-0.0178737072130057,0.0441133626517729));
#44112=CARTESIAN_POINT('',(0.00490243177550567,-0.0187778915477432,0.0440434614272629));
#44113=CARTESIAN_POINT('',(0.0020822622425663,-0.0192952805907951,0.0439720759472064));
#44114=CARTESIAN_POINT('',(-0.00167918760469326,-0.0194268328273352,0.0438807494904873));
#44115=CARTESIAN_POINT('',(-0.00545523429515539,-0.0187196130472065,0.0437856215390418));
#44116=CARTESIAN_POINT('',(-0.00891300648284402,-0.0172399362322272,0.0436934413975258));
#44117=CARTESIAN_POINT('',(-0.0113573504197405,-0.0157376069342165,0.04362384288412));
#44118=CARTESIAN_POINT('',(-0.0135102835960664,-0.0139325421260677,0.0435535746462952));
#44119=CARTESIAN_POINT('',(-0.0154180093269257,-0.0117870438403986,0.0434824863656544));
#44120=CARTESIAN_POINT('',(-0.0169618356024676,-0.00943085053462302,0.0434142434361397));
#44121=CARTESIAN_POINT('',(-0.018561552248414,-0.00597807502936931,0.043319871863772));
#44122=CARTESIAN_POINT('',(-0.0193687071465493,-0.00227159356300758,0.0432271688042743));
#44123=CARTESIAN_POINT('',(-0.0193459881530204,0.00154443687141394,0.043134160214351));
#44124=CARTESIAN_POINT('',(-0.0189197212929505,0.0043234240436967,0.0430637334209306));
#44125=CARTESIAN_POINT('',(-0.018074362755791,0.00706858698254036,0.0429930115786603));
#44126=CARTESIAN_POINT('',(-0.0168625782586977,0.00960726235925872,0.0429248070362474));
#44127=CARTESIAN_POINT('',(-0.015268013302165,0.0119817090270433,0.0428536025858245));
#44128=CARTESIAN_POINT('',(-0.013360235232493,0.0140750748851165,0.0427834074356023));
#44129=CARTESIAN_POINT('',(-0.0111697667217031,0.0158720510310536,0.0427147000605931));
#44130=CARTESIAN_POINT('',(-0.00871620076132663,0.0173399062434923,0.0426443517707747));
#44131=CARTESIAN_POINT('',(-0.00611636466270319,0.0184183849806335,0.0425739346463595));
#44132=CARTESIAN_POINT('',(-0.0033321215578175,0.0191193135415984,0.042503638306099));
#44133=CARTESIAN_POINT('',(-0.000534719349594548,0.0194001567923326,0.0424352481242054));
#44134=CARTESIAN_POINT('',(0.00327849885131586,0.0192236784280454,0.0423397283567898));
#44135=CARTESIAN_POINT('',(0.00693693435561955,0.0182248427665248,0.0422486928840703));
#44136=CARTESIAN_POINT('',(0.0103015416551695,0.0164475884952921,0.0421545163322705));
#44137=CARTESIAN_POINT('',(0.0125743260223434,0.0147828414026713,0.0420842344442644));
#44138=CARTESIAN_POINT('',(0.0146175543522543,0.0127663093377594,0.0420143045368343));
#44139=CARTESIAN_POINT('',(0.0163078319804017,0.0105219606378753,0.0419455699872781));
#44140=CARTESIAN_POINT('',(0.0176804778117793,0.00800303522391728,0.0418737798000558));
#44141=CARTESIAN_POINT('',(0.0189788691155733,0.00447263254597852,0.0417818750029852));
#44142=CARTESIAN_POINT('',(0.0194877865696638,0.000664950319516681,0.0416882131489404));
#44143=CARTESIAN_POINT('',(0.0191606344240293,-0.00308452734371485,0.0415945646754112));
#44144=CARTESIAN_POINT('',(0.0184972150414569,-0.00587405614797688,0.0415249961850151));
#44145=CARTESIAN_POINT('',(0.0174551688991988,-0.00848356918159712,0.0414557067014046));
#44146=CARTESIAN_POINT('',(0.0160118984407478,-0.0109666655171155,0.0413840608453789));
#44147=CARTESIAN_POINT('',(0.0142568879553151,-0.0131671967630898,0.0413154608515628));
#44148=CARTESIAN_POINT('',(0.0114739992840907,-0.0157687954816694,0.0412225537492099));
#44149=CARTESIAN_POINT('',(0.00820510218136591,-0.0176905682270122,0.041127987405849));
#44150=CARTESIAN_POINT('',(0.00457500630677842,-0.0188604491142679,0.0410356755215267));
#44151=CARTESIAN_POINT('',(0.00180103482447101,-0.0193238643528813,0.0409657832532925));
#44152=CARTESIAN_POINT('',(-0.00107107012237494,-0.0193776995117875,0.0408944417055149));
#44153=CARTESIAN_POINT('',(-0.00385957609717241,-0.0190194680803449,0.0408261940093936));
#44154=CARTESIAN_POINT('',(-0.00661674975701956,-0.0182460217520095,0.0407559615376911));
#44155=CARTESIAN_POINT('',(-0.00919615117806423,-0.0170879464996363,0.0406851519599111));
#44156=CARTESIAN_POINT('',(-0.0115757360312258,-0.0155783764814346,0.0406160327672618));
#44157=CARTESIAN_POINT('',(-0.0144816228512718,-0.0130632680781061,0.0405226059839666));
#44158=CARTESIAN_POINT('',(-0.0167255080784181,-0.0100258204989716,0.0404284451556143));
#44159=CARTESIAN_POINT('',(-0.018273821340579,-0.00653624939613813,0.0403361064322415));
#44160=CARTESIAN_POINT('',(-0.0190266203226373,-0.00382735491088818,0.0402665472857832));
#44161=CARTESIAN_POINT('',(-0.0193826548713618,-0.000976776954179603,0.040194831061496));
#44162=CARTESIAN_POINT('',(-0.0193202269220419,0.00183427021572927,0.0401262202187513));
#44163=CARTESIAN_POINT('',(-0.0188410320331117,0.00465684276915032,0.04005635983472));
#44164=CARTESIAN_POINT('',(-0.0176721712985505,0.00824010010470064,0.0399619467409778));
#44165=CARTESIAN_POINT('',(-0.0157139906954545,0.0115444562535526,0.0398700712706307));
#44166=CARTESIAN_POINT('',(-0.0131404121963109,0.0142825387260622,0.0397766036249347));
#44167=CARTESIAN_POINT('',(-0.0108892506373088,0.0160641909999058,0.0397052086483859));
#44168=CARTESIAN_POINT('',(-0.00845490209584555,0.0174688971648347,0.0396369495862849));
#44169=CARTESIAN_POINT('',(-0.0057901959548591,0.0185240850474543,0.039566438989386));
#44170=CARTESIAN_POINT('',(-0.00304034502797974,0.0191668077438134,0.0394959407562146));
#44171=CARTESIAN_POINT('',(-0.000205901340496404,0.0194070054520654,0.0394264264215391));
#44172=CARTESIAN_POINT('',(0.00263699327955384,0.0192272254647594,0.0393571893618666));
#44173=CARTESIAN_POINT('',(0.00539600038814193,0.0186426594092554,0.0392866544513076));
#44174=CARTESIAN_POINT('',(0.00808505590971417,0.0176426432032035,0.0392157074108896));
#44175=CARTESIAN_POINT('',(0.0105483699747408,0.0162909067686871,0.0391476200440295));
#44176=CARTESIAN_POINT('',(0.0128356568770419,0.0145569551839711,0.0390764682392641));
#44177=CARTESIAN_POINT('',(0.0154667936342723,0.0118723552378021,0.0389830095045639));
#44178=CARTESIAN_POINT('',(0.0174959375379232,0.00861028352118488,0.0388910983122013));
#44179=CARTESIAN_POINT('',(0.018737560948652,0.00505469577241424,0.0387967510809749));
#44180=CARTESIAN_POINT('',(0.0192773093553197,0.00224064998029077,0.0387263243880055));
#44181=CARTESIAN_POINT('',(0.0193996109462872,-0.000567772972921872,0.038658090573959));
#44182=CARTESIAN_POINT('',(0.019103237189323,-0.00342339164913732,0.0385865907481668));
#44183=CARTESIAN_POINT('',(0.018406524551842,-0.0061503438852885,0.038516874656554));
#44184=CARTESIAN_POINT('',(0.0169361589213083,-0.00966858061701975,0.038424581031263));
#44185=CARTESIAN_POINT('',(0.0147454945400407,-0.0127612251195262,0.038330334371663));
#44186=CARTESIAN_POINT('',(0.0119167773275786,-0.0153174725086515,0.0382369783791112));
#44187=CARTESIAN_POINT('',(0.00957733860555868,-0.0168803266372561,0.0381685058222812));
#44188=CARTESIAN_POINT('',(0.00698077170066027,-0.0181084047715643,0.0380966845785145));
#44189=CARTESIAN_POINT('',(0.0042918767418205,-0.0189264882216141,0.0380274832798624));
#44190=CARTESIAN_POINT('',(0.00145824599298628,-0.0193532361924154,0.0379581524639087));
#44191=CARTESIAN_POINT('',(-0.00230745717185322,-0.0193620370982988,0.0378643768735323));
#44192=CARTESIAN_POINT('',(-0.00605875712442595,-0.0185332614335168,0.037770630359556));
#44193=CARTESIAN_POINT('',(-0.00946539676442699,-0.0169433041032279,0.0376786997789487));
#44194=CARTESIAN_POINT('',(-0.0118601315399094,-0.0153614098090379,0.0376069200646522));
#44195=CARTESIAN_POINT('',(-0.0139539673129934,-0.0134878988356932,0.0375381410572525));
#44196=CARTESIAN_POINT('',(-0.0157915027794027,-0.0112835406068729,0.0374685270222508));
#44197=CARTESIAN_POINT('',(-0.0172579230800856,-0.00887577363203918,0.0373980765841363));
#44198=CARTESIAN_POINT('',(-0.0183727133494431,-0.00625378905721084,0.0373274841689959));
#44199=CARTESIAN_POINT('',(-0.0190884840066312,-0.00350098448769894,0.0372584724349144));
#44200=CARTESIAN_POINT('',(-0.0193957163038253,-0.000694067135523436,0.0371887234296306));
#44201=CARTESIAN_POINT('',(-0.0192850410734145,0.00217035261908061,0.0371172799265481));
#44202=CARTESIAN_POINT('',(-0.0187701121534513,0.00493301967824674,0.0370488310019022));
#44203=CARTESIAN_POINT('',(-0.0178372483489486,0.00764932587964424,0.0369788065708886));
#44204=CARTESIAN_POINT('',(-0.0165419620384625,0.010147864520342,0.0369082891947026));
#44205=CARTESIAN_POINT('',(-0.0148734158890986,0.0124680415791245,0.036837870820931));
#44206=CARTESIAN_POINT('',(-0.0128973916193517,0.0145010968396696,0.0367691497387133));
#44207=CARTESIAN_POINT('',(-0.0106519271325968,0.0162238286040827,0.0366987385269726));
#44208=CARTESIAN_POINT('',(-0.00814949887436442,0.0176125565764292,0.0366277713925307));
#44209=CARTESIAN_POINT('',(-0.00551879983682063,0.0186067070341556,0.0365595624449246));
#44210=CARTESIAN_POINT('',(-0.00271205952795247,0.0192174753444305,0.0364889202888244));
#44211=CARTESIAN_POINT('',(9.33714311773742E-5,0.0194065080580889,0.0364185370033719));
#44212=CARTESIAN_POINT('',(0.00389771074671841,0.0191082063674791,0.03632547293438));
#44213=CARTESIAN_POINT('',(0.00752080983387477,0.0179919526508517,0.0362324801372786));
#44214=CARTESIAN_POINT('',(0.0108287899040495,0.0161047355207281,0.0361378634417124));
#44215=CARTESIAN_POINT('',(0.0123060494137679,0.0149474122876113,0.0360927078861263));
#44216=CARTESIAN_POINT('',(0.0130058841653258,0.0143115250488958,0.036069621110675));
#44217=CARTESIAN_POINT('',(0.0133472924810068,0.013834004568283,0.0361523595743667));
#44218=CARTESIAN_POINT('',(0.0133936849724094,0.0137807465598252,0.0361621806530942));
#44219=CARTESIAN_POINT('',(0.0134819277095383,0.0136809336166974,0.0361806693828696));
#44220=CARTESIAN_POINT('',(0.0136838792255527,0.0134680380101868,0.036221212408854));
#44221=CARTESIAN_POINT('',(0.0137247775534597,0.0134264423745443,0.0362290943081679));
#44222=CARTESIAN_POINT('',(0.0137371265537183,0.013413795666025,0.0362315327602123));
#44223=CARTESIAN_POINT('',(-0.0192,0.,0.0373616076561507));
#44224=CARTESIAN_POINT('',(-0.0192,0.000371890410119982,0.0373522525296843));
#44225=CARTESIAN_POINT('',(-0.0191785530500175,0.00116597240745298,0.0373323651099912));
#44226=CARTESIAN_POINT('',(-0.0190533790090975,0.00250459018190321,0.0372989507415849));
#44227=CARTESIAN_POINT('',(-0.0188473405126322,0.00373007741948374,0.0372682487486553));
#44228=CARTESIAN_POINT('',(-0.0186320455861301,0.00464879561353362,0.03724500860155));
#44229=CARTESIAN_POINT('',(-0.0184910260779751,0.00517577049788258,0.0372315910441466));
#44230=CARTESIAN_POINT('',(-0.0183631738799605,0.00561124864393773,0.0372204437696751));
#44231=CARTESIAN_POINT('',(-0.0182640831751387,0.00592442485168977,0.0372123708776225));
#44232=CARTESIAN_POINT('',(-0.0181114229288877,0.00638129356744456,0.0372005013632639));
#44233=CARTESIAN_POINT('',(-0.0178282980344812,0.00715369007655939,0.0371801655718353));
#44234=CARTESIAN_POINT('',(-0.0174532063649077,0.00802611439628738,0.0371565444398454));
#44235=CARTESIAN_POINT('',(-0.0170319137943417,0.00887256924934606,0.0371328574091274));
#44236=CARTESIAN_POINT('',(-0.0166916512615943,0.00949703934327355,0.0371149616027724));
#44237=CARTESIAN_POINT('',(-0.0163920316200393,0.0100022368165151,0.0371001174124457));
#44238=CARTESIAN_POINT('',(-0.0161668301297771,0.0103582788158399,0.037089432092816));
#44239=CARTESIAN_POINT('',(-0.0160442954394929,0.0105467961338315,0.0370837216066706));
#44240=CARTESIAN_POINT('',(-0.0159259339101793,0.0107243466139525,0.0370782923415417));
#44241=CARTESIAN_POINT('',(-0.015902121562517,0.0107593087439536,0.0370772214540573));
#44242=CARTESIAN_POINT('',(-0.0158246774181559,0.0108733496105961,0.0370737446787212));
#44243=CARTESIAN_POINT('',(-0.0156785114667725,0.0110844976801846,0.0370673156842167));
#44244=CARTESIAN_POINT('',(-0.0153807730333783,0.0114997536190571,0.0370546167892147));
#44245=CARTESIAN_POINT('',(-0.014962269035776,0.0120387684412869,0.0370377633163098));
#44246=CARTESIAN_POINT('',(-0.0145507291330991,0.0125303807447499,0.0370219676193401));
#44247=CARTESIAN_POINT('',(-0.0140566959530989,0.0130876736332664,0.0370036516599521));
#44248=CARTESIAN_POINT('',(-0.0134911078549613,0.0136706063886826,0.036983680328007));
#44249=CARTESIAN_POINT('',(-0.0130066880814553,0.0141265515432096,0.036967283585551));
#44250=CARTESIAN_POINT('',(-0.0126777438236585,0.0144203680610192,0.0369563905284894));
#44251=CARTESIAN_POINT('',(-0.0124597249647613,0.0146087978374249,0.0369492596498424));
#44252=CARTESIAN_POINT('',(-0.0123099397336204,0.0147348872989819,0.0369444033292919));
#44253=CARTESIAN_POINT('',(-0.0121944734692698,0.0148302309493534,0.0369406777873217));
#44254=CARTESIAN_POINT('',(-0.0121492528362333,0.0148675088863959,0.0369392176100781));
#44255=CARTESIAN_POINT('',(-0.0119863805608889,0.0149993545089899,0.036933984538422));
#44256=CARTESIAN_POINT('',(-0.0118085399796179,0.015139992071706,0.0369283182662103));
#44257=CARTESIAN_POINT('',(-0.0114746059451049,0.0153972690138823,0.0369177724023816));
#44258=CARTESIAN_POINT('',(-0.0109992219992465,0.0157425412407583,0.036903044451745));
#44259=CARTESIAN_POINT('',(-0.0105013973511648,0.0160764140150835,0.0368879731719335));
#44260=CARTESIAN_POINT('',(-0.0101104080215209,0.0163238952481856,0.0368763158121412));
#44261=CARTESIAN_POINT('',(-0.00977639198801372,0.0165255784868323,0.0368664640946302));
#44262=CARTESIAN_POINT('',(-0.00958104132157012,0.0166391770763527,0.036860770200424));
#44263=CARTESIAN_POINT('',(-0.00923219712027506,0.0168370294522573,0.0368507156214954));
#44264=CARTESIAN_POINT('',(-0.00856053323848537,0.0171961213283961,0.0368317271371337));
#44265=CARTESIAN_POINT('',(-0.00758934787306023,0.0176566860768508,0.0368051955704689));
#44266=CARTESIAN_POINT('',(-0.00636643819771057,0.0181219912186938,0.036772976891564));
#44267=CARTESIAN_POINT('',(-0.0052667098920806,0.0184781293286437,0.0367444452964538));
#44268=CARTESIAN_POINT('',(-0.00400582762844146,0.0187957254590059,0.0367122907087581));
#44269=CARTESIAN_POINT('',(-0.00294566296814909,0.0189789958608912,0.0366855418485812));
#44270=CARTESIAN_POINT('',(-0.00232318507258854,0.0190604019775968,0.0366698466292546));
#44271=CARTESIAN_POINT('',(-0.00198376779530057,0.0190975924642744,0.0366612799344118));
#44272=CARTESIAN_POINT('',(-0.00179049704812089,0.0191170012041065,0.0366563916149323));
#44273=CARTESIAN_POINT('',(-0.00144107189914202,0.0191469089045128,0.0366475609085875));
#44274=CARTESIAN_POINT('',(-0.00102086988890093,0.0191748137169543,0.0366369845716538));
#44275=CARTESIAN_POINT('',(-0.000242744702888557,0.0192077009052938,0.0366174751610461));
#44276=CARTESIAN_POINT('',(0.000903540972486138,0.0191964529250526,0.0365889325725422));
#44277=CARTESIAN_POINT('',(0.00236686630270527,0.0190724376044203,0.0365525815476574));
#44278=CARTESIAN_POINT('',(0.00360662279469994,0.0188721503870318,0.0365217257376382));
#44279=CARTESIAN_POINT('',(0.00469151749077868,0.0186237860444726,0.0364943675307728));
#44280=CARTESIAN_POINT('',(0.00540082376038474,0.0184290014337655,0.0364761561957));
#44281=CARTESIAN_POINT('',(0.00593364138090763,0.0182624425984035,0.036462249397394));
#44282=CARTESIAN_POINT('',(0.00633445502197581,0.0181256641700199,0.0364516317998972));
#44283=CARTESIAN_POINT('',(0.00658566662395393,0.0180361904684984,0.0364449143813257));
#44284=CARTESIAN_POINT('',(0.00694154913776284,0.0179025878526453,0.0364353138516747));
#44285=CARTESIAN_POINT('',(0.00737542446485554,0.0177295306256606,0.0364235218690459));
#44286=CARTESIAN_POINT('',(0.00792504129770683,0.0174929818445577,0.0364084143183134));
#44287=CARTESIAN_POINT('',(0.00845826749280384,0.017239460962699,0.0363935064609552));
#44288=CARTESIAN_POINT('',(0.00883222304449844,0.0170485828373795,0.0363829021210688));
#44289=CARTESIAN_POINT('',(0.00903653051859202,0.0169408952112956,0.0363770691222274));
#44290=CARTESIAN_POINT('',(0.00921086669198421,0.0168465991202952,0.0363720612873765));
#44291=CARTESIAN_POINT('',(0.00930080306136933,0.0167969846854805,0.0363694715142351));
#44292=CARTESIAN_POINT('',(0.00946017099694578,0.0167081137134898,0.0363648869257377));
#44293=CARTESIAN_POINT('',(0.00974470880582175,0.0165452759759724,0.0363566902289924));
#44294=CARTESIAN_POINT('',(0.010216916845427,0.0162610675113002,0.0363430146333954));
#44295=CARTESIAN_POINT('',(0.0108590295515736,0.0158416026951709,0.0363241211007571));
#44296=CARTESIAN_POINT('',(0.0115972342310281,0.0153116725285745,0.0363018822071081));
#44297=CARTESIAN_POINT('',(0.0123260419243019,0.0147294470622927,0.0362790852966174));
#44298=CARTESIAN_POINT('',(0.0130972614005013,0.0140534113101744,0.0362539467117431));
#44299=CARTESIAN_POINT('',(0.0135202801000095,0.0136359227301335,0.0362393193646486));
#44300=CARTESIAN_POINT('',(0.0137371532346411,0.0134138220134304,0.0362316338257453));
#44301=CARTESIAN_POINT('',(-0.0192,2.09607971128427E-14,0.0373616076561507));
#44302=CARTESIAN_POINT('',(0.0192,6.20369116582113E-17,0.0388620248355153));
#44303=CARTESIAN_POINT('',(0.0192,-0.000124988712080034,0.0388589418972036));
#44304=CARTESIAN_POINT('',(0.019197908568983,-0.000469951366362968,0.0388503776671778));
#44305=CARTESIAN_POINT('',(0.0191708854160062,-0.00113849276069121,0.0388336681086579));
#44306=CARTESIAN_POINT('',(0.0191167543307171,-0.00181358675664011,0.0388167129967166));
#44307=CARTESIAN_POINT('',(0.019053823567411,-0.00239064344730558,0.0388021651865298));
#44308=CARTESIAN_POINT('',(0.0189785332376671,-0.00292447550362445,0.0387886436902797));
#44309=CARTESIAN_POINT('',(0.0189087227591735,-0.0033350115235191,0.0387781924280792));
#44310=CARTESIAN_POINT('',(0.0188663906766718,-0.00356565828611578,0.0387723058742901));
#44311=CARTESIAN_POINT('',(0.018825097103103,-0.00377681105440297,0.0387669036693559));
#44312=CARTESIAN_POINT('',(0.0188077282469835,-0.00386153097423765,0.0387647329733464));
#44313=CARTESIAN_POINT('',(0.0187750316529949,-0.00401877614816724,0.0387607045053975));
#44314=CARTESIAN_POINT('',(0.0187193199572928,-0.00427374897108696,0.0387541660083545));
#44315=CARTESIAN_POINT('',(0.0186304266466907,-0.00464970563988405,0.0387445081722731));
#44316=CARTESIAN_POINT('',(0.0185129476878379,-0.00509733713455083,0.0387329720111096));
#44317=CARTESIAN_POINT('',(0.0183398599789788,-0.00569735566998535,0.0387174493033485));
#44318=CARTESIAN_POINT('',(0.0180945951276823,-0.00644494954433084,0.0386979707530031));
#44319=CARTESIAN_POINT('',(0.0177437299560687,-0.00735566619832176,0.038673968118737));
#44320=CARTESIAN_POINT('',(0.0173645091276954,-0.0082100275935466,0.0386509980338975));
#44321=CARTESIAN_POINT('',(0.0169395232115261,-0.00905492681459564,0.0386276443282059));
#44322=CARTESIAN_POINT('',(0.0164747060732539,-0.00987520965215876,0.0386042864124672));
#44323=CARTESIAN_POINT('',(0.0159698691930589,-0.0106724061933238,0.0385808228137399));
#44324=CARTESIAN_POINT('',(0.015426561638605,-0.0114436727128365,0.0385572800129853));
#44325=CARTESIAN_POINT('',(0.0149428266243687,-0.0120633797631095,0.0385375913015805));
#44326=CARTESIAN_POINT('',(0.01453781514937,-0.0125445541649258,0.0385217941673181));
#44327=CARTESIAN_POINT('',(0.0142776465840892,-0.0128387126614965,0.0385119130566294));
#44328=CARTESIAN_POINT('',(0.0140645984954196,-0.013070769057157,0.0385039754056187));
#44329=CARTESIAN_POINT('',(0.0139043962979387,-0.0132411426968139,0.0384980777448022));
#44330=CARTESIAN_POINT('',(0.013763723147588,-0.0133868564728369,0.0384929650586733));
#44331=CARTESIAN_POINT('',(0.013662313595645,-0.0134903048716543,0.0384893064291248));
#44332=CARTESIAN_POINT('',(0.0135525008274683,-0.013600476147292,0.0384853748174183));
#44333=CARTESIAN_POINT('',(0.0135690565436169,-0.0135838157902813,0.0384859700957141));
#44334=CARTESIAN_POINT('',(0.0135391866005673,-0.0136136572054972,0.0384849120327072));
#44335=CARTESIAN_POINT('',(0.0134917789484498,-0.0136607045306038,0.0384832550069352));
#44336=CARTESIAN_POINT('',(0.0133655542699404,-0.0137849389174932,0.0384788679632096));
#44337=CARTESIAN_POINT('',(0.0131407368446433,-0.0140001630606948,0.038471180294041));
#44338=CARTESIAN_POINT('',(0.0128329907468812,-0.0142838284621455,0.0384608522080179));
#44339=CARTESIAN_POINT('',(0.0124394944651753,-0.014629051704642,0.0384479439399829));
#44340=CARTESIAN_POINT('',(0.0120350384336053,-0.0149629409663656,0.0384350171155988));
#44341=CARTESIAN_POINT('',(0.0116630824288502,-0.0152531313620447,0.0384233910564852));
#44342=CARTESIAN_POINT('',(0.0113578002512048,-0.0154819406315971,0.038413990371784));
#44343=CARTESIAN_POINT('',(0.0110852017754261,-0.0156778700166862,0.0384057194634792));
#44344=CARTESIAN_POINT('',(0.0108757691840278,-0.0158229190119628,0.0383994431066811));
#44345=CARTESIAN_POINT('',(0.0107633978180121,-0.0158995337565912,0.0383960924847546));
#44346=CARTESIAN_POINT('',(0.010647220670249,-0.0159774670540609,0.0383926461721934));
#44347=CARTESIAN_POINT('',(0.010644680199581,-0.015979057777509,0.0383925721061032));
#44348=CARTESIAN_POINT('',(0.0106004017580862,-0.0160085336640853,0.0383912603424084));
#44349=CARTESIAN_POINT('',(0.0105388855056911,-0.0160491332519111,0.0383894399309875));
#44350=CARTESIAN_POINT('',(0.0104337580683584,-0.0161178495328419,0.0383863325780379));
#44351=CARTESIAN_POINT('',(0.0102995596447433,-0.0162039569082081,0.0383823779216498));
#44352=CARTESIAN_POINT('',(0.0101026409934458,-0.0163279400315075,0.0383765955804146));
#44353=CARTESIAN_POINT('',(0.00982569348738544,-0.0164971000054074,0.0383685125932213));
#44354=CARTESIAN_POINT('',(0.00931229706094346,-0.0167953943362142,0.0383536861129244));
#44355=CARTESIAN_POINT('',(0.00869623024698729,-0.0171259186584117,0.0383361879893404));
#44356=CARTESIAN_POINT('',(0.00804598232123238,-0.0174348214410755,0.0383181275958529));
#44357=CARTESIAN_POINT('',(0.00766192783303044,-0.0176062593109793,0.0383075679160363));
#44358=CARTESIAN_POINT('',(0.00731139699448762,-0.0177542581748895,0.0382980077197107));
#44359=CARTESIAN_POINT('',(0.00712765573843583,-0.0178283104509261,0.0382930327414598));
#44360=CARTESIAN_POINT('',(0.00682289565956123,-0.0179482076378896,0.0382848198753714));
#44361=CARTESIAN_POINT('',(0.00645992069858502,-0.0180825892927988,0.0382751348480656));
#44362=CARTESIAN_POINT('',(0.00601258557271775,-0.0182363346904473,0.0382633299572721));
#44363=CARTESIAN_POINT('',(0.00556480119192505,-0.0183778750104654,0.0382516426298377));
#44364=CARTESIAN_POINT('',(0.00511355445316589,-0.0185084972990694,0.038239983726734));
#44365=CARTESIAN_POINT('',(0.00466130310345707,-0.0186275784942477,0.0382284093826885));
#44366=CARTESIAN_POINT('',(0.00427933841460029,-0.0187180967791853,0.0382187217286313));
#44367=CARTESIAN_POINT('',(0.00401789245348191,-0.0187752281188422,0.0382121305187804));
#44368=CARTESIAN_POINT('',(0.00385789607829158,-0.0188084863297999,0.0382081100715769));
#44369=CARTESIAN_POINT('',(0.00376711328860128,-0.018827031731736,0.0382058321410011));
#44370=CARTESIAN_POINT('',(0.00356421552584282,-0.0188666354876692,0.0382007513506392));
#44371=CARTESIAN_POINT('',(0.00333905036475743,-0.0189079866307164,0.0381951232778063));
#44372=CARTESIAN_POINT('',(0.00293936341804117,-0.0189761002733566,0.0381851532080257));
#44373=CARTESIAN_POINT('',(0.00241653091500352,-0.0190504529133085,0.0381721596825934));
#44374=CARTESIAN_POINT('',(0.00184779993776262,-0.0191134168112792,0.0381580649595237));
#44375=CARTESIAN_POINT('',(0.00134438187706576,-0.0191548105265659,0.0381456055678352));
#44376=CARTESIAN_POINT('',(0.000905072994749517,-0.0191800757495629,0.038134731794586));
#44377=CARTESIAN_POINT('',(0.000532799307105026,-0.0191936389183209,0.0381255046676114));
#44378=CARTESIAN_POINT('',(0.00027220902580008,-0.0191983861193444,0.0381190256016955));
#44379=CARTESIAN_POINT('',(0.000128419938523944,-0.0191996842940641,0.0381154391115202));
#44380=CARTESIAN_POINT('',(3.90987858716185E-5,-0.0191999474181661,0.0381132046010067));
#44381=CARTESIAN_POINT('',(1.95431978264071E-5,-0.0192001150269539,0.0381127151714058));
#44382=CARTESIAN_POINT('',(-0.000161500855682608,-0.0191995839834403,0.0381081740006597));
#44383=CARTESIAN_POINT('',(-0.000344994553467409,-0.0191972462183798,0.038103572552286));
#44384=CARTESIAN_POINT('',(-0.000689203714121839,-0.019189417004198,0.0380949412020279));
#44385=CARTESIAN_POINT('',(-0.00115754456909656,-0.0191677379106035,0.0380831957121736));
#44386=CARTESIAN_POINT('',(-0.00170968846669982,-0.0191263395125739,0.0380693347309524));
#44387=CARTESIAN_POINT('',(-0.00242229227603454,-0.0190523549997508,0.0380514148760769));
#44388=CARTESIAN_POINT('',(-0.00327277835673546,-0.0189278245373745,0.0380299489735858));
#44389=CARTESIAN_POINT('',(-0.00454268577104214,-0.0186737472496771,0.0379976696929144));
#44390=CARTESIAN_POINT('',(-0.00568050934246028,-0.0183541258273889,0.0379683371672561));
#44391=CARTESIAN_POINT('',(-0.0066719009761423,-0.0180092154984539,0.0379423639538944));
#44392=CARTESIAN_POINT('',(-0.00726202656726792,-0.0177759556110926,0.0379267344521425));
#44393=CARTESIAN_POINT('',(-0.00764324733329641,-0.0176141181512875,0.037916525073436));
#44394=CARTESIAN_POINT('',(-0.00809920545239486,-0.0174115610264153,0.0379041591448252));
#44395=CARTESIAN_POINT('',(-0.00874479716386492,-0.0171013740913796,0.0378863251899204));
#44396=CARTESIAN_POINT('',(-0.00949423536320096,-0.0166957978671014,0.0378650102089074));
#44397=CARTESIAN_POINT('',(-0.0100722264432436,-0.016347902852265,0.0378480854348865));
#44398=CARTESIAN_POINT('',(-0.0104051711420505,-0.0161371977584436,0.037838189497368));
#44399=CARTESIAN_POINT('',(-0.0106884929050717,-0.0159506554757344,0.0378296616784728));
#44400=CARTESIAN_POINT('',(-0.0108714091101842,-0.0158261890624888,0.0378241013526368));
#44401=CARTESIAN_POINT('',(-0.0111453733805073,-0.015635575467968,0.0378157253933416));
#44402=CARTESIAN_POINT('',(-0.0115986568668551,-0.0153064203204682,0.0378016947061641));
#44403=CARTESIAN_POINT('',(-0.0120998520795891,-0.0149133113635874,0.0377858059068655));
#44404=CARTESIAN_POINT('',(-0.0125756135298173,-0.014510852707208,0.0377703222271541));
#44405=CARTESIAN_POINT('',(-0.0129200908078643,-0.0142050469318278,0.0377589086192492));
#44406=CARTESIAN_POINT('',(-0.0132006411545733,-0.0139434429700079,0.0377494317412391));
#44407=CARTESIAN_POINT('',(-0.0133857111418757,-0.013765000810918,0.0377430936558732));
#44408=CARTESIAN_POINT('',(-0.0134998711245461,-0.0136526570365928,0.0377391496876206));
#44409=CARTESIAN_POINT('',(-0.0135570653366891,-0.0135961534484681,0.0377371713818215));
#44410=CARTESIAN_POINT('',(-0.0137194782686012,-0.0134325193052724,0.0377315005296542));
#44411=CARTESIAN_POINT('',(-0.013890846647042,-0.0132555097358427,0.0377254395139226));
#44412=CARTESIAN_POINT('',(-0.0141914410618802,-0.0129364066458154,0.0377146534601655));
#44413=CARTESIAN_POINT('',(-0.0145641887987515,-0.012516248297343,0.037700830463428));
#44414=CARTESIAN_POINT('',(-0.0149458174721339,-0.0120567748443482,0.0376861206343685));
#44415=CARTESIAN_POINT('',(-0.0152621379397411,-0.0116525098886725,0.0376734681880677));
#44416=CARTESIAN_POINT('',(-0.015519755577611,-0.0113060729252389,0.0376628139369461));
#44417=CARTESIAN_POINT('',(-0.0157216407675846,-0.0110227938931655,0.0376542150155887));
#44418=CARTESIAN_POINT('',(-0.0158495685055665,-0.0108369321344913,0.0376486208969609));
#44419=CARTESIAN_POINT('',(-0.0159131669067378,-0.0107430778913541,0.0376458014971848));
#44420=CARTESIAN_POINT('',(-0.0159509485593324,-0.0106867591251374,0.0376441090112356));
#44421=CARTESIAN_POINT('',(-0.0159555729316056,-0.0106800156854144,0.0376439054569211));
#44422=CARTESIAN_POINT('',(-0.0160366912572767,-0.0105579889100657,0.0376402359555261));
#44423=CARTESIAN_POINT('',(-0.0161171589222373,-0.0104348325909768,0.0376365510641637));
#44424=CARTESIAN_POINT('',(-0.016268398071352,-0.0101992684367464,0.037629536890784));
#44425=CARTESIAN_POINT('',(-0.0164718347676829,-0.00986866479784329,0.0376198039485842));
#44426=CARTESIAN_POINT('',(-0.0167088982025017,-0.00946187138190906,0.037607987549141));
#44427=CARTESIAN_POINT('',(-0.0169352425124742,-0.00905045159144459,0.0375961914250413));
#44428=CARTESIAN_POINT('',(-0.0171515224314667,-0.00863362799674667,0.0375843835572777));
#44429=CARTESIAN_POINT('',(-0.0173579642690949,-0.00821054566971484,0.0375725348777327));
#44430=CARTESIAN_POINT('',(-0.017519853357746,-0.00785750697306154,0.0375627505445255));
#44431=CARTESIAN_POINT('',(-0.0176315159093588,-0.0076012047946677,0.0375557017408629));
#44432=CARTESIAN_POINT('',(-0.0176894144861573,-0.00746532669201923,0.0375519767883745));
#44433=CARTESIAN_POINT('',(-0.0177451023052229,-0.00733173837843177,0.0375483250161489));
#44434=CARTESIAN_POINT('',(-0.0177507176499454,-0.00731790430173732,0.037547949788258));
#44435=CARTESIAN_POINT('',(-0.0177786056944096,-0.00725011263857024,0.0375461082256053));
#44436=CARTESIAN_POINT('',(-0.0178249505298768,-0.00713585437300043,0.037543024456147));
#44437=CARTESIAN_POINT('',(-0.017911869168981,-0.00691657760835478,0.0375371512036404));
#44438=CARTESIAN_POINT('',(-0.0180372299084404,-0.00658405541648223,0.0375283410975867));
#44439=CARTESIAN_POINT('',(-0.0181819996122516,-0.00617484022070445,0.0375176079482784));
#44440=CARTESIAN_POINT('',(-0.0183404129537489,-0.00568953373275272,0.0375050087314909));
#44441=CARTESIAN_POINT('',(-0.0185070965992825,-0.00512393103192481,0.0374904763843311));
#44442=CARTESIAN_POINT('',(-0.0186457068520012,-0.00459147257359349,0.0374769312162186));
#44443=CARTESIAN_POINT('',(-0.018741723435775,-0.00417253373587205,0.0374663558945341));
#44444=CARTESIAN_POINT('',(-0.0187919046418404,-0.00393965552253266,0.0374604956552035));
#44445=CARTESIAN_POINT('',(-0.0188378277371704,-0.00371279381327267,0.0374548032660863));
#44446=CARTESIAN_POINT('',(-0.0188477741035621,-0.00366081165764643,0.0374535007869088));
#44447=CARTESIAN_POINT('',(-0.0188734250289746,-0.00352750121917844,0.037450156909658));
#44448=CARTESIAN_POINT('',(-0.0189120412610658,-0.00331666349387629,0.0374448677960544));
#44449=CARTESIAN_POINT('',(-0.0189684945740984,-0.00298253617925169,0.0374364833505349));
#44450=CARTESIAN_POINT('',(-0.0190303728155349,-0.0025592179366185,0.037425860538847));
#44451=CARTESIAN_POINT('',(-0.0191047485512526,-0.00195409312532511,0.0374106767231135));
#44452=CARTESIAN_POINT('',(-0.0191765387773259,-0.00112634873242808,0.0373899094755316));
#44453=CARTESIAN_POINT('',(-0.0192,-0.000387773697818323,0.037371362336252));
#44454=CARTESIAN_POINT('',(-0.0192,8.05624845824862E-17,0.0373616076561507));
#44455=CARTESIAN_POINT('',(0.0192,1.96007229986627E-17,0.0388620248355153));
#44456=CARTESIAN_POINT('',(-0.0192,0.,0.0403612589235446));
#44457=CARTESIAN_POINT('',(-0.0192,0.00251327412287183,0.0402987908365434));
#44458=CARTESIAN_POINT('',(-0.0182002919343753,0.00753865073535337,0.040173854662541));
#44459=CARTESIAN_POINT('',(-0.0139299003749868,0.0139299426504137,0.0399864504015373));
#44460=CARTESIAN_POINT('',(-0.00753880775836791,0.0182002798556818,0.0397990461405336));
#44461=CARTESIAN_POINT('',(-3.10273503482896E-17,0.0196998600721591,0.03961164187953));
#44462=CARTESIAN_POINT('',(0.00753880775836785,0.0182002798556819,0.0394242376185263));
#44463=CARTESIAN_POINT('',(0.0139299003749868,0.0139299426504138,0.0392368333575227));
#44464=CARTESIAN_POINT('',(0.0182002919343752,0.00753865073535343,0.039049429096519));
#44465=CARTESIAN_POINT('',(0.0192,0.00251327412287189,0.0389244929225166));
#44466=CARTESIAN_POINT('',(0.0192,6.20369116582113E-17,0.0388620248355153));
#44467=CARTESIAN_POINT('',(-0.0192,-1.4501171666592E-17,0.0403612589235446));
#44468=CARTESIAN_POINT('',(0.0192,-4.02812422912431E-17,0.0418617389925214));
#44469=CARTESIAN_POINT('',(0.0192,-0.000627843242455304,0.0418459149896042));
#44470=CARTESIAN_POINT('',(0.0191537643301771,-0.00156960588184851,0.0418222692764327));
#44471=CARTESIAN_POINT('',(0.0190001188250343,-0.00281623939187291,0.0417909221529283));
#44472=CARTESIAN_POINT('',(0.01883918794397,-0.00374443486002948,0.0417675022340309));
#44473=CARTESIAN_POINT('',(0.0186329305165787,-0.00466364444896726,0.041744172032056));
#44474=CARTESIAN_POINT('',(0.0184237261443943,-0.00542023794619651,0.0417248071699552));
#44475=CARTESIAN_POINT('',(0.0182341939543165,-0.00601895963697044,0.041709356516343));
#44476=CARTESIAN_POINT('',(0.0181067373193245,-0.00638980793763761,0.0416997275496235));
#44477=CARTESIAN_POINT('',(0.0179990141098919,-0.00668531233952582,0.0416920153142986));
#44478=CARTESIAN_POINT('',(0.017916392612426,-0.00690382795499897,0.0416862924890993));
#44479=CARTESIAN_POINT('',(0.0178425052565168,-0.00709176327290445,0.0416813509509974));
#44480=CARTESIAN_POINT('',(0.0177883148431507,-0.00722653945516051,0.0416777980127546));
#44481=CARTESIAN_POINT('',(0.0177298981413602,-0.00736843643407748,0.0416740486377474));
#44482=CARTESIAN_POINT('',(0.0177361056959902,-0.00735322856386581,0.0416744462653413));
#44483=CARTESIAN_POINT('',(0.0177135634101485,-0.00740754993225115,0.0416729888207892));
#44484=CARTESIAN_POINT('',(0.0176680143708629,-0.00751609556693613,0.041670043125588));
#44485=CARTESIAN_POINT('',(0.0175448062254457,-0.00780316456919125,0.041662210094693));
#44486=CARTESIAN_POINT('',(0.017348210981071,-0.00823261039592076,0.0416503418793174));
#44487=CARTESIAN_POINT('',(0.0171581507082923,-0.00861763583287296,0.0416395442179049));
#44488=CARTESIAN_POINT('',(0.0170408569778842,-0.00884688509719389,0.041633066860205));
#44489=CARTESIAN_POINT('',(0.016927301857711,-0.00906191411808112,0.0416269489218333));
#44490=CARTESIAN_POINT('',(0.0168732845432318,-0.00916165575196913,0.0416240955502257));
#44491=CARTESIAN_POINT('',(0.0167812975926273,-0.00932980027693052,0.0416192760630031));
#44492=CARTESIAN_POINT('',(0.016631988134669,-0.00959517286625485,0.0416116243936469));
#44493=CARTESIAN_POINT('',(0.0164193261483387,-0.00995586530857537,0.0416011166646698));
#44494=CARTESIAN_POINT('',(0.0161847624984565,-0.0103324864458127,0.0415900052069004));
#44495=CARTESIAN_POINT('',(0.0159498587768442,-0.0106902384024307,0.0415793156198152));
#44496=CARTESIAN_POINT('',(0.015796244316713,-0.0109155198260444,0.041572531035281));
#44497=CARTESIAN_POINT('',(0.0155129752010751,-0.0113183676381549,0.0415603119633324));
#44498=CARTESIAN_POINT('',(0.0150924641525449,-0.0118804942876301,0.0415429661108013));
#44499=CARTESIAN_POINT('',(0.0145440817653639,-0.0125441050815185,0.041521767807207));
#44500=CARTESIAN_POINT('',(0.0140915599306013,-0.0130438517449637,0.0415051948603972));
#44501=CARTESIAN_POINT('',(0.0138418101853328,-0.0133064327326426,0.0414962928479585));
#44502=CARTESIAN_POINT('',(0.0137000435118975,-0.0134521125954502,0.0414913009244137));
#44503=CARTESIAN_POINT('',(0.0135721568664822,-0.01358097893778,0.0414868440266645));
#44504=CARTESIAN_POINT('',(0.0135127579654517,-0.0136399226716658,0.0414847888114123));
#44505=CARTESIAN_POINT('',(0.0134079418667648,-0.013743266022233,0.0414811698358558));
#44506=CARTESIAN_POINT('',(0.0132321544619379,-0.0139134442118671,0.0414751447406687));
#44507=CARTESIAN_POINT('',(0.0128578074911663,-0.0142643394281208,0.0414624736336486));
#44508=CARTESIAN_POINT('',(0.0122839075380286,-0.0147662800087533,0.0414435430200608));
#44509=CARTESIAN_POINT('',(0.0115197718166145,-0.0153709239660496,0.0414192000206712));
#44510=CARTESIAN_POINT('',(0.0106812149772433,-0.0159668181269291,0.0413933220512161));
#44511=CARTESIAN_POINT('',(0.00975690466001372,-0.0165472060690147,0.0413658437512961));
#44512=CARTESIAN_POINT('',(0.00890441110781952,-0.0170185858158063,0.0413414504706516));
#44513=CARTESIAN_POINT('',(0.00823467043365877,-0.0173488409284886,0.0413228317413075));
#44514=CARTESIAN_POINT('',(0.00771530984471599,-0.0175829815851227,0.0413086879133658));
#44515=CARTESIAN_POINT('',(0.00737764376545773,-0.0177277551035595,0.0412995976301186));
#44516=CARTESIAN_POINT('',(0.00691403151053966,-0.0179142109294009,0.0412872590562853));
#44517=CARTESIAN_POINT('',(0.00633275608651757,-0.0181300937591548,0.0412719520498979));
#44518=CARTESIAN_POINT('',(0.00558179665843677,-0.0183789366066925,0.0412524444884101));
#44519=CARTESIAN_POINT('',(0.00467350144335485,-0.0186304502234844,0.0412292194259067));
#44520=CARTESIAN_POINT('',(0.00375189364860263,-0.0188377440194866,0.0412059982606157));
#44521=CARTESIAN_POINT('',(0.00282298528495288,-0.0189991349645822,0.041182719351927));
#44522=CARTESIAN_POINT('',(0.0020426204353073,-0.0190955533563667,0.0411630849459833));
#44523=CARTESIAN_POINT('',(0.00141662338007611,-0.0191496192573831,0.0411472834710634));
#44524=CARTESIAN_POINT('',(0.00094492328585047,-0.0191786222294659,0.0411353397205267));
#44525=CARTESIAN_POINT('',(0.00055562148532413,-0.0191931629113999,0.0411254480643244));
#44526=CARTESIAN_POINT('',(0.000274635500326976,-0.019198259287767,0.0411182849436181));
#44527=CARTESIAN_POINT('',(0.0001270905012555,-0.019199752920174,0.0411145184785584));
#44528=CARTESIAN_POINT('',(-2.02964970173482E-5,-0.0192000691117518,0.0411107494338678));
#44529=CARTESIAN_POINT('',(-2.73070643263094E-5,-0.0191999691316681,0.0411105723125384));
#44530=CARTESIAN_POINT('',(-9.42927973934236E-5,-0.0191998346321775,0.0411088723275784));
#44531=CARTESIAN_POINT('',(-0.000205969520278353,-0.0191990996183042,0.0411060611825788));
#44532=CARTESIAN_POINT('',(-0.000518280221740988,-0.0191947419058968,0.0410982542710774));
#44533=CARTESIAN_POINT('',(-0.00103309894591407,-0.0191768017109537,0.0410854977049571));
#44534=CARTESIAN_POINT('',(-0.00171336636587479,-0.0191260939133093,0.0410686752816012));
#44535=CARTESIAN_POINT('',(-0.00230543730467123,-0.0190645268048041,0.0410540247051728));
#44536=CARTESIAN_POINT('',(-0.00286067294098488,-0.0189885112329839,0.0410402526882767));
#44537=CARTESIAN_POINT('',(-0.00329193554404226,-0.0189163249776132,0.0410295156066571));
#44538=CARTESIAN_POINT('',(-0.0035342242342768,-0.0188723538347853,0.0410234708837452));
#44539=CARTESIAN_POINT('',(-0.00375910804039232,-0.0188286630706858,0.0410178493118795));
#44540=CARTESIAN_POINT('',(-0.00384162655933352,-0.0188117972953263,0.0410157817445844));
#44541=CARTESIAN_POINT('',(-0.00400143706818024,-0.018778748732123,0.0410117720926416));
#44542=CARTESIAN_POINT('',(-0.00425819699640189,-0.0187228728404288,0.0410053066525806));
#44543=CARTESIAN_POINT('',(-0.00463771989515113,-0.0186334494088187,0.0409956885112588));
#44544=CARTESIAN_POINT('',(-0.00508851127973717,-0.0185153993939838,0.040984153418488));
#44545=CARTESIAN_POINT('',(-0.00569224122452594,-0.0183415009407844,0.0409685468614956));
#44546=CARTESIAN_POINT('',(-0.00644300606195459,-0.018095346477159,0.0409488352351614));
#44547=CARTESIAN_POINT('',(-0.00735583170749214,-0.0177436664305437,0.0409242354126093));
#44548=CARTESIAN_POINT('',(-0.00820912160318066,-0.0173649177393381,0.0409007285815477));
#44549=CARTESIAN_POINT('',(-0.0090538279450822,-0.01694010742605,0.040877039843528));
#44550=CARTESIAN_POINT('',(-0.00987370713245694,-0.016475597121502,0.0408535109429379));
#44551=CARTESIAN_POINT('',(-0.0106706046380784,-0.0159710614231159,0.0408300498006754));
#44552=CARTESIAN_POINT('',(-0.0114415208803768,-0.0154281587004333,0.0408066829887606));
#44553=CARTESIAN_POINT('',(-0.0120611630247417,-0.0149445875513516,0.0407872774133061));
#44554=CARTESIAN_POINT('',(-0.0125418597742535,-0.0145401658432658,0.0407718081455736));
#44555=CARTESIAN_POINT('',(-0.0128957072007173,-0.014227200367128,0.0407601975066044));
#44556=CARTESIAN_POINT('',(-0.0131812984549019,-0.0139620693089218,0.0407506373546599));
#44557=CARTESIAN_POINT('',(-0.0133832261727362,-0.013767278863127,0.0407437641941292));
#44558=CARTESIAN_POINT('',(-0.0134890079980719,-0.0136635724747964,0.0407401370570444));
#44559=CARTESIAN_POINT('',(-0.0135920490877858,-0.013560945588807,0.0407365795937386));
#44560=CARTESIAN_POINT('',(-0.0136020244899235,-0.0135508187127998,0.0407362285870597));
#44561=CARTESIAN_POINT('',(-0.0136593695095193,-0.0134931587835208,0.0407342215620005));
#44562=CARTESIAN_POINT('',(-0.0137674260651111,-0.0133833208258739,0.0407303919271764));
#44563=CARTESIAN_POINT('',(-0.013996397043834,-0.0131459926664997,0.040722152941196));
#44564=CARTESIAN_POINT('',(-0.0143081322534517,-0.0128059126383152,0.040710578123726));
#44565=CARTESIAN_POINT('',(-0.014597060811328,-0.0124744910247934,0.0406995286431268));
#44566=CARTESIAN_POINT('',(-0.0149345701175886,-0.0120710784827756,0.0406862962487426));
#44567=CARTESIAN_POINT('',(-0.0152524455295557,-0.0116664523525784,0.0406733520355922));
#44568=CARTESIAN_POINT('',(-0.0155706647652202,-0.0112369780874827,0.0406599171117849));
#44569=CARTESIAN_POINT('',(-0.0157645283850144,-0.0109610542320634,0.0406514507041408));
#44570=CARTESIAN_POINT('',(-0.0158919455376738,-0.0107745665543249,0.0406457889478978));
#44571=CARTESIAN_POINT('',(-0.0159519309316406,-0.0106856931805736,0.0406431040826272));
#44572=CARTESIAN_POINT('',(-0.0160654338153441,-0.0105145670838618,0.0406379731773375));
#44573=CARTESIAN_POINT('',(-0.0162016770731501,-0.010304023853768,0.0406317192796287));
#44574=CARTESIAN_POINT('',(-0.0164552144854539,-0.0098995951624851,0.0406198432844194));
#44575=CARTESIAN_POINT('',(-0.0168277519493567,-0.00926111915807136,0.0406015336613028));
#44576=CARTESIAN_POINT('',(-0.0172135131107076,-0.00851708721611685,0.0405808712722396));
#44577=CARTESIAN_POINT('',(-0.0175135330475122,-0.00787589007472945,0.0405634606948363));
#44578=CARTESIAN_POINT('',(-0.0177503849735952,-0.00732539050718729,0.0405487545920869));
#44579=CARTESIAN_POINT('',(-0.017922722387128,-0.00689108231165104,0.040537280282719));
#44580=CARTESIAN_POINT('',(-0.0181511767555939,-0.00627423918175756,0.040521067440932));
#44581=CARTESIAN_POINT('',(-0.0183961393016278,-0.00552402500539296,0.0405015295443943));
#44582=CARTESIAN_POINT('',(-0.0186009225445446,-0.00477507780306626,0.0404821756477855));
#44583=CARTESIAN_POINT('',(-0.0187209541078721,-0.00426730281736034,0.0404690999049196));
#44584=CARTESIAN_POINT('',(-0.0187862510926728,-0.00396592695886857,0.0404613500609706));
#44585=CARTESIAN_POINT('',(-0.0188251795061491,-0.00377850956076864,0.0404565299607827));
#44586=CARTESIAN_POINT('',(-0.0188886225474197,-0.00344903140273257,0.040448075166883));
#44587=CARTESIAN_POINT('',(-0.0189541146207765,-0.00307263170116469,0.0404384569554945));
#44588=CARTESIAN_POINT('',(-0.0190535010784377,-0.00241795211744246,0.0404218022349424));
#44589=CARTESIAN_POINT('',(-0.019142591264807,-0.00157900478061102,0.0404006391407023));
#44590=CARTESIAN_POINT('',(-0.0191926184988158,-0.000705848102638887,0.040378783110985));
#44591=CARTESIAN_POINT('',(-0.0192,-0.000219444370327988,0.0403666935404272));
#44592=CARTESIAN_POINT('',(-0.0192,8.05624845824862E-17,0.0403612589235446));
#44593=CARTESIAN_POINT('',(0.0192,-1.29239240960012E-18,0.0418617389925214));
#44594=CARTESIAN_POINT('',(-0.0192,0.,0.0433622164621474));
#44595=CARTESIAN_POINT('',(-0.0192,0.000147507211797211,0.043358580368065));
#44596=CARTESIAN_POINT('',(-0.0191968671072525,0.000525458418521057,0.0433492025507995));
#44597=CARTESIAN_POINT('',(-0.0191667659187235,0.00120492352254042,0.0433322092910609));
#44598=CARTESIAN_POINT('',(-0.0191111396477066,0.00187068354310731,0.0433154645381049));
#44599=CARTESIAN_POINT('',(-0.0190484499763511,0.00243151124645706,0.0433012997814833));
#44600=CARTESIAN_POINT('',(-0.0189751065261789,0.00294512260095273,0.0432882627843026));
#44601=CARTESIAN_POINT('',(-0.0189084433553087,0.00333635026762873,0.0432782816926402));
#44602=CARTESIAN_POINT('',(-0.018867967792637,0.00355705390119569,0.0432726367653853));
#44603=CARTESIAN_POINT('',(-0.0188296083107075,0.00375417659207935,0.0432675830486295));
#44604=CARTESIAN_POINT('',(-0.0188106259416012,0.00384747730435347,0.0432651876727724));
#44605=CARTESIAN_POINT('',(-0.0187773583892012,0.00400792394336318,0.0432610681996519));
#44606=CARTESIAN_POINT('',(-0.0187199017558882,0.00427152271885334,0.0432542932527772));
#44607=CARTESIAN_POINT('',(-0.0185927099205175,0.00480905822935209,0.0432404507442756));
#44608=CARTESIAN_POINT('',(-0.0183836195261831,0.00556575431155928,0.0432208669820836));
#44609=CARTESIAN_POINT('',(-0.0180873089804619,0.0064646645018153,0.0431973794975082));
#44610=CARTESIAN_POINT('',(-0.0177442040660365,0.00735402961973002,0.0431738834876022));
#44611=CARTESIAN_POINT('',(-0.0173632993142133,0.00821279140121295,0.0431507581437783));
#44612=CARTESIAN_POINT('',(-0.0169392847532721,0.00905524136579888,0.043127446598598));
#44613=CARTESIAN_POINT('',(-0.0164748479127218,0.00987497000160888,0.0431040980083793));
#44614=CARTESIAN_POINT('',(-0.0159706659023455,0.0106711723912282,0.0430806726152886));
#44615=CARTESIAN_POINT('',(-0.0154280486374394,0.0114416409274727,0.0430571802943427));
#44616=CARTESIAN_POINT('',(-0.0149449728707957,0.0120607045846526,0.0430375478018137));
#44617=CARTESIAN_POINT('',(-0.014540513942163,0.0125414184154737,0.0430218030197048));
#44618=CARTESIAN_POINT('',(-0.0142807307678563,0.0128352797598789,0.0430119587851853));
#44619=CARTESIAN_POINT('',(-0.0140679438908703,0.0130671648106762,0.043004050686227));
#44620=CARTESIAN_POINT('',(-0.0139080950559403,0.0132372608859938,0.0429981814449215));
#44621=CARTESIAN_POINT('',(-0.0137672328849502,0.0133832378360116,0.0429930765146623));
#44622=CARTESIAN_POINT('',(-0.0136667665316002,0.0134857999722318,0.0429894621544974));
#44623=CARTESIAN_POINT('',(-0.0135546774144437,0.0135983119843254,0.0429854613326154));
#44624=CARTESIAN_POINT('',(-0.0135803507422782,0.0135725269208031,0.0429863795009893));
#44625=CARTESIAN_POINT('',(-0.0135579609249865,0.0135949436866065,0.042985589934664));
#44626=CARTESIAN_POINT('',(-0.0135241260074496,0.0136286319576716,0.0429844163957469));
#44627=CARTESIAN_POINT('',(-0.0134122684980384,0.0137393669158131,0.0429805353181473));
#44628=CARTESIAN_POINT('',(-0.0131987708866369,0.013945378430781,0.0429732294322348));
#44629=CARTESIAN_POINT('',(-0.0128957040977496,0.014227232826039,0.0429630389328064));
#44630=CARTESIAN_POINT('',(-0.0124999931542044,0.0145775187949328,0.0429500291460551));
#44631=CARTESIAN_POINT('',(-0.0120874028980407,0.0149208543561088,0.0429368171809524));
#44632=CARTESIAN_POINT('',(-0.0117047957792533,0.0152212463926557,0.0429248432281859));
#44633=CARTESIAN_POINT('',(-0.0113893116609989,0.0154588971641096,0.0429151208160326));
#44634=CARTESIAN_POINT('',(-0.011106377823381,0.015662973841106,0.0429065341368306));
#44635=CARTESIAN_POINT('',(-0.0108884901785639,0.0158141883601005,0.0429000058007099));
#44636=CARTESIAN_POINT('',(-0.0107712324571543,0.0158942424996833,0.0428965109700417));
#44637=CARTESIAN_POINT('',(-0.0106505171116694,0.0159752774569547,0.0428929322227892));
#44638=CARTESIAN_POINT('',(-0.0106460205250655,0.0159781642821721,0.042892800425013));
#44639=CARTESIAN_POINT('',(-0.0105983640035796,0.0160098901889975,0.0428913896894949));
#44640=CARTESIAN_POINT('',(-0.0105316156086848,0.0160539203188257,0.04288941627459));
#44641=CARTESIAN_POINT('',(-0.0104195822931692,0.0161270482431749,0.0428861083490502));
#44642=CARTESIAN_POINT('',(-0.0102784486791453,0.0162173812691568,0.0428819542411143));
#44643=CARTESIAN_POINT('',(-0.0100739574925949,0.0163457058768856,0.0428759566447638));
#44644=CARTESIAN_POINT('',(-0.00979076681366074,0.0165178911957962,0.0428677007940556));
#44645=CARTESIAN_POINT('',(-0.00927468092065322,0.0168162097782484,0.0428528076913747));
#44646=CARTESIAN_POINT('',(-0.00866625429603682,0.0171406412178905,0.0428355294012159));
#44647=CARTESIAN_POINT('',(-0.00803551042611735,0.0174395582385297,0.0428179883621527));
#44648=CARTESIAN_POINT('',(-0.00766259866638816,0.0176058407656829,0.042807716932329));
#44649=CARTESIAN_POINT('',(-0.0073310592070669,0.0177461135495836,0.0427986527046041));
#44650=CARTESIAN_POINT('',(-0.00713356770854759,0.0178260102771758,0.042793290591069));
#44651=CARTESIAN_POINT('',(-0.0068231221615849,0.0179481502777101,0.042784905775808));
#44652=CARTESIAN_POINT('',(-0.00630114392385532,0.0181413482143627,0.042770945861394));
#44653=CARTESIAN_POINT('',(-0.00569487666756819,0.0183407643472124,0.0427550049086278));
#44654=CARTESIAN_POINT('',(-0.00509246246604135,0.0185142887079103,0.0427394087070486));
#44655=CARTESIAN_POINT('',(-0.00464231757800164,0.0186322966851656,0.0427278639663815));
#44656=CARTESIAN_POINT('',(-0.00426436225872812,0.0187214681324995,0.0427182582784477));
#44657=CARTESIAN_POINT('',(-0.00400818107344625,0.0187773012896955,0.0427117862363903));
#44658=CARTESIAN_POINT('',(-0.00384992820223385,0.0188101057953246,0.042707801538979));
#44659=CARTESIAN_POINT('',(-0.00376537048733135,0.0188273945620611,0.0427056751899009));
#44660=CARTESIAN_POINT('',(-0.00355088111217657,0.0188691891749171,0.0427002933345339));
#44661=CARTESIAN_POINT('',(-0.00331734099086169,0.0189118443746048,0.0426944453268529));
#44662=CARTESIAN_POINT('',(-0.00290184491701416,0.0189820651534296,0.0426840636256509));
#44663=CARTESIAN_POINT('',(-0.00236329931331893,0.0190572768250712,0.0426706619882368));
#44664=CARTESIAN_POINT('',(-0.00178375572217991,0.0191195601331886,0.0426562849943036));
#44665=CARTESIAN_POINT('',(-0.00127851800713429,0.0191592938373893,0.0426437722637567));
#44666=CARTESIAN_POINT('',(-0.000846210903470214,0.019182682757136,0.042633068638827));
#44667=CARTESIAN_POINT('',(-0.000489776321299228,0.019194662079583,0.0426242354581687));
#44668=CARTESIAN_POINT('',(-0.000249869930458502,0.0191986202501759,0.0426182746804729));
#44669=CARTESIAN_POINT('',(-0.000124192823849701,0.0191996863541797,0.0426151432531564));
#44670=CARTESIAN_POINT('',(-4.6679784386015E-5,0.0191999290556816,0.0426132061190403));
#44671=CARTESIAN_POINT('',(-3.55273807247816E-5,0.0192000724718196,0.0426129275911167));
#44672=CARTESIAN_POINT('',(0.000132725872022036,0.0191997674150739,0.0426087113417112));
#44673=CARTESIAN_POINT('',(0.000301334959408398,0.0191979264153387,0.0426044875461309));
#44674=CARTESIAN_POINT('',(0.000620058787525162,0.0191915262452281,0.0425965042664429));
#44675=CARTESIAN_POINT('',(0.00105625017562631,0.0191732552424566,0.042585580121496));
#44676=CARTESIAN_POINT('',(0.00157586498512921,0.0191375540444232,0.0425725590697522));
#44677=CARTESIAN_POINT('',(0.00225352720874131,0.0190725286873344,0.0425555563992737));
#44678=CARTESIAN_POINT('',(0.00307577592015579,0.0189604661224298,0.0425348667722705));
#44679=CARTESIAN_POINT('',(0.00433461762632953,0.0187229113146007,0.042502996563044));
#44680=CARTESIAN_POINT('',(0.00550296403284533,0.0184106330699154,0.0424730401318015));
#44681=CARTESIAN_POINT('',(0.00645166983970761,0.0180871524016339,0.0424482907150997));
#44682=CARTESIAN_POINT('',(0.0069619172411926,0.017895080795899,0.0424348530334128));
#44683=CARTESIAN_POINT('',(0.00735895883345079,0.0177350110020672,0.0424243268030787));
#44684=CARTESIAN_POINT('',(0.00764643716145475,0.0176127467126435,0.0424166296301185));
#44685=CARTESIAN_POINT('',(0.00811981898701091,0.0174022159675745,0.0424037960919214));
#44686=CARTESIAN_POINT('',(0.00876944710166559,0.0170887290080066,0.0423858318340952));
#44687=CARTESIAN_POINT('',(0.00951315708613044,0.0166847494227937,0.0423646407192132));
#44688=CARTESIAN_POINT('',(0.0100790413869899,0.0163436474742964,0.0423480383242041));
#44689=CARTESIAN_POINT('',(0.0104056123469378,0.0161368273680414,0.0423383123596306));
#44690=CARTESIAN_POINT('',(0.0106773257678165,0.0159581190475695,0.0423301204250104));
#44691=CARTESIAN_POINT('',(0.0108709588255067,0.0158265622046039,0.0423242248261542));
#44692=CARTESIAN_POINT('',(0.0111500967747105,0.015632249483432,0.0423156711224693));
#44693=CARTESIAN_POINT('',(0.0116135143005295,0.015295404023264,0.04230128967554));
#44694=CARTESIAN_POINT('',(0.0121187756985194,0.0148979561232106,0.0422852165665296));
#44695=CARTESIAN_POINT('',(0.0125939722026192,0.0144949013505583,0.0422696964213244));
#44696=CARTESIAN_POINT('',(0.0129353033061177,0.0141911492153154,0.0422583475135069));
#44697=CARTESIAN_POINT('',(0.0132118784921364,0.013932722585271,0.0422489739755852));
#44698=CARTESIAN_POINT('',(0.0133921363015402,0.0137587491919012,0.0422427835420144));
#44699=CARTESIAN_POINT('',(0.0135049874974253,0.0136475723361838,0.0422388740275091));
#44700=CARTESIAN_POINT('',(0.0135562891590839,0.013596963006152,0.0422370968087094));
#44701=CARTESIAN_POINT('',(0.0137309751687791,0.0134208586502648,0.0422309823553245));
#44702=CARTESIAN_POINT('',(0.0139110674958282,0.0132343715184421,0.0422245911612597));
#44703=CARTESIAN_POINT('',(0.014137592520735,0.0129930306245759,0.0422164308470755));
#44704=CARTESIAN_POINT('',(0.0143812101760025,0.012722482322191,0.0422074541024341));
#44705=CARTESIAN_POINT('',(0.0146807978338182,0.0123774570750208,0.0421961857196092));
#44706=CARTESIAN_POINT('',(0.0150050919875872,0.0119830224113509,0.0421835912660922));
#44707=CARTESIAN_POINT('',(0.0153221172843545,0.0115735139904246,0.0421708117041865));
#44708=CARTESIAN_POINT('',(0.0155727474341347,0.0112327867664899,0.0421603668629035));
#44709=CARTESIAN_POINT('',(0.0157608818977209,0.0109663563764849,0.0421523048467191));
#44710=CARTESIAN_POINT('',(0.0158724187713138,0.0108032907586352,0.0421474110573046));
#44711=CARTESIAN_POINT('',(0.015920938994233,0.0107315178459205,0.0421452606250145));
#44712=CARTESIAN_POINT('',(0.0159505791891584,0.0106873007672264,0.0421439337517554));
#44713=CARTESIAN_POINT('',(0.015945066621156,0.0106956996029432,0.0421441861147551));
#44714=CARTESIAN_POINT('',(0.0160294734566912,0.0105689614014762,0.0421403759015017));
#44715=CARTESIAN_POINT('',(0.016109585952249,0.0104465073799381,0.0421367138763467));
#44716=CARTESIAN_POINT('',(0.0162190528755293,0.0102763008430629,0.0421316482460841));
#44717=CARTESIAN_POINT('',(0.0163433133630848,0.0100774090294254,0.0421257758606307));
#44718=CARTESIAN_POINT('',(0.0165073176998543,0.00980776814333849,0.0421178704423418));
#44719=CARTESIAN_POINT('',(0.0167055244977741,0.00946782764719573,0.0421080091426432));
#44720=CARTESIAN_POINT('',(0.0169335320293294,0.00905371540032421,0.0420961542095714));
#44721=CARTESIAN_POINT('',(0.0171510782008102,0.00863455858579092,0.0420843034014677));
#44722=CARTESIAN_POINT('',(0.0173587805779037,0.00820886568577517,0.0420724088552192));
#44723=CARTESIAN_POINT('',(0.0175214623450828,0.00785396744808819,0.0420625985799328));
#44724=CARTESIAN_POINT('',(0.0176338988238206,0.00759567097700161,0.042055515377216));
#44725=CARTESIAN_POINT('',(0.0176918003353244,0.00745968562854511,0.0420517984670205));
#44726=CARTESIAN_POINT('',(0.0177486744917219,0.00732308913251824,0.0420480760415315));
#44727=CARTESIAN_POINT('',(0.0177509115770147,0.00731742321369519,0.0420479242320732));
#44728=CARTESIAN_POINT('',(0.0177761573272115,0.00725608237038993,0.0420462630915224));
#44729=CARTESIAN_POINT('',(0.0178177081338389,0.00715380871307502,0.0420435119330493));
#44730=CARTESIAN_POINT('',(0.0179324378360052,0.00686538158825476,0.0420358069385859));
#44731=CARTESIAN_POINT('',(0.018112361246438,0.00638436331410489,0.04202312787808));
#44732=CARTESIAN_POINT('',(0.018325840757539,0.00573631041106067,0.0420063211939584));
#44733=CARTESIAN_POINT('',(0.0184670742169264,0.00526192427057464,0.0419941430133837));
#44734=CARTESIAN_POINT('',(0.0185813044969062,0.00483863311912185,0.0419833616396935));
#44735=CARTESIAN_POINT('',(0.0186659401494481,0.00450204727579162,0.0419748302421681));
#44736=CARTESIAN_POINT('',(0.0187366075089475,0.00419556750954496,0.0419671013379643));
#44737=CARTESIAN_POINT('',(0.0187882700525209,0.00395705887023389,0.0419611053876857));
#44738=CARTESIAN_POINT('',(0.0188355216601128,0.00372453810855936,0.0419552769852958));
#44739=CARTESIAN_POINT('',(0.0188459268142927,0.00367031565686944,0.0419539197122962));
#44740=CARTESIAN_POINT('',(0.0188723933446082,0.00353309330142448,0.0419504809509566));
#44741=CARTESIAN_POINT('',(0.0189121053612324,0.00331649859254612,0.0419450518953231));
#44742=CARTESIAN_POINT('',(0.0189696566091318,0.00297547776343546,0.0419364996287203));
#44743=CARTESIAN_POINT('',(0.0190320962233435,0.00254661211898106,0.0419257401145415));
#44744=CARTESIAN_POINT('',(0.0191064706331641,0.00193756668593801,0.0419104555385234));
#44745=CARTESIAN_POINT('',(0.0191772638259746,0.00111160555292925,0.0418897173539831));
#44746=CARTESIAN_POINT('',(0.0192,0.000381663654322056,0.0418713583471171));
#44747=CARTESIAN_POINT('',(0.0192,-4.02812422912431E-17,0.0418617389925214));
#44748=CARTESIAN_POINT('',(-0.0192,-1.94617121099498E-14,0.0433622164621474));
#44749=CARTESIAN_POINT('',(0.0192,6.20369116582113E-17,0.044861351498379));
#44750=CARTESIAN_POINT('',(0.0192,-0.00251327412287178,0.044798887538536));
#44751=CARTESIAN_POINT('',(0.0182002919343753,-0.00753865073535333,0.0446739596188501));
#44752=CARTESIAN_POINT('',(0.0139299003749868,-0.0139299426504138,0.0444865677393211));
#44753=CARTESIAN_POINT('',(0.00753880775836791,-0.0182002798556818,0.0442991758597921));
#44754=CARTESIAN_POINT('',(-2.05686929275178E-17,-0.0196998600721591,0.0441117839802632));
#44755=CARTESIAN_POINT('',(-0.00753880775836791,-0.0182002798556818,0.0439243921007342));
#44756=CARTESIAN_POINT('',(-0.0139299003749868,-0.0139299426504137,0.0437370002212053));
#44757=CARTESIAN_POINT('',(-0.0182002919343753,-0.00753865073535333,0.0435496083416764));
#44758=CARTESIAN_POINT('',(-0.0192,-0.00251327412287176,0.0434246804219904));
#44759=CARTESIAN_POINT('',(-0.0192,8.05624845824862E-17,0.0433622164621474));
#44760=CARTESIAN_POINT('',(0.0192,3.74901540623289E-17,0.044861351498379));
#44761=CARTESIAN_POINT('',(0.0134577614771412,0.0136941102677163,0.0452414742614655));
#44762=CARTESIAN_POINT('',(0.0136855201965706,0.0134702824716422,0.0452335016921451));
#44763=CARTESIAN_POINT('',(0.0141298762423033,0.0130112461702288,0.0452175335389093));
#44764=CARTESIAN_POINT('',(0.0147611864198779,0.0122903912231453,0.0451935160925514));
#44765=CARTESIAN_POINT('',(0.0152568174315112,0.0116639372101018,0.0451734376386303));
#44766=CARTESIAN_POINT('',(0.0156338613138156,0.0111489679873024,0.0451573575763656));
#44767=CARTESIAN_POINT('',(0.0158622047786986,0.0108200703234377,0.0451472556778677));
#44768=CARTESIAN_POINT('',(0.0160161124866989,0.0105894382716242,0.0451402525654601));
#44769=CARTESIAN_POINT('',(0.0161053175604917,0.0104528771547491,0.0451361303424177));
#44770=CARTESIAN_POINT('',(0.016154666013204,0.0103764619483118,0.0451338308807265));
#44771=CARTESIAN_POINT('',(0.0162073223318096,0.0102938574043665,0.0451313536193738));
#44772=CARTESIAN_POINT('',(0.0162105065664181,0.0102887837226033,0.0451312024072254));
#44773=CARTESIAN_POINT('',(0.0162276362812458,0.0102618121619652,0.0451303990393071));
#44774=CARTESIAN_POINT('',(0.0162656449954779,0.0102015708728732,0.0451286212751449));
#44775=CARTESIAN_POINT('',(0.0163518542543136,0.0100635898383705,0.0451245826096027));
#44776=CARTESIAN_POINT('',(0.0165458020487241,0.0097441841874731,0.0451153427643101));
#44777=CARTESIAN_POINT('',(0.0168210008826648,0.00926799885690159,0.0451017819588008));
#44778=CARTESIAN_POINT('',(0.0171567968830624,0.00862548394619102,0.0450839282812965));
#44779=CARTESIAN_POINT('',(0.0174318062881837,0.00805757222941041,0.0450683983614061));
#44780=CARTESIAN_POINT('',(0.0176741525058544,0.00750847684832872,0.0450536336429448));
#44781=CARTESIAN_POINT('',(0.0178699501137322,0.00702574106353254,0.0450408207709287));
#44782=CARTESIAN_POINT('',(0.0179822065441399,0.00673081700074846,0.0450330602954559));
#44783=CARTESIAN_POINT('',(0.0180534349049712,0.00653593891772145,0.0450279578728813));
#44784=CARTESIAN_POINT('',(0.018108461643912,0.00638211837966673,0.0450239406980777));
#44785=CARTESIAN_POINT('',(0.0181209638386689,0.00634584696742375,0.0450229966878678));
#44786=CARTESIAN_POINT('',(0.0181500355739649,0.00626254619710393,0.0450208223787282));
#44787=CARTESIAN_POINT('',(0.0182027591255457,0.00610851249593621,0.0450168028334002));
#44788=CARTESIAN_POINT('',(0.0183281524290541,0.00573045201233244,0.0450069368917786));
#44789=CARTESIAN_POINT('',(0.018539378786679,0.00502322040266667,0.0449885388735071));
#44790=CARTESIAN_POINT('',(0.0187521753782728,0.00415974937968944,0.0449662614921629));
#44791=CARTESIAN_POINT('',(0.0189149832005711,0.00331540125865183,0.044944641160551));
#44792=CARTESIAN_POINT('',(0.0190333696277108,0.0025692626256965,0.0449256334103954));
#44793=CARTESIAN_POINT('',(0.0191322007628907,0.00170925695092131,0.0449039322303267));
#44794=CARTESIAN_POINT('',(0.0191903413400752,0.000786870471325928,0.0448808604775793));
#44795=CARTESIAN_POINT('',(0.0192,0.000249323547247888,0.0448675179844314));
#44796=CARTESIAN_POINT('',(0.0192,6.20369116582113E-17,0.044861351498379));
#44797=CARTESIAN_POINT('',(0.0134577620733179,0.0136941154998904,0.0452413722509897));
#44798=CARTESIAN_POINT('',(0.0134693251163026,0.0136827518905366,0.0452383139305518));
#44799=CARTESIAN_POINT('',(0.0135091245810281,0.0136433186594187,0.0452279191596696));
#44800=CARTESIAN_POINT('',(0.0137222886796034,0.0134398023342058,0.0451722602640239));
#44801=CARTESIAN_POINT('',(0.0138190249762464,0.0133538551974653,0.045147745444006));
#44802=CARTESIAN_POINT('',(0.0138718459707152,0.0133075728375538,0.0451344229377038));
#44803=CARTESIAN_POINT('',(0.,-0.0120000000000245,0.050900001));
#44804=CARTESIAN_POINT('',(0.,0.,0.050900001));
#44805=CARTESIAN_POINT('',(-0.0120000000000245,0.,0.050900001));
#44806=CARTESIAN_POINT('',(0.,0.,0.050900001));
#44807=CARTESIAN_POINT('',(-0.0192,0.,0.050900001));
#44808=CARTESIAN_POINT('',(0.,-0.0192,0.0489));
#44809=CARTESIAN_POINT('',(0.,0.,0.0489));
#44810=CARTESIAN_POINT('',(0.019,0.,0.0489));
#44811=CARTESIAN_POINT('',(0.,0.,0.0489));
#44812=CARTESIAN_POINT('',(0.0130000000000245,0.,0.0489));
#44813=CARTESIAN_POINT('',(0.,-0.0212,0.0332));
#44814=CARTESIAN_POINT('',(0.,0.,0.0332));
#44815=CARTESIAN_POINT('',(-0.0212,0.,0.0332));
#44816=CARTESIAN_POINT('',(0.,0.,0.0332));
#44817=CARTESIAN_POINT('',(0.0194,0.,0.0332));
#44818=CARTESIAN_POINT('',(0.0133472984199003,0.013834010563528,0.0361523640312405));
#44819=CARTESIAN_POINT('',(0.0136128985927427,0.0137274518465872,0.0359418834605953));
#44820=CARTESIAN_POINT('',(0.0136795294310282,0.0135039659523647,0.0356739008696272));
#44821=CARTESIAN_POINT('',(0.0134661557341698,0.0136975950548514,0.0361775333758731));
#44822=CARTESIAN_POINT('',(0.0136086981289552,0.0136172271430925,0.0360110987392474));
#44823=CARTESIAN_POINT('',(0.0136923375685161,0.013469742563547,0.035850717259336));
#44824=CARTESIAN_POINT('',(0.0135994539125629,0.0135548405221097,0.0362044425855375));
#44825=CARTESIAN_POINT('',(0.0136557312369491,0.0134970649841054,0.0361223786925854));
#44826=CARTESIAN_POINT('',(0.0137121251631036,0.0134394533765344,0.0360402698661124));
#44827=CARTESIAN_POINT('',(0.0137371549655767,0.0134138202407715,0.0362316337644044));
#44828=CARTESIAN_POINT('',(0.0137371549655767,0.0134138202407715,0.0362316337644044));
#44829=CARTESIAN_POINT('',(0.0137371549655767,0.0134138202407715,0.0362316337644044));
#44830=CARTESIAN_POINT('',(0.0136559709074636,0.013527425587518,0.034318741929522));
#44831=CARTESIAN_POINT('',(0.0135793479802664,0.013759152940594,0.0340623518581637));
#44832=CARTESIAN_POINT('',(0.0133075405240014,0.0138718879878007,0.0338655879801856));
#44833=CARTESIAN_POINT('',(0.0136626512276672,0.0134997252191483,0.0341411899032202));
#44834=CARTESIAN_POINT('',(0.013573293989727,0.0136518751809117,0.0339895570776138));
#44835=CARTESIAN_POINT('',(0.0134253578297479,0.0137374428278113,0.0338316666320085));
#44836=CARTESIAN_POINT('',(0.0136758218608079,0.013476371070873,0.03395063623351));
#44837=CARTESIAN_POINT('',(0.0136166570008004,0.0135364342732092,0.033872945275307));
#44838=CARTESIAN_POINT('',(0.0135576402206721,0.0135966282545905,0.033795255466116));
#44839=CARTESIAN_POINT('',(0.0136941106116928,0.0134577611271237,0.0337585246088596));
#44840=CARTESIAN_POINT('',(0.0136941106116928,0.0134577611271237,0.0337585246088596));
#44841=CARTESIAN_POINT('',(0.0136941106116929,0.0134577611271237,0.0337585246088596));
#44842=CARTESIAN_POINT('',(0.0135274197783297,0.0136559722321683,0.0446813017208849));
#44843=CARTESIAN_POINT('',(0.0137591216978861,0.0135793490080532,0.0449376690887189));
#44844=CARTESIAN_POINT('',(0.0138718493711407,0.0133075760157034,0.045134425378585));
#44845=CARTESIAN_POINT('',(0.0134997222462602,0.0136626530426041,0.0448588356204341));
#44846=CARTESIAN_POINT('',(0.0136518575203163,0.0135733015815387,0.0450104603247853));
#44847=CARTESIAN_POINT('',(0.0137374220236025,0.0134253776620627,0.0451683385915406));
#44848=CARTESIAN_POINT('',(0.0134763694953618,0.0136758234091799,0.0450493806425446));
#44849=CARTESIAN_POINT('',(0.0135364280715176,0.0136166631201245,0.0451270635743358));
#44850=CARTESIAN_POINT('',(0.0135966170774267,0.0135576512053218,0.0452047477806426));
#44851=CARTESIAN_POINT('',(0.0134577611073142,0.0136941106311604,0.045241474274411));
#44852=CARTESIAN_POINT('',(0.0134577611073142,0.0136941106311604,0.045241474274411));
#44853=CARTESIAN_POINT('',(0.0134577611073142,0.0136941106311604,0.0452414742744111));
#44854=CARTESIAN_POINT('',(0.0138344560633967,0.0133469119961932,0.0428477145766618));
#44855=CARTESIAN_POINT('',(0.0137278240280446,0.0136129157959794,0.0430583504712027));
#44856=CARTESIAN_POINT('',(0.0135040802168539,0.0136794867633816,0.0433266840430608));
#44857=CARTESIAN_POINT('',(0.0136984847986298,0.0134653599156988,0.0428226323586712));
#44858=CARTESIAN_POINT('',(0.0136177534369767,0.0136086105319708,0.0429893073493089));
#44859=CARTESIAN_POINT('',(0.013469952068938,0.0136922398391085,0.0431504402352761));
#44860=CARTESIAN_POINT('',(0.0135541740640735,0.0136001046836198,0.0427954286245404));
#44861=CARTESIAN_POINT('',(0.0134968084997804,0.0136559821004703,0.0428772848614511));
#44862=CARTESIAN_POINT('',(0.0134393323812074,0.0137122433104624,0.0429588263990224));
#44863=CARTESIAN_POINT('',(0.0134138202606126,0.0137371549462027,0.0427683673505048));
#44864=CARTESIAN_POINT('',(0.0134138202606126,0.0137371549462027,0.0427683673505048));
#44865=CARTESIAN_POINT('',(0.0134138202606126,0.0137371549462026,0.0427683673505048));
#44866=CARTESIAN_POINT('',(0.,0.,0.));
#44867=CARTESIAN_POINT('',(0.,0.,0.0487));
#44868=CARTESIAN_POINT('',(0.0192,0.,0.0487));
#44869=CARTESIAN_POINT('',(0.,0.,0.0334));
#44870=CARTESIAN_POINT('',(0.0192,0.,0.0334));
#44871=CARTESIAN_POINT('',(0.,0.,0.));
#44872=CARTESIAN_POINT('',(0.,0.,0.0499));
#44873=CARTESIAN_POINT('',(0.0120000000000245,0.,0.0499));
#44874=CARTESIAN_POINT('',(0.,0.,0.));
#44875=CARTESIAN_POINT('',(0.,0.,0.048900001));
#44876=CARTESIAN_POINT('',(-0.0212,0.,0.048900001));
#44877=CARTESIAN_POINT('',(0.0128751173724028,0.0144085717216295,0.0429735312461257));
#44878=CARTESIAN_POINT('',(0.0131333244250874,0.0141707592149881,0.042964717528887));
#44879=CARTESIAN_POINT('',(0.0133904435253121,0.0139280160341615,0.0429559068947327));
#44880=CARTESIAN_POINT('',(0.0158987497722569,0.0114264395544413,0.0428683193785747));
#44881=CARTESIAN_POINT('',(0.0175920161811642,0.00859581528207105,0.0427891876797143));
#44882=CARTESIAN_POINT('',(0.0194222911783444,0.00247676590716676,0.0426313696477661));
#44883=CARTESIAN_POINT('',(0.019562963909536,-0.000810843784974266,0.0425524653615877));
#44884=CARTESIAN_POINT('',(0.0182606575169193,-0.00706581685312737,0.0423944750844562));
#44885=CARTESIAN_POINT('',(0.0168183760123872,-0.0100242050478105,0.042315562410242));
#44886=CARTESIAN_POINT('',(0.0126966573657828,-0.0149044022188295,0.0421577017371009));
#44887=CARTESIAN_POINT('',(0.0100210068874356,-0.0168212406508217,0.0420787719850549));
#44888=CARTESIAN_POINT('',(0.00407243963060028,-0.0191515920325448,0.0419208058699113));
#44889=CARTESIAN_POINT('',(0.000806848361851911,-0.019562531967154,0.0418418755928234));
#44890=CARTESIAN_POINT('',(-0.00553306068688165,-0.018781161179321,0.0416840174919447));
#44891=CARTESIAN_POINT('',(-0.00860120532063141,-0.0175895931973386,0.0416050879420078));
#44892=CARTESIAN_POINT('',(-0.0138056580461542,-0.0138842419326171,0.0414471211199442));
#44893=CARTESIAN_POINT('',(-0.0159357918461525,-0.0113751566036123,0.0413681914665986));
#44894=CARTESIAN_POINT('',(-0.0187492557985244,-0.00564022844013249,0.0412103332713815));
#44895=CARTESIAN_POINT('',(-0.0194298312204639,-0.00241995492611967,0.0411314037292813));
#44896=CARTESIAN_POINT('',(-0.0191744011757895,0.0039636736746371,0.0409734369221964));
#44897=CARTESIAN_POINT('',(-0.0182389517901175,0.0071192897701119,0.040894507254258));
#44898=CARTESIAN_POINT('',(-0.0149766811072747,0.0126113358866933,0.0407366490611891));
#44899=CARTESIAN_POINT('',(-0.0126530155410305,0.0149424134885897,0.0406577195188047));
#44900=CARTESIAN_POINT('',(-0.00716914867521055,0.0182200899183962,0.040499752711441));
#44901=CARTESIAN_POINT('',(-0.0040157303431181,0.0191629214644348,0.0404208230437047));
#44902=CARTESIAN_POINT('',(0.00236631950412073,0.0194357223134969,0.0402629648507107));
#44903=CARTESIAN_POINT('',(0.00558874413207926,0.0187654059953617,0.0401840353082519));
#44904=CARTESIAN_POINT('',(0.011332095847439,0.0159672155702773,0.0400260685009428));
#44905=CARTESIAN_POINT('',(0.0138461591609683,0.0138429594282163,0.0399471388332248));
#44906=CARTESIAN_POINT('',(0.017565189295934,0.00864932915543225,0.0397892806401376));
#44907=CARTESIAN_POINT('',(0.0187665221595431,0.00558499500257808,0.0397103510977194));
#44908=CARTESIAN_POINT('',(0.0195652865780699,-0.000753611625385773,0.0395523842904227));
#44909=CARTESIAN_POINT('',(0.0191619928435045,-0.0040201591400539,0.0394734546227174));
#44910=CARTESIAN_POINT('',(0.0168481763607773,-0.00997425301230359,0.0393155964295924));
#44911=CARTESIAN_POINT('',(0.0149398853269601,-0.0126560005357337,0.039236666887228));
#44912=CARTESIAN_POINT('',(0.0100702990665986,-0.016791588551228,0.0390787000798614));
#44913=CARTESIAN_POINT('',(0.00711507422239091,-0.0182405967022088,0.0389997704121751));
#44914=CARTESIAN_POINT('',(0.000864968760624566,-0.0195601277829158,0.038841912219082));
#44915=CARTESIAN_POINT('',(-0.00242383663527852,-0.0194293473670445,0.0387629826766795));
#44916=CARTESIAN_POINT('',(-0.00854942352561615,-0.0176146452346672,0.0386050158693573));
#44917=CARTESIAN_POINT('',(-0.0113788393619798,-0.0159331623988121,0.038526086201702));
#44918=CARTESIAN_POINT('',(-0.0159019902197058,-0.0114224987144947,0.0383682280085025));
#44919=CARTESIAN_POINT('',(-0.0175913112934338,-0.00859769097603843,0.0382892984661209));
#44920=CARTESIAN_POINT('',(-0.0194224819673239,-0.00247700698301382,0.0381313316588633));
#44921=CARTESIAN_POINT('',(-0.0195623446832896,0.000811369048211784,0.0380524019910925));
#44922=CARTESIAN_POINT('',(-0.0182600972832356,0.00706509851662393,0.0378945437980595));
#44923=CARTESIAN_POINT('',(-0.016819233986536,0.0100243648801336,0.0378156142556532));
#44924=CARTESIAN_POINT('',(-0.0126967579507606,0.0149050564206465,0.0376576474482783));
#44925=CARTESIAN_POINT('',(-0.0100203374244886,0.0168207160115748,0.0375787177806155));
#44926=CARTESIAN_POINT('',(-0.004072662932392,0.0191509839559279,0.0374208595874837));
#44927=CARTESIAN_POINT('',(-0.000807186806473285,0.0195633067910464,0.0373419300450818));
#44928=CARTESIAN_POINT('',(0.00553354521670946,0.018781593295045,0.0371839632377971));
#44929=CARTESIAN_POINT('',(0.00860113448735149,0.0175887502336188,0.0371050335701185));
#44930=CARTESIAN_POINT('',(0.0138050263039444,0.0138840922850618,0.0369471753769281));
#44931=CARTESIAN_POINT('',(0.0159362553123575,0.0113758643522062,0.0368682458345405));
#44932=CARTESIAN_POINT('',(0.0187498826791494,0.00564005929796595,0.0367102790272858));
#44933=CARTESIAN_POINT('',(0.0194290867556229,0.00241955307612708,0.0366313493595608));
#44934=CARTESIAN_POINT('',(0.0191739303520504,-0.00396322655069507,0.036473491166433));
#44935=CARTESIAN_POINT('',(0.0182397977873896,-0.00711929068202113,0.0363945616240418));
#44936=CARTESIAN_POINT('',(0.0149768823760523,-0.0126119532056393,0.0362365948167335));
#44937=CARTESIAN_POINT('',(0.0126522719426653,-0.0149420100364957,0.0361576651490156));
#44938=CARTESIAN_POINT('',(0.00716926547582709,-0.0182194512093103,0.0359998069559463));
#44939=CARTESIAN_POINT('',(0.00401619229775511,-0.0191636302044921,0.0359208774133096));
#44940=CARTESIAN_POINT('',(-0.0023667262209589,-0.0194362284487689,0.0357629106062309));
#44941=CARTESIAN_POINT('',(-0.00558881308252601,-0.0187645628162864,0.0356839809387912));
#44942=CARTESIAN_POINT('',(-0.0113314972464994,-0.0159669640166278,0.0355261227436458));
#44943=CARTESIAN_POINT('',(-0.0138464999243795,-0.0138437337554346,0.0354471932155239));
#44944=CARTESIAN_POINT('',(-0.01756583540215,-0.00864926556607988,0.0352892263937148));
#44945=CARTESIAN_POINT('',(-0.018765854056893,-0.00558447602392299,0.0352102967174342));
#44946=CARTESIAN_POINT('',(-0.0195647493008025,0.000753248602856806,0.0350524386178169));
#44947=CARTESIAN_POINT('',(-0.0191628223557256,0.00402001703766339,0.0349735084674251));
#44948=CARTESIAN_POINT('',(-0.0168484806950671,0.00997483127891498,0.0348155423423861));
#44949=CARTESIAN_POINT('',(-0.014939075025363,0.0126557229800961,0.0347366124977029));
#44950=CARTESIAN_POINT('',(-0.0100702823681381,0.0167909070241343,0.0345787517858474));
#44951=CARTESIAN_POINT('',(-0.00711585876291648,0.0182414349753937,0.0344998392303287));
#44952=CARTESIAN_POINT('',(-0.000864400312993994,0.0195605093863205,0.0343418491020202));
#44953=CARTESIAN_POINT('',(0.0024235334564365,0.0194289217552847,0.0342629443605591));
#44954=CARTESIAN_POINT('',(0.0085476414010583,0.0176156446635616,0.0341051266538377));
#44955=CARTESIAN_POINT('',(0.0113888335904153,0.0159241881786858,0.0340257855313145));
#44956=CARTESIAN_POINT('',(0.0138919024844783,0.013427851971904,0.0339383847815977));
#44957=CARTESIAN_POINT('',(0.014134362965028,0.0131716883241156,0.0339295970016211));
#44958=CARTESIAN_POINT('',(0.0143721856923585,0.0129134700672116,0.0339207829037038));
#44959=CARTESIAN_POINT('',(0.013244880717954,0.0148039903320255,0.0431369141780147));
#44960=CARTESIAN_POINT('',(0.0135065467987276,0.014562992009576,0.0431279823892726));
#44961=CARTESIAN_POINT('',(0.0137690967913546,0.0143151389119729,0.0431191067182131));
#44962=CARTESIAN_POINT('',(0.0163483463147584,0.0117415761632288,0.04303142627739));
#44963=CARTESIAN_POINT('',(0.0180872928602693,0.00883212246784146,0.0429523232752052));
#44964=CARTESIAN_POINT('',(0.0199672051382433,0.00254146260767922,0.042794576298));
#44965=CARTESIAN_POINT('',(0.0201112200424338,-0.00083757785566147,0.042715711296312));
#44966=CARTESIAN_POINT('',(0.0187705210453593,-0.00726924770963437,0.0425575818040092));
#44967=CARTESIAN_POINT('',(0.0172869776211763,-0.0103097002776528,0.0424787150432717));
#44968=CARTESIAN_POINT('',(0.0130490476432779,-0.0153249931900973,0.0423209135715474));
#44969=CARTESIAN_POINT('',(0.0102983988238696,-0.0172948889052652,0.0422420144205481));
#44970=CARTESIAN_POINT('',(0.00418102238433576,-0.019689679955431,0.0420839261351123));
#44971=CARTESIAN_POINT('',(0.000824147707122541,-0.020110982597467,0.0420050253753412));
#44972=CARTESIAN_POINT('',(-0.00569243630278051,-0.0193062101235236,0.0418472297219421));
#44973=CARTESIAN_POINT('',(-0.00884600679789724,-0.0180808786993726,0.0417683304244268));
#44974=CARTESIAN_POINT('',(-0.0141967388150451,-0.0142694498651659,0.0416102406980189));
#44975=CARTESIAN_POINT('',(-0.0163854744768955,-0.0116896130235589,0.0415313413624343));
#44976=CARTESIAN_POINT('',(-0.0192759793352938,-0.00579397917775157,0.041373545475094));
#44977=CARTESIAN_POINT('',(-0.0199750126908028,-0.00248372302623619,0.0412946462125953));
#44978=CARTESIAN_POINT('',(-0.0197107852448881,0.00408038461059604,0.0411365565175739));
#44979=CARTESIAN_POINT('',(-0.0187481572506002,0.00732375763574827,0.0410576571475741));
#44980=CARTESIAN_POINT('',(-0.0153934865396828,0.0129681974909316,0.0408998612656592));
#44981=CARTESIAN_POINT('',(-0.0130045860573409,0.0153639432955975,0.0408209620020816));
#44982=CARTESIAN_POINT('',(-0.00736481647076704,0.0187329675119329,0.040662872306547));
#44983=CARTESIAN_POINT('',(-0.00412306568888511,0.0197010445290123,0.0405839729369947));
#44984=CARTESIAN_POINT('',(0.00243710111309297,0.019979842646596,0.0404261770552279));
#44985=CARTESIAN_POINT('',(0.00574934390972627,0.0192902839979054,0.0403472777915276));
#44986=CARTESIAN_POINT('',(0.0116544396358271,0.0164115395447182,0.0401891880960528));
#44987=CARTESIAN_POINT('',(0.0142379508821379,0.0142271424006341,0.0401102887265381));
#44988=CARTESIAN_POINT('',(0.0180594224696077,0.00888767877911417,0.0399524928446313));
#44989=CARTESIAN_POINT('',(0.0192937721810321,0.00573762730904085,0.0398735935809895));
#44990=CARTESIAN_POINT('',(0.0201135650562981,-0.000780444860065475,0.0397155038855382));
#44991=CARTESIAN_POINT('',(0.0196979077097771,-0.00413802586633374,0.0396366045160817));
#44992=CARTESIAN_POINT('',(0.0173180345998703,-0.0102576435700848,0.039478808634035));
#44993=CARTESIAN_POINT('',(0.015356042405559,-0.0130139146204963,0.0393999093704902));
#44994=CARTESIAN_POINT('',(0.0103477150858215,-0.0172652653022394,0.0392418196749849));
#44995=CARTESIAN_POINT('',(0.00730951779926764,-0.0187537136523111,0.0391629203054914));
#44996=CARTESIAN_POINT('',(0.000884711783842049,-0.020108477293814,0.0390051244235729));
#44997=CARTESIAN_POINT('',(-0.0024958539615088,-0.0199735005723642,0.0389262251599531));
#44998=CARTESIAN_POINT('',(-0.00879423764234924,-0.0181059652530067,0.0387681354644694));
#44999=CARTESIAN_POINT('',(-0.011702053115772,-0.0163765924140203,0.0386892360951575));
#45000=CARTESIAN_POINT('',(-0.016350251638447,-0.0117389456667314,0.038531440212854));
#45001=CARTESIAN_POINT('',(-0.0180862478599091,-0.00883502407804941,0.0384525409493668));
#45002=CARTESIAN_POINT('',(-0.0199676992469986,-0.00254078339015984,0.0382944512540031));
#45003=CARTESIAN_POINT('',(-0.0201103505948417,0.000839419538129869,0.0382155518843851));
#45004=CARTESIAN_POINT('',(-0.0187701918210865,0.00726728787221907,0.0380577560025739));
#45005=CARTESIAN_POINT('',(-0.0172886259471365,0.0103089002794402,0.037978856738934));
#45006=CARTESIAN_POINT('',(-0.0130483550078281,0.015326611662146,0.0378207670433832));
#45007=CARTESIAN_POINT('',(-0.0102965853185908,0.0172948303544054,0.0377418676739293));
#45008=CARTESIAN_POINT('',(-0.00418239204957526,0.0196886050994017,0.037584071791977));
#45009=CARTESIAN_POINT('',(-0.000825716376582044,0.0201118921182084,0.0375051725283272));
#45010=CARTESIAN_POINT('',(0.0056941517708637,0.0193065074279527,0.0373470828329373));
#45011=CARTESIAN_POINT('',(0.00884695384515193,0.0180793316767743,0.0372681834635453));
#45012=CARTESIAN_POINT('',(0.0141950885647465,0.0142700047178758,0.0371103875813084));
#45013=CARTESIAN_POINT('',(0.0163853778444867,0.0116914244214254,0.0370314883177673));
#45014=CARTESIAN_POINT('',(0.0192771666541589,0.00579270569280173,0.0368733986224446));
#45015=CARTESIAN_POINT('',(0.0199742355396882,0.00248208396680975,0.03679449925292));
#45016=CARTESIAN_POINT('',(0.0197103471394279,-0.00407869950554762,0.0366367033708807));
#45017=CARTESIAN_POINT('',(0.018749620840931,-0.00732268601191894,0.0365578041072789));
#45018=CARTESIAN_POINT('',(0.0153930698197874,-0.0129698880095284,0.036399714411885));
#45019=CARTESIAN_POINT('',(0.0130027888314922,-0.0153641891687384,0.0363208150423589));
#45020=CARTESIAN_POINT('',(0.00736598756274524,-0.0187316790820181,0.036163019160431));
#45021=CARTESIAN_POINT('',(0.0041247633259904,-0.0197016836759312,0.0360841198963006));
#45022=CARTESIAN_POINT('',(-0.00243874428503272,-0.0199804184070515,0.0359260302013203));
#45023=CARTESIAN_POINT('',(-0.0057505327317695,-0.0192889139048742,0.0358471308327378));
#45024=CARTESIAN_POINT('',(-0.0116527204687135,-0.0164118152451721,0.0356893349457639));
#45025=CARTESIAN_POINT('',(-0.0142375575240833,-0.0142289131365525,0.0356104357158766));
#45026=CARTESIAN_POINT('',(-0.0180608031458059,-0.00888661814352176,0.0354523459896135));
#45027=CARTESIAN_POINT('',(-0.0192932754654998,-0.00573588273138894,0.0353734465854948));
#45028=CARTESIAN_POINT('',(-0.0201128562646196,0.000778855422054386,0.0352156509329156));
#45029=CARTESIAN_POINT('',(-0.0196991696809191,0.00413672481531792,0.0351367502803128));
#45030=CARTESIAN_POINT('',(-0.0173179069910243,0.0102593800136393,0.0349786619865434));
#45031=CARTESIAN_POINT('',(-0.0153542920277628,0.0130144577141355,0.0348997627572814));
#45032=CARTESIAN_POINT('',(-0.0103486360334633,0.017263766075639,0.034741961252782));
#45033=CARTESIAN_POINT('',(-0.00731153357968647,0.0187542778224974,0.0346630945924325));
#45034=CARTESIAN_POINT('',(-0.00088283361010462,0.0201091459479512,0.0345049652257676));
#45035=CARTESIAN_POINT('',(0.00249648070157979,0.0199728080362074,0.0344260998394164));
#45036=CARTESIAN_POINT('',(0.00879141509936053,0.0181072591432389,0.0342683531370332));
#45037=CARTESIAN_POINT('',(0.0117108803520172,0.0163687603127585,0.0341890347296195));
#45038=CARTESIAN_POINT('',(0.0142847430045092,0.0138005869114252,0.0341015476699935));
#45039=CARTESIAN_POINT('',(0.0145322375581197,0.0135389638897274,0.0340926962624872));
#45040=CARTESIAN_POINT('',(0.0147732447934845,0.0132772880232293,0.0340837641415089));
#45041=CARTESIAN_POINT('',(0.0134164396611127,0.0149734662699873,0.0435900976144594));
#45042=CARTESIAN_POINT('',(0.0136796474430364,0.0147310480180751,0.0435811132008271));
#45043=CARTESIAN_POINT('',(0.0139445606758513,0.0144808533047822,0.0435722084496325));
#45044=CARTESIAN_POINT('',(0.0165541803787265,0.0118740244693021,0.0434844866053923));
#45045=CARTESIAN_POINT('',(0.0183120729305598,0.00892862932083445,0.0434053963917));
#45046=CARTESIAN_POINT('',(0.0202110140523984,0.00256064972205639,0.0432476811088157));
#45047=CARTESIAN_POINT('',(0.0203548755530947,-0.000859156831837742,0.0431688335154196));
#45048=CARTESIAN_POINT('',(0.0189940535653762,-0.00736886204407924,0.0430106420675322));
#45049=CARTESIAN_POINT('',(0.0174906492691983,-0.0104451356738669,0.0429317957701886));
#45050=CARTESIAN_POINT('',(0.0131985459197013,-0.0155185165039707,0.0427740206496132));
#45051=CARTESIAN_POINT('',(0.0104135587920133,-0.0175106919071648,0.0426951351063101));
#45052=CARTESIAN_POINT('',(0.00421989511762802,-0.0199312807768646,0.0425369924254557));
#45053=CARTESIAN_POINT('',(0.000822165829661969,-0.0203555687823335,0.0424581048304965));
#45054=CARTESIAN_POINT('',(-0.00577268415217634,-0.0195372110262576,0.0423003369807169));
#45055=CARTESIAN_POINT('',(-0.00896368245745464,-0.0182953203640746,0.0422214511295832));
#45056=CARTESIAN_POINT('',(-0.014377738173501,-0.0144341362566882,0.042063306682774));
#45057=CARTESIAN_POINT('',(-0.0165913177413619,-0.0118217297559613,0.0419844208681352));
#45058=CARTESIAN_POINT('',(-0.0195132569626783,-0.00585314394204532,0.0418266527220008));
#45059=CARTESIAN_POINT('',(-0.0202188985482763,-0.00250249737859145,0.0417477669181936));
#45060=CARTESIAN_POINT('',(-0.0199476524226673,0.00414183628428791,0.0415896225100204));
#45061=CARTESIAN_POINT('',(-0.0189713465461571,0.0074238217144122,0.0415107366521508));
#45062=CARTESIAN_POINT('',(-0.0155727958581524,0.0131344783069039,0.0413529685129072));
#45063=CARTESIAN_POINT('',(-0.0131536962360839,0.0155578477627397,0.0412740827076612));
#45064=CARTESIAN_POINT('',(-0.00744292525627976,0.0189648756528633,0.0411159382988743));
#45065=CARTESIAN_POINT('',(-0.00416136837068427,0.0199426209891001,0.041037052441561));
#45066=CARTESIAN_POINT('',(0.0024782329367654,0.0202209013832472,0.0408792843024956));
#45067=CARTESIAN_POINT('',(0.00583011869197187,0.0195211697322738,0.0408003984971062));
#45068=CARTESIAN_POINT('',(0.0118058639010852,0.0166037713321414,0.0406422540883824));
#45069=CARTESIAN_POINT('',(0.0144192410151831,0.0143913379217445,0.0405633682311128));
#45070=CARTESIAN_POINT('',(0.0182837257384388,0.00898509122716692,0.0404056000918904));
#45071=CARTESIAN_POINT('',(0.0195312415965337,0.00579628789620374,0.0403267142865668));
#45072=CARTESIAN_POINT('',(0.0203573162877559,-0.000802071356869746,0.0401685698778692));
#45073=CARTESIAN_POINT('',(0.0199345230002467,-0.00419998945070916,0.0400896840206814));
#45074=CARTESIAN_POINT('',(0.0175222672957333,-0.0103921431886806,0.0399319158812692));
#45075=CARTESIAN_POINT('',(0.0155350345421537,-0.0131806317546663,0.0398530300760634));
#45076=CARTESIAN_POINT('',(0.010462929394733,-0.0174811542348422,0.03969488566732));
#45077=CARTESIAN_POINT('',(0.00738706026086871,-0.0189856909101189,0.039615999810069));
#45078=CARTESIAN_POINT('',(0.000883817908637908,-0.0203530183791772,0.0394582316708292));
#45079=CARTESIAN_POINT('',(-0.00253752453815646,-0.0202145324184487,0.0393793458655338));
#45080=CARTESIAN_POINT('',(-0.00891195636570637,-0.0183204988642966,0.0392212014567969));
#45081=CARTESIAN_POINT('',(-0.0118538449930932,-0.016568387897323,0.0391423155997955));
#45082=CARTESIAN_POINT('',(-0.0165554621411534,-0.0118719486406755,0.0389845474600498));
#45083=CARTESIAN_POINT('',(-0.0183108232868112,-0.00893197079241942,0.0389056616549338));
#45084=CARTESIAN_POINT('',(-0.0202116856337268,-0.0025595719846472,0.0387475172463442));
#45085=CARTESIAN_POINT('',(-0.0203539376319971,0.000861592423192441,0.0386686313889525));
#45086=CARTESIAN_POINT('',(-0.0189937769587308,0.00736633749442342,0.0385108632498404));
#45087=CARTESIAN_POINT('',(-0.0174926176026702,0.0104438824718023,0.0384319774445165));
#45088=CARTESIAN_POINT('',(-0.0131975320941528,0.0155205924991396,0.0382738330357088));
#45089=CARTESIAN_POINT('',(-0.0104112524037978,0.0175108806750789,0.0381949471785047));
#45090=CARTESIAN_POINT('',(-0.00422176050540625,0.0199299580901202,0.0380371790392355));
#45091=CARTESIAN_POINT('',(-0.000824286670233699,0.020356495355586,0.0379582932338931));
#45092=CARTESIAN_POINT('',(0.00577495389241394,0.0195374909454256,0.0378001488252795));
#45093=CARTESIAN_POINT('',(0.00896510698013095,0.01829349544155,0.0377212629681725));
#45094=CARTESIAN_POINT('',(0.014375608693655,0.014434970243203,0.0375634948285151));
#45095=CARTESIAN_POINT('',(0.0165909334505597,0.0118240128093593,0.0374846090233243));
#45096=CARTESIAN_POINT('',(0.0195147328835605,0.00585139687469778,0.0373264646147958));
#45097=CARTESIAN_POINT('',(0.0202181499040229,0.00250030659957759,0.0372475787575161));
#45098=CARTESIAN_POINT('',(0.0199471858992586,-0.0041395973158831,0.0370898106181184));
#45099=CARTESIAN_POINT('',(0.0189730476548394,-0.00742225130017299,0.0370109248128424));
#45100=CARTESIAN_POINT('',(0.0155721405214547,-0.0131366694593094,0.036852780404231));
#45101=CARTESIAN_POINT('',(0.0131514527210815,-0.0155584192627295,0.0367738945469489));
#45102=CARTESIAN_POINT('',(0.00744454448079525,-0.0189632604976578,0.0366161264076841));
#45103=CARTESIAN_POINT('',(0.00416361348869007,-0.0199431861661279,0.0365372406017529));
#45104=CARTESIAN_POINT('',(-0.00248042573380237,-0.0202215512025244,0.0363790961936408));
#45105=CARTESIAN_POINT('',(-0.00583182421418022,-0.0195196041217457,0.0363002103375919));
#45106=CARTESIAN_POINT('',(-0.0118036261064655,-0.0166042434939482,0.0361424421919664));
#45107=CARTESIAN_POINT('',(-0.0144184862761918,-0.0143935265254053,0.0360635564290704));
#45108=CARTESIAN_POINT('',(-0.0182854690326266,-0.00898361096526036,0.0359054119822515));
#45109=CARTESIAN_POINT('',(-0.0195308638237847,-0.00579400387153972,0.0358265260789878));
#45110=CARTESIAN_POINT('',(-0.0203564882148241,0.000799940324915589,0.0356687582293281));
#45111=CARTESIAN_POINT('',(-0.0199359375067954,0.00419815773277999,0.0355898706870897));
#45112=CARTESIAN_POINT('',(-0.0175219871768453,0.0103944117617503,0.0354317280021644));
#45113=CARTESIAN_POINT('',(-0.0155328938191153,0.0131815721981596,0.0353528424204919));
#45114=CARTESIAN_POINT('',(-0.0104642419482611,0.0174792590663091,0.0351950672837447));
#45115=CARTESIAN_POINT('',(-0.00738961226246486,0.0189860828077318,0.0351162210357799));
#45116=CARTESIAN_POINT('',(-0.000881364410376992,0.0203538577683945,0.0349580296493947));
#45117=CARTESIAN_POINT('',(0.00253857652463648,0.0202137634662172,0.0348791818673028));
#45118=CARTESIAN_POINT('',(0.00890865369405714,0.0183218706412125,0.0347214667192783));
#45119=CARTESIAN_POINT('',(0.0118621239181345,0.0165610351729331,0.034642158413343));
#45120=CARTESIAN_POINT('',(0.0144662895113594,0.0139596614511138,0.0345546329568948));
#45121=CARTESIAN_POINT('',(0.0147159584881365,0.0136955527308699,0.034545753344709));
#45122=CARTESIAN_POINT('',(0.0149583820325668,0.0134323390934634,0.0345367687330064));
#45123=CARTESIAN_POINT('',(0.0134243968563088,0.014965926637851,0.0440266469880068));
#45124=CARTESIAN_POINT('',(0.013687606574829,0.0147235066023048,0.04401766250827));
#45125=CARTESIAN_POINT('',(0.0139524570657552,0.0144732354661768,0.0440087576139998));
#45126=CARTESIAN_POINT('',(0.0165606827243585,0.0118650105264396,0.0439210357331533));
#45127=CARTESIAN_POINT('',(0.0183169785555386,0.00891864534677705,0.0438419455335554));
#45128=CARTESIAN_POINT('',(0.0202123964059005,0.00254961458525535,0.0436842303191043));
#45129=CARTESIAN_POINT('',(0.0203543744478548,-0.000870260450086682,0.0436053826318688));
#45130=CARTESIAN_POINT('',(0.0189900756022342,-0.00737923951972287,0.0434471912128856));
#45131=CARTESIAN_POINT('',(0.017484961083932,-0.0104546923800447,0.0433683449407809));
#45132=CARTESIAN_POINT('',(0.0131900644680276,-0.015525710760186,0.0432105698130354));
#45133=CARTESIAN_POINT('',(0.0104039896779972,-0.0175163459681026,0.0431316842509498));
#45134=CARTESIAN_POINT('',(0.00420902850051582,-0.0199336166445472,0.0429735415663171));
#45135=CARTESIAN_POINT('',(0.000811053872307399,-0.020356036240556,0.042894653998026));
#45136=CARTESIAN_POINT('',(-0.00578334574047468,-0.019534045015475,0.0427368861494216));
#45137=CARTESIAN_POINT('',(-0.00897364968385085,-0.0182904018976007,0.0426580002725041));
#45138=CARTESIAN_POINT('',(-0.0143856374953915,-0.0144263171073726,0.0424998558240156));
#45139=CARTESIAN_POINT('',(-0.0165977866640469,-0.0118126828312217,0.0424209700357734));
#45140=CARTESIAN_POINT('',(-0.0195164378422495,-0.0058424867825746,0.0422632018905156));
#45141=CARTESIAN_POINT('',(-0.0202202325281431,-0.00249146300533311,0.0421843160611639));
#45142=CARTESIAN_POINT('',(-0.0199454269988205,0.0041527259998003,0.0420261716512487));
#45143=CARTESIAN_POINT('',(-0.0189673109311248,0.00743418547945166,0.0419472858197865));
#45144=CARTESIAN_POINT('',(-0.0155656138172359,0.0131429701460771,0.041789517681426));
#45145=CARTESIAN_POINT('',(-0.0131451882465153,0.0155649997561152,0.0417106318506291));
#45146=CARTESIAN_POINT('',(-0.00743259156012253,0.0189689687126589,0.0415524874401043));
#45147=CARTESIAN_POINT('',(-0.00415048490179366,0.0199449109496952,0.0414736016091979));
#45148=CARTESIAN_POINT('',(0.00248927022391019,0.020219533415104,0.0413158334710133));
#45149=CARTESIAN_POINT('',(0.00584075953030216,0.0195179588982117,0.0412369476400729));
#45150=CARTESIAN_POINT('',(0.0118149424696186,0.0165973589996381,0.0410788032296136));
#45151=CARTESIAN_POINT('',(0.0144271107866775,0.0143834791361427,0.0409999173987475));
#45152=CARTESIAN_POINT('',(0.0182886173452566,0.00897510297271117,0.0408421492604103));
#45153=CARTESIAN_POINT('',(0.0195343735808227,0.00578562358327755,0.0407632634295357));
#45154=CARTESIAN_POINT('',(0.020356913604267,-0.000813178843569358,0.0406051190190981));
#45155=CARTESIAN_POINT('',(0.0199322482453678,-0.0042108761078978,0.0405262331883193));
#45156=CARTESIAN_POINT('',(0.0175165809193028,-0.0104017013353189,0.0403684650497858));
#45157=CARTESIAN_POINT('',(0.0155278197699022,-0.0131890865732395,0.0402895792190312));
#45158=CARTESIAN_POINT('',(0.0104534103322118,-0.0174868923411122,0.04013143480855));
#45159=CARTESIAN_POINT('',(0.00737670214342564,-0.0189897409987214,0.0400525489777058));
#45160=CARTESIAN_POINT('',(0.000872705995556211,-0.0203534857461097,0.0398947808393469));
#45161=CARTESIAN_POINT('',(-0.00254854873523769,-0.0202131168004107,0.0398158950085049));
#45162=CARTESIAN_POINT('',(-0.00892196654963962,-0.0183156682709116,0.0396577505980237));
#45163=CARTESIAN_POINT('',(-0.0118629009446791,-0.0165619316170496,0.0395788647674302));
#45164=CARTESIAN_POINT('',(-0.0165619310455589,-0.0118629017450905,0.0394210966285696));
#45165=CARTESIAN_POINT('',(-0.0183156678431523,-0.00892196743450048,0.0393422107979038));
#45166=CARTESIAN_POINT('',(-0.0202131166745193,-0.00254854971005675,0.0391840663875722));
#45167=CARTESIAN_POINT('',(-0.0203534857867463,0.000872705012919857,0.0391051805565894));
#45168=CARTESIAN_POINT('',(-0.0189897413562358,0.00737670122719252,0.0389474124183581));
#45169=CARTESIAN_POINT('',(-0.0174868928479001,0.0104534094901412,0.0388685265874864));
#45170=CARTESIAN_POINT('',(-0.0131890873204951,0.0155278191313265,0.0387103821769368));
#45171=CARTESIAN_POINT('',(-0.0104017021802572,0.017516580415848,0.0386314963461393));
#45172=CARTESIAN_POINT('',(-0.00421087707039726,0.0199322480435583,0.0384737282077554));
#45173=CARTESIAN_POINT('',(-0.000813179825758113,0.0203569135679558,0.038394842376862));
#45174=CARTESIAN_POINT('',(0.00578562264002206,0.0195343738571403,0.0382366979665085));
#45175=CARTESIAN_POINT('',(0.00897510208915741,0.0182886177771876,0.0381578121358093));
#45176=CARTESIAN_POINT('',(0.0143834784406977,0.01442711148213,0.0380000439970328));
#45177=CARTESIAN_POINT('',(0.0165973584320769,0.0118149432719776,0.0379211581662922));
#45178=CARTESIAN_POINT('',(0.0195179586135799,0.00584076047113161,0.0377630137560259));
#45179=CARTESIAN_POINT('',(0.0202195332934501,0.002489271199808,0.0376841279251519));
#45180=CARTESIAN_POINT('',(0.0199449111515263,-0.00415048393918659,0.0375263597866371));
#45181=CARTESIAN_POINT('',(0.0189689690739686,-0.00743259064608601,0.0374474739558123));
#45182=CARTESIAN_POINT('',(0.0155650003880389,-0.0131451874936908,0.0372893295454589));
#45183=CARTESIAN_POINT('',(0.0131429708966224,-0.015565613181577,0.0372104437145858));
#45184=CARTESIAN_POINT('',(0.00743418639561038,-0.0189673105736437,0.0370526755762019));
#45185=CARTESIAN_POINT('',(0.00415272696260282,-0.0199454268013481,0.036973789744721));
#45186=CARTESIAN_POINT('',(-0.0024914620294482,-0.0202202326454308,0.0368156453348712));
#45187=CARTESIAN_POINT('',(-0.00584248583997558,-0.0195164381228754,0.0367367595052236));
#45188=CARTESIAN_POINT('',(-0.0118126820307963,-0.0165977872355334,0.0365789913604876));
#45189=CARTESIAN_POINT('',(-0.0144263164154719,-0.0143856381934081,0.0365001055720521));
#45190=CARTESIAN_POINT('',(-0.018290401462013,-0.00897365056498236,0.0363419611234327));
#45191=CARTESIAN_POINT('',(-0.0195340447348365,-0.00578334668312191,0.0362630752468074));
#45192=CARTESIAN_POINT('',(-0.0203560362812166,0.000811052889691331,0.0361053073977451));
#45193=CARTESIAN_POINT('',(-0.0199336168504544,0.0042090275394474,0.0360264198296735));
#45194=CARTESIAN_POINT('',(-0.0175163464674805,0.0104039888314446,0.0358682771450641));
#45195=CARTESIAN_POINT('',(-0.0155257113958446,0.0131900637175812,0.035789391583042));
#45196=CARTESIAN_POINT('',(-0.0104546932247947,0.0174849605803254,0.0356316164551422));
#45197=CARTESIAN_POINT('',(-0.00737924043715088,0.01899007524981,0.0355527701832371));
#45198=CARTESIAN_POINT('',(-0.000870261431598303,0.0203543744029426,0.0353945787640066));
#45199=CARTESIAN_POINT('',(0.00254961361012549,0.02021239652742,0.0353157310768663));
#45200=CARTESIAN_POINT('',(0.00891864446487162,0.0183169789881492,0.035158015862421));
#45201=CARTESIAN_POINT('',(0.0118711468820354,0.0165545454869355,0.0350787075431251));
#45202=CARTESIAN_POINT('',(0.0144739176610643,0.0139517749677388,0.034991182120757));
#45203=CARTESIAN_POINT('',(0.014723509957734,0.0136876030217121,0.0349823026500466));
#45204=CARTESIAN_POINT('',(0.0149659317995843,0.0134243912328982,0.0349733181014439));
#45205=CARTESIAN_POINT('',(0.0134323507348915,0.014958390148285,0.0444630144047823));
#45206=CARTESIAN_POINT('',(0.0136955623892009,0.0147159683298484,0.0444540298589685));
#45207=CARTESIAN_POINT('',(0.0139603501643897,0.0144656208027388,0.0444451248216824));
#45208=CARTESIAN_POINT('',(0.0165671823597683,0.0118560003406502,0.0443574029042448));
#45209=CARTESIAN_POINT('',(0.0183218821358191,0.00890866553410848,0.0442783127187353));
#45210=CARTESIAN_POINT('',(0.0202137781832282,0.00253858404797499,0.044120597572689));
#45211=CARTESIAN_POINT('',(0.0203538735514792,-0.000881359440271408,0.0440417497916532));
#45212=CARTESIAN_POINT('',(0.0189860992971344,-0.0073896126699635,0.0438835584015622));
#45213=CARTESIAN_POINT('',(0.0174792752695404,-0.0104642451029217,0.043804712154686));
#45214=CARTESIAN_POINT('',(0.0131815865514812,-0.0155329020177859,0.0436469370197732));
#45215=CARTESIAN_POINT('',(0.0103944245524534,-0.0175219976723892,0.0435680514389131));
#45216=CARTESIAN_POINT('',(0.00419816641268413,-0.0199359515386241,0.0434099087505035));
#45217=CARTESIAN_POINT('',(0.000799946546492838,-0.0203565035039386,0.0433310212088694));
#45218=CARTESIAN_POINT('',(-0.00579400288494992,-0.0195308803243074,0.0431732533614397));
#45219=CARTESIAN_POINT('',(-0.00898361275583876,-0.0182854854811773,0.0430943674587492));
#45220=CARTESIAN_POINT('',(-0.0143935335247905,-0.014418501217132,0.042936223008582));
#45221=CARTESIAN_POINT('',(-0.0166042528904406,-0.0118036396773023,0.0428573372467254));
#45222=CARTESIAN_POINT('',(-0.0195196173960083,-0.00583183406508102,0.0426995691023438));
#45223=CARTESIAN_POINT('',(-0.0202215659519979,-0.00248043323127719,0.0426206832474583));
#45224=CARTESIAN_POINT('',(-0.0199432025025457,0.0041636111764046,0.0424625388358018));
#45225=CARTESIAN_POINT('',(-0.0189632769981644,0.0074445449248028,0.0423836530307362));
#45226=CARTESIAN_POINT('',(-0.0155584347698434,0.0131514584457935,0.0422258848932583));
#45227=CARTESIAN_POINT('',(-0.013136683803135,0.0155721487684907,0.042146999036921));
#45228=CARTESIAN_POINT('',(-0.0074222621711207,0.0189730600664392,0.0419888546246593));
#45229=CARTESIAN_POINT('',(-0.0041396059692075,0.0199471999558189,0.0419099688201486));
#45230=CARTESIAN_POINT('',(0.00250030291063802,0.0202181660171394,0.0417522006828445));
#45231=CARTESIAN_POINT('',(0.00585139593345808,0.0195147494024473,0.0416733148263639));
#45232=CARTESIAN_POINT('',(0.0118240172541425,0.0165909493398389,0.0415151704141697));
#45233=CARTESIAN_POINT('',(0.0144349772779972,0.0143756236261366,0.0414362846096961));
#45234=CARTESIAN_POINT('',(0.0182935069132192,0.00896511888142835,0.0412785164722437));
#45235=CARTESIAN_POINT('',(0.0195375042596792,0.0057749637153101,0.0411996306158288));
#45236=CARTESIAN_POINT('',(0.0203565110886193,-0.00082428170059236,0.0410414862036521));
#45237=CARTESIAN_POINT('',(0.0199299744386224,-0.00422175822745308,0.0409626003992711));
#45238=CARTESIAN_POINT('',(0.017510896912993,-0.0104112554980561,0.040804832261616));
#45239=CARTESIAN_POINT('',(0.0155206080048174,-0.0131975378677864,0.0407259464053232));
#45240=CARTESIAN_POINT('',(0.0104438952373011,-0.0174926280557002,0.040567801993105));
#45241=CARTESIAN_POINT('',(0.00736634834331694,-0.0189937893992192,0.0404889161886566));
#45242=CARTESIAN_POINT('',(0.000861598713996071,-0.0203539529182404,0.0403311480511781));
#45243=CARTESIAN_POINT('',(-0.002559568337358,-0.0202117017724119,0.0402522621948001));
#45244=CARTESIAN_POINT('',(-0.00893197256125958,-0.0183108396909511,0.0400941177825755));
#45245=CARTESIAN_POINT('',(-0.0118719531216823,-0.0165554780277981,0.0400152319783788));
#45246=CARTESIAN_POINT('',(-0.0165683972536806,-0.0118538586203137,0.039857463840403));
#45247=CARTESIAN_POINT('',(-0.0183205103802491,-0.0089119682460497,0.039778577984198));
#45248=CARTESIAN_POINT('',(-0.0202145471188442,-0.00253753202962592,0.039620433572125));
#45249=CARTESIAN_POINT('',(-0.0203530341298277,0.000883812970843685,0.0395415477675402));
#45250=CARTESIAN_POINT('',(-0.0189857074358077,0.00738706064028674,0.0393837796301893));
#45251=CARTESIAN_POINT('',(-0.0174811704792471,0.0104629325375536,0.0393048937737806));
#45252=CARTESIAN_POINT('',(-0.013180646066677,0.0155350427514035,0.0391467493614896));
#45253=CARTESIAN_POINT('',(-0.0103921559373152,0.0175222777809261,0.0390678635570879));
#45254=CARTESIAN_POINT('',(-0.00419999817167859,0.019934537042528,0.0389100954195888));
#45255=CARTESIAN_POINT('',(-0.000802077610691454,0.0203573316060118,0.0388312095631551));
#45256=CARTESIAN_POINT('',(0.00579628694082303,0.0195312580680787,0.0386730651510625));
#45257=CARTESIAN_POINT('',(0.0089850930321539,0.0182837421458691,0.0385941793467601));
#45258=CARTESIAN_POINT('',(0.0143913449075759,0.0144192559966424,0.0384364112088641));
#45259=CARTESIAN_POINT('',(0.0166037807356177,0.0118058775148413,0.0383575253525841));
#45260=CARTESIAN_POINT('',(0.019521182999093,0.00583012850089137,0.0381993809405809));
#45261=CARTESIAN_POINT('',(0.020220916106271,0.00247824039966869,0.0381204951361016));
#45262=CARTESIAN_POINT('',(0.0199426373519245,-0.00416136602487085,0.0379627269984695));
#45263=CARTESIAN_POINT('',(0.0189648921930783,-0.00744292568248877,0.0378838411421065));
#45264=CARTESIAN_POINT('',(0.0155578632306798,-0.0131537019776971,0.0377256967300117));
#45265=CARTESIAN_POINT('',(0.0131344926074458,-0.0155728041019498,0.0376468109255366));
#45266=CARTESIAN_POINT('',(0.00742383262774643,-0.0189713589615301,0.0374890427880331));
#45267=CARTESIAN_POINT('',(0.00414184497409428,-0.0199476665026562,0.0374101569310133));
#45268=CARTESIAN_POINT('',(-0.00250249372509033,-0.020218914637921,0.0372520125194265));
#45269=CARTESIAN_POINT('',(-0.00585314302193221,-0.0195132734436152,0.0371731267161692));
#45270=CARTESIAN_POINT('',(-0.0118217341805558,-0.0165913336681314,0.0370153585723223));
#45271=CARTESIAN_POINT('',(-0.0144341432910962,-0.0143777531493217,0.036936472758358));
#45272=CARTESIAN_POINT('',(-0.0182953318355289,-0.00896369431626748,0.0367783283079389));
#45273=CARTESIAN_POINT('',(-0.0195372243200628,-0.00577269393669329,0.0366994424579409));
#45274=CARTESIAN_POINT('',(-0.0203555845359782,0.000822160822673886,0.0365416746094756));
#45275=CARTESIAN_POINT('',(-0.019931297161379,0.00421989281550488,0.0364627870155816));
#45276=CARTESIAN_POINT('',(-0.017510708109202,0.0104135619093506,0.0363046443312881));
#45277=CARTESIAN_POINT('',(-0.0155185319662571,0.0131985516976792,0.036225758788908));
#45278=CARTESIAN_POINT('',(-0.0104451484813017,0.0174906597179114,0.0360679836698519));
#45279=CARTESIAN_POINT('',(-0.00736887293488479,0.0189940660278109,0.0359891373740166));
#45280=CARTESIAN_POINT('',(-0.000859163080617291,0.0203548908221539,0.0358309459219546));
#45281=CARTESIAN_POINT('',(0.0025606460952816,0.0202110301583723,0.0357520983297262));
#45282=CARTESIAN_POINT('',(0.00892863107146433,0.0183120893739606,0.0355943830488878));
#45283=CARTESIAN_POINT('',(0.011880166085103,0.0165480585058836,0.0355150747162368));
#45284=CARTESIAN_POINT('',(0.0144815426313042,0.0139438917715042,0.0354275493279347));
#45285=CARTESIAN_POINT('',(0.0147310582798273,0.0136796566260476,0.0354186699986407));
#45286=CARTESIAN_POINT('',(0.0149734784198071,0.0134164466850558,0.0354096855131117));
#45287=CARTESIAN_POINT('',(0.0132774325567157,0.0147734032199086,0.0449158584910965));
#45288=CARTESIAN_POINT('',(0.0135391077187239,0.0145323965335079,0.0449069263923718));
#45289=CARTESIAN_POINT('',(0.0138014039135308,0.0142842302640092,0.0448980501159253));
#45290=CARTESIAN_POINT('',(0.0163749972709665,0.011704953790514,0.0448103694939715));
#45291=CARTESIAN_POINT('',(0.0181074530777823,0.00879152021484105,0.0447312665590919));
#45292=CARTESIAN_POINT('',(0.0199730255068591,0.00249651795811219,0.0445735198851828));
#45293=CARTESIAN_POINT('',(0.0201093666845512,-0.000882833009343425,0.0444946545146255));
#45294=CARTESIAN_POINT('',(0.0187544866881982,-0.00731160469610085,0.0443365250922151));
#45295=CARTESIAN_POINT('',(0.0172639601138449,-0.0103487409519681,0.0442576584501176));
#45296=CARTESIAN_POINT('',(0.0130146079248891,-0.0153544536244878,0.0440998569695397));
#45297=CARTESIAN_POINT('',(0.0102595012097063,-0.0173180914728919,0.0440209577525291));
#45298=CARTESIAN_POINT('',(0.00413677952879929,-0.0196993834358412,0.0438628694096752));
#45299=CARTESIAN_POINT('',(0.000778873719066263,-0.0201130760903658,0.0437839687687258));
#45300=CARTESIAN_POINT('',(-0.00573593586137178,-0.0192934896015891,0.0436261731415959));
#45301=CARTESIAN_POINT('',(-0.00888670629679085,-0.0180610055096835,0.0435472737494208));
#45302=CARTESIAN_POINT('',(-0.0142290621595103,-0.0142377202406875,0.0433891839738936));
#45303=CARTESIAN_POINT('',(-0.0164119892680786,-0.0116528560195468,0.0433102847563008));
#45304=CARTESIAN_POINT('',(-0.0192891222321422,-0.00575060537461488,0.0431524888939648));
#45305=CARTESIAN_POINT('',(-0.0199806360344781,-0.00243878116859957,0.043073589537792));
#45306=CARTESIAN_POINT('',(-0.0197019014047589,0.0041247990854508,0.0429154997933989));
#45307=CARTESIAN_POINT('',(-0.0187318877423047,0.0073660591097996,0.0428366005414287));
#45308=CARTESIAN_POINT('',(-0.0153643639269432,0.0130029235040371,0.042678804684548));
#45309=CARTESIAN_POINT('',(-0.0129700379181249,0.0153932318367515,0.0425999053272683));
#45310=CARTESIAN_POINT('',(-0.0073227751616878,0.0187498226748011,0.0424418155823795));
#45311=CARTESIAN_POINT('',(-0.0040787537352243,0.0197105609554491,0.0423629163308548));
#45312=CARTESIAN_POINT('',(0.00248210112658439,0.019974455500205,0.0422051204741111));
#45313=CARTESIAN_POINT('',(0.00579275933568636,0.0192773807675007,0.0421262211167112));
#45314=CARTESIAN_POINT('',(0.0116915446297296,0.0163855628703383,0.0419681313718886));
#45315=CARTESIAN_POINT('',(0.0142701540567164,0.0141952509103176,0.0418892321203894));
#45316=CARTESIAN_POINT('',(0.0180795252057958,0.00884705978653905,0.0417314362635233));
#45317=CARTESIAN_POINT('',(0.0193067160163676,0.00569422397168671,0.0416525369061795));
#45318=CARTESIAN_POINT('',(0.0201121127633341,-0.000825715811345802,0.0414944471613675));
#45319=CARTESIAN_POINT('',(0.0196888226900121,-0.00418242827643942,0.0414155479099439));
#45320=CARTESIAN_POINT('',(0.0172950248955886,-0.01029668939015,0.0412577520529161));
#45321=CARTESIAN_POINT('',(0.0153267861934022,-0.0130484901409762,0.041178852695677));
#45322=CARTESIAN_POINT('',(0.0103090214339838,-0.0172888103546578,0.0410207629508175));
#45323=CARTESIAN_POINT('',(0.00726737655517426,-0.0187703937948799,0.0409418636993504));
#45324=CARTESIAN_POINT('',(0.000839438816763122,-0.0201105703799344,0.0407840678424572));
#45325=CARTESIAN_POINT('',(-0.00254080105956695,-0.0199679192694803,0.0407051684851519));
#45326=CARTESIAN_POINT('',(-0.00883511219257549,-0.0180864501478478,0.0405470787402899));
#45327=CARTESIAN_POINT('',(-0.0117390662474826,-0.0163504363500681,0.0404681794890089));
#45328=CARTESIAN_POINT('',(-0.0163767658662786,-0.0117021894662202,0.0403103836317459));
#45329=CARTESIAN_POINT('',(-0.0181061591128077,-0.00879434319095104,0.04023148427456));
#45330=CARTESIAN_POINT('',(-0.0199737181150179,-0.00249589083605073,0.0400733945298292));
#45331=CARTESIAN_POINT('',(-0.020108697879637,0.000884711702365825,0.0399944952782453));
#45332=CARTESIAN_POINT('',(-0.0187539226697023,0.00730958843101573,0.0398366994214571));
#45333=CARTESIAN_POINT('',(-0.017265459695178,0.0103478196490916,0.0397578000641271));
#45334=CARTESIAN_POINT('',(-0.0130140644752542,0.015356204356557,0.0395997103192093));
#45335=CARTESIAN_POINT('',(-0.0102577642874015,0.0173182192223741,0.0395208110677819));
#45336=CARTESIAN_POINT('',(-0.00413808105738116,0.0196981213240248,0.0393630152108678));
#45337=CARTESIAN_POINT('',(-0.000780463646085143,0.0201137849862969,0.039284115853516));
#45338=CARTESIAN_POINT('',(0.00573768092622813,0.0192939862131531,0.0391260261087678));
#45339=CARTESIAN_POINT('',(0.00888776731266,0.0180596245087814,0.0390471268574055));
#45340=CARTESIAN_POINT('',(0.0142272910447909,0.0142381139224078,0.0388893310001916));
#45341=CARTESIAN_POINT('',(0.0164117133878414,0.0116545756531483,0.0388104316429529));
#45342=CARTESIAN_POINT('',(0.0192904925041646,0.00574941608770125,0.0386523418982784));
#45343=CARTESIAN_POINT('',(0.0199800602103527,0.00243713750068655,0.0385734426467758));
#45344=CARTESIAN_POINT('',(0.0197012623214353,-0.00412310095417178,0.0384156467897683));
#45345=CARTESIAN_POINT('',(0.0187331764642615,-0.00736488761193141,0.0383367474324733));
#45346=CARTESIAN_POINT('',(0.0153641177626821,-0.0130047211342287,0.0381786576877099));
#45347=CARTESIAN_POINT('',(0.0129683469496416,-0.0153936487746862,0.0380997584362191));
#45348=CARTESIAN_POINT('',(0.00732384723385657,-0.0187483588673528,0.0379419625793142));
#45349=CARTESIAN_POINT('',(0.00408043933965481,-0.0197109990832421,0.0378630632214872));
#45350=CARTESIAN_POINT('',(-0.00248374068359378,-0.0199752326289125,0.0377049734771552));
#45351=CARTESIAN_POINT('',(-0.00579403324945224,-0.0192761931914336,0.0376260742265771));
#45352=CARTESIAN_POINT('',(-0.0116897328046641,-0.0163856597591573,0.0374682783646604));
#45353=CARTESIAN_POINT('',(-0.0142695989494591,-0.0141969015908406,0.0373893790411247));
#45354=CARTESIAN_POINT('',(-0.0180810724819061,-0.00884611231053172,0.0372312892652485));
#45355=CARTESIAN_POINT('',(-0.0193064187306797,-0.0056925080040017,0.0371523899800911));
#45356=CARTESIAN_POINT('',(-0.0201112032241304,0.000824146644046457,0.0369945943514264));
#45357=CARTESIAN_POINT('',(-0.0196898977667719,0.00418105816284977,0.0369156936037029));
#45358=CARTESIAN_POINT('',(-0.0172950832261643,0.0102985033413524,0.0367576052691976));
#45359=CARTESIAN_POINT('',(-0.0153251673105889,0.0130491830686049,0.0366787061305392));
#45360=CARTESIAN_POINT('',(-0.0103098218392397,0.0172871617375925,0.0365209046824581));
#45361=CARTESIAN_POINT('',(-0.00726933690112621,0.018770722967874,0.036442037940343));
#45362=CARTESIAN_POINT('',(-0.00083759659875895,0.0201114398926357,0.0362839083919405));
#45363=CARTESIAN_POINT('',(0.00254148063827732,0.0199674250037726,0.0362050434060442));
#45364=CARTESIAN_POINT('',(0.00883221018549675,0.0180874953282551,0.0360472964574278));
#45365=CARTESIAN_POINT('',(0.0117477586613136,0.0163424685172153,0.0359679780033833));
#45366=CARTESIAN_POINT('',(0.0143159619590558,0.0137685786180237,0.0358804910529425));
#45367=CARTESIAN_POINT('',(0.014563145781723,0.0135066960806843,0.0358716402000459));
#45368=CARTESIAN_POINT('',(0.0148041471746711,0.0132450265576457,0.0358627082955947));
#45369=CARTESIAN_POINT('',(0.0129138508916869,0.0143725930875827,0.0450790488739469));
#45370=CARTESIAN_POINT('',(0.0131720706341788,0.0141347688934417,0.0450702347235489));
#45371=CARTESIAN_POINT('',(0.0134288924071795,0.0138916521969391,0.0450614233363915));
#45372=CARTESIAN_POINT('',(0.0159305442659458,0.0113832729646018,0.0449738355536919));
#45373=CARTESIAN_POINT('',(0.0176161543656036,0.00854789414688023,0.0448947039506003));
#45374=CARTESIAN_POINT('',(0.0194294856532803,0.00242360909110657,0.0447368863175001));
#45375=CARTESIAN_POINT('',(0.0195610782100481,-0.000864419420761024,0.0446579816168119));
#45376=CARTESIAN_POINT('',(0.0182419666895939,-0.00711606163363783,0.0444999913442412));
#45377=CARTESIAN_POINT('',(0.0167913972841028,-0.0100705709602299,0.0444210788362177));
#45378=CARTESIAN_POINT('',(0.0126560949175306,-0.0149395055174694,0.0442632181858345));
#45379=CARTESIAN_POINT('',(0.00997512630113625,-0.0168489673916814,0.0441842883728412));
#45380=CARTESIAN_POINT('',(0.00402013804374216,-0.0191633784369803,0.0440263221211558));
#45381=CARTESIAN_POINT('',(0.000753275155927111,-0.0195653175752822,0.0439473920012669));
#45382=CARTESIAN_POINT('',(-0.00558463299752592,-0.0187664008856396,0.0437895339665373));
#45383=CARTESIAN_POINT('',(-0.00864951164828749,-0.0175663485840429,0.043710604321552));
#45384=CARTESIAN_POINT('',(-0.0138441331044444,-0.0138469053737105,0.0435526373723547));
#45385=CARTESIAN_POINT('',(-0.0159674252333963,-0.0113318302923382,0.0434737078756761));
#45386=CARTESIAN_POINT('',(-0.018765106459829,-0.00558898075670583,0.0433158497450324));
#45387=CARTESIAN_POINT('',(-0.0194367926615482,-0.00236680089305438,0.0432369201090668));
#45388=CARTESIAN_POINT('',(-0.0191641880564002,0.00401630485958065,0.043078953174557));
#45389=CARTESIAN_POINT('',(-0.0182199822859882,0.00716946943245308,0.0430000236633192));
#45390=CARTESIAN_POINT('',(-0.0149424477523284,0.0126526353535143,0.0428421655348627));
#45391=CARTESIAN_POINT('',(-0.0126123243137451,0.0149773138742785,0.0427632358985783));
#45392=CARTESIAN_POINT('',(-0.00711950156511704,0.0182403263678245,0.0426052689638103));
#45393=CARTESIAN_POINT('',(-0.00396334627656238,0.0191744865054583,0.0425263394527732));
#45394=CARTESIAN_POINT('',(0.00241961790374605,0.0194296519634247,0.0423684813243768));
#45395=CARTESIAN_POINT('',(0.00564021755686893,0.018750429365584,0.0422895516880225));
#45396=CARTESIAN_POINT('',(0.0113761915199589,0.015936720962703,0.0421315847533152));
#45397=CARTESIAN_POINT('',(0.0138844923942741,0.0138054307215434,0.042052655242283));
#45398=CARTESIAN_POINT('',(0.0175892588639255,0.00860138935517418,0.0418947971138141));
#45399=CARTESIAN_POINT('',(0.0187821375220497,0.00553371173675391,0.041815867477496));
#45400=CARTESIAN_POINT('',(0.0195638755616741,-0.000807206013704218,0.041657900542789));
#45401=CARTESIAN_POINT('',(0.0191515413594767,-0.0040727766949323,0.0415789710317868));
#45402=CARTESIAN_POINT('',(0.0168212075730868,-0.0100206238332644,0.0414211129032577));
#45403=CARTESIAN_POINT('',(0.0149054934897077,-0.012697122481573,0.0413421832670016));
#45404=CARTESIAN_POINT('',(0.0100246598884266,-0.0168197206475598,0.0411842163322308));
#45405=CARTESIAN_POINT('',(0.00706530814937353,-0.0182606261450326,0.0411052868212415));
#45406=CARTESIAN_POINT('',(0.000811398134958812,-0.0195629128528423,0.0409474286927504));
#45407=CARTESIAN_POINT('',(-0.00247707310188533,-0.0194230472462728,0.0408684990564665));
#45408=CARTESIAN_POINT('',(-0.00859793703807817,-0.0175918244429124,0.0407105321217132));
#45409=CARTESIAN_POINT('',(-0.0114228268016637,-0.0159024549772322,0.0406316026107603));
#45410=CARTESIAN_POINT('',(-0.0159336221423258,-0.0113791744716903,0.0404737444821789));
#45411=CARTESIAN_POINT('',(-0.0176151546309675,-0.0085496773513497,0.0403948148459005));
#45412=CARTESIAN_POINT('',(-0.0194299115416473,-0.00242391130659293,0.0402368479112266));
#45413=CARTESIAN_POINT('',(-0.0195606963090452,0.00086498922598336,0.0401579184001611));
#45414=CARTESIAN_POINT('',(-0.0182411287006575,0.0071152758165584,0.0400000602717256));
#45415=CARTESIAN_POINT('',(-0.0167920796589088,0.0100705866865345,0.0399211306354328));
#45416=CARTESIAN_POINT('',(-0.0126563716223977,0.014940316793741,0.0397631637006416));
#45417=CARTESIAN_POINT('',(-0.00997454683381245,0.0168486635053003,0.0396842341896759));
#45418=CARTESIAN_POINT('',(-0.0040202813476444,0.019162548476316,0.0395263760611581));
#45419=CARTESIAN_POINT('',(-0.00075363945007261,0.0195658550302225,0.0394474464248561));
#45420=CARTESIAN_POINT('',(0.00558515324695027,0.0187670688107491,0.0392894794901657));
#45421=CARTESIAN_POINT('',(0.00864957627121354,0.0175657017159631,0.0392105499791872));
#45422=CARTESIAN_POINT('',(0.0138433577443138,0.0138465653716977,0.0390526918505942));
#45423=CARTESIAN_POINT('',(0.0159676762407863,0.011332430055188,0.0389737622143119));
#45424=CARTESIAN_POINT('',(0.0187659501848109,0.00558891064506963,0.0388157952796574));
#45425=CARTESIAN_POINT('',(0.0194362864539758,0.00236639289421834,0.0387368657686242));
#45426=CARTESIAN_POINT('',(0.0191634793886099,-0.00401584162374749,0.0385790076401043));
#45427=CARTESIAN_POINT('',(0.0182206216688099,-0.00716935153876095,0.0385000780038236));
#45428=CARTESIAN_POINT('',(0.0149428505310971,-0.0126533800442663,0.0383421110690947));
#45429=CARTESIAN_POINT('',(0.0126117058821609,-0.0149771132462627,0.0382631815580843));
#45430=CARTESIAN_POINT('',(0.00711950176515704,-0.0182394797302009,0.0381053234296125));
#45431=CARTESIAN_POINT('',(0.00396379468394748,-0.0191749572951896,0.0380263937930821));
#45432=CARTESIAN_POINT('',(-0.002420021036381,-0.0194303964622404,0.0378684268586038));
#45433=CARTESIAN_POINT('',(-0.00564038784424458,-0.0187498019041688,0.0377894973478354));
#45434=CARTESIAN_POINT('',(-0.0113754826268754,-0.0159362580769357,0.0376316392173264));
#45435=CARTESIAN_POINT('',(-0.0138846413112407,-0.0138060635195378,0.0375527095953789));
#45436=CARTESIAN_POINT('',(-0.0175901025577762,-0.00860145913332057,0.0373947426458515));
#45437=CARTESIAN_POINT('',(-0.0187817055459195,-0.00553322593065883,0.0373158131273598));
#45438=CARTESIAN_POINT('',(-0.0195631005983065,0.000806866293556,0.0371579550911043));
#45439=CARTESIAN_POINT('',(-0.0191521499202236,0.00407255220458082,0.0370790248446952));
#45440=CARTESIAN_POINT('',(-0.01682173172892,0.0100212944823637,0.0369210586028574));
#45441=CARTESIAN_POINT('',(-0.0149048382880035,0.0126970227189995,0.0368421288825937));
#45442=CARTESIAN_POINT('',(-0.0100245010513865,0.0168188618539805,0.0366842682707503));
#45443=CARTESIAN_POINT('',(-0.00706602777302647,0.0182611861391709,0.0366053556442268));
#45444=CARTESIAN_POINT('',(-0.000810871506560531,0.0195635323386266,0.0364473652226556));
#45445=CARTESIAN_POINT('',(0.00247683298098486,0.0194228561427848,0.0363684609772384));
#45446=CARTESIAN_POINT('',(0.00859606028164421,0.0175925296827086,0.0362106430189561));
#45447=CARTESIAN_POINT('',(0.0114326608091759,0.0158933207565089,0.0361313018539961));
#45448=CARTESIAN_POINT('',(0.0139290714571154,0.0133901785987586,0.0360439011850484));
#45449=CARTESIAN_POINT('',(0.0141711670058611,0.0131337047426488,0.0360351140257455));
#45450=CARTESIAN_POINT('',(0.0144089846063591,0.012875492052252,0.0360263001178339));
#45451=CARTESIAN_POINT('',(0.,0.,0.0334));
#45452=CARTESIAN_POINT('',(0.,0.,0.0487));
#45453=CARTESIAN_POINT('',(0.,0.,0.0499));
#45454=CARTESIAN_POINT('',(0.,0.,0.048900001));
#45455=CARTESIAN_POINT('',(0.,0.,0.));
#45456=CARTESIAN_POINT('',(0.,0.,-0.0300923697749146));
#45457=CARTESIAN_POINT('',(0.,0.,0.00891153628714572));
#45458=CARTESIAN_POINT('',(-0.01,0.,0.00891153628714572));
#45459=CARTESIAN_POINT('',(0.,0.,0.0103398219728543));
#45460=CARTESIAN_POINT('',(-0.01,0.,0.0103398219728543));
#45461=CARTESIAN_POINT('',(0.,0.,0.00962567913));
#45462=CARTESIAN_POINT('',(6.60748485622387E-18,-2.3203745570722E-19,0.0263648045536099));
#45463=MECHANICAL_DESIGN_GEOMETRIC_PRESENTATION_REPRESENTATION('',(#13529,
#13530,#13531,#13532,#13533,#13534,#13535,#13536,#13537,#13538,#13539,#13540,
#13541,#13542,#13543,#13544,#13545,#13546,#13547,#13548,#13549,#13550,#13551,
#13552,#13553,#13554,#13555),#45464);
#45464=(
GEOMETRIC_REPRESENTATION_CONTEXT(3)
GLOBAL_UNCERTAINTY_ASSIGNED_CONTEXT((#45492))
GLOBAL_UNIT_ASSIGNED_CONTEXT((#45522,#45521,#45520))
REPRESENTATION_CONTEXT('MAS-690','TOP_LEVEL_ASSEMBLY_PART')
);
#45465=(
GEOMETRIC_REPRESENTATION_CONTEXT(3)
GLOBAL_UNCERTAINTY_ASSIGNED_CONTEXT((#45493))
GLOBAL_UNIT_ASSIGNED_CONTEXT((#45522,#45521,#45520))
REPRESENTATION_CONTEXT('Top_acces_nozzle_supporter','COMPONENT_PART')
);
#45466=(
GEOMETRIC_REPRESENTATION_CONTEXT(3)
GLOBAL_UNCERTAINTY_ASSIGNED_CONTEXT((#45494))
GLOBAL_UNIT_ASSIGNED_CONTEXT((#45522,#45521,#45520))
REPRESENTATION_CONTEXT('piston','COMPONENT_PART')
);
#45467=(
GEOMETRIC_REPRESENTATION_CONTEXT(3)
GLOBAL_UNCERTAINTY_ASSIGNED_CONTEXT((#45495))
GLOBAL_UNIT_ASSIGNED_CONTEXT((#45522,#45521,#45520))
REPRESENTATION_CONTEXT('75632s_.prt','COMPONENT_PART')
);
#45468=(
GEOMETRIC_REPRESENTATION_CONTEXT(3)
GLOBAL_UNCERTAINTY_ASSIGNED_CONTEXT((#45496))
GLOBAL_UNIT_ASSIGNED_CONTEXT((#45522,#45521,#45520))
REPRESENTATION_CONTEXT('refill_cap','COMPONENT_PART')
);
#45469=(
GEOMETRIC_REPRESENTATION_CONTEXT(3)
GLOBAL_UNCERTAINTY_ASSIGNED_CONTEXT((#45497))
GLOBAL_UNIT_ASSIGNED_CONTEXT((#45522,#45521,#45520))
REPRESENTATION_CONTEXT('spring','COMPONENT_PART')
);
#45470=(
GEOMETRIC_REPRESENTATION_CONTEXT(3)
GLOBAL_UNCERTAINTY_ASSIGNED_CONTEXT((#45498))
GLOBAL_UNIT_ASSIGNED_CONTEXT((#45522,#45521,#45520))
REPRESENTATION_CONTEXT('floating_ring_bottom_connector',
'COMPONENT_PART')
);
#45471=(
GEOMETRIC_REPRESENTATION_CONTEXT(3)
GLOBAL_UNCERTAINTY_ASSIGNED_CONTEXT((#45499))
GLOBAL_UNIT_ASSIGNED_CONTEXT((#45522,#45521,#45520))
REPRESENTATION_CONTEXT(
'binding head screw_ai_CR-BHMS 0.099-48x0.25x0.25-N','COMPONENT_PART')
);
#45472=(
GEOMETRIC_REPRESENTATION_CONTEXT(3)
GLOBAL_UNCERTAINTY_ASSIGNED_CONTEXT((#45500))
GLOBAL_UNIT_ASSIGNED_CONTEXT((#45522,#45521,#45520))
REPRESENTATION_CONTEXT('Floating_ring_guide','COMPONENT_PART')
);
#45473=(
GEOMETRIC_REPRESENTATION_CONTEXT(3)
GLOBAL_UNCERTAINTY_ASSIGNED_CONTEXT((#45501))
GLOBAL_UNIT_ASSIGNED_CONTEXT((#45522,#45521,#45520))
REPRESENTATION_CONTEXT('Bottle_Nech_Seal','COMPONENT_PART')
);
#45474=(
GEOMETRIC_REPRESENTATION_CONTEXT(3)
GLOBAL_UNCERTAINTY_ASSIGNED_CONTEXT((#45502))
GLOBAL_UNIT_ASSIGNED_CONTEXT((#45522,#45521,#45520))
REPRESENTATION_CONTEXT('refill_cap','COMPONENT_PART')
);
#45475=(
GEOMETRIC_REPRESENTATION_CONTEXT(3)
GLOBAL_UNCERTAINTY_ASSIGNED_CONTEXT((#45503))
GLOBAL_UNIT_ASSIGNED_CONTEXT((#45522,#45521,#45520))
REPRESENTATION_CONTEXT('main_housing','COMPONENT_PART')
);
#45476=(
GEOMETRIC_REPRESENTATION_CONTEXT(3)
GLOBAL_UNCERTAINTY_ASSIGNED_CONTEXT((#45504))
GLOBAL_UNIT_ASSIGNED_CONTEXT((#45522,#45521,#45520))
REPRESENTATION_CONTEXT('Nozzle cap','COMPONENT_PART')
);
#45477=(
GEOMETRIC_REPRESENTATION_CONTEXT(3)
GLOBAL_UNCERTAINTY_ASSIGNED_CONTEXT((#45505))
GLOBAL_UNIT_ASSIGNED_CONTEXT((#45522,#45521,#45520))
REPRESENTATION_CONTEXT('dip','COMPONENT_PART')
);
#45478=(
GEOMETRIC_REPRESENTATION_CONTEXT(3)
GLOBAL_UNCERTAINTY_ASSIGNED_CONTEXT((#45506))
GLOBAL_UNIT_ASSIGNED_CONTEXT((#45522,#45521,#45520))
REPRESENTATION_CONTEXT('Neck_flat_seal','COMPONENT_PART')
);
#45479=(
GEOMETRIC_REPRESENTATION_CONTEXT(3)
GLOBAL_UNCERTAINTY_ASSIGNED_CONTEXT((#45507))
GLOBAL_UNIT_ASSIGNED_CONTEXT((#45522,#45521,#45520))
REPRESENTATION_CONTEXT('refill_port','COMPONENT_PART')
);
#45480=(
GEOMETRIC_REPRESENTATION_CONTEXT(3)
GLOBAL_UNCERTAINTY_ASSIGNED_CONTEXT((#45508))
GLOBAL_UNIT_ASSIGNED_CONTEXT((#45522,#45521,#45520))
REPRESENTATION_CONTEXT('ball_outlet_valve','COMPONENT_PART')
);
#45481=(
GEOMETRIC_REPRESENTATION_CONTEXT(3)
GLOBAL_UNCERTAINTY_ASSIGNED_CONTEXT((#45509))
GLOBAL_UNIT_ASSIGNED_CONTEXT((#45522,#45521,#45520))
REPRESENTATION_CONTEXT('Floating_ring','COMPONENT_PART')
);
#45482=(
GEOMETRIC_REPRESENTATION_CONTEXT(3)
GLOBAL_UNCERTAINTY_ASSIGNED_CONTEXT((#45510))
GLOBAL_UNIT_ASSIGNED_CONTEXT((#45522,#45521,#45520))
REPRESENTATION_CONTEXT('ball','COMPONENT_PART')
);
#45483=(
GEOMETRIC_REPRESENTATION_CONTEXT(3)
GLOBAL_UNCERTAINTY_ASSIGNED_CONTEXT((#45511))
GLOBAL_UNIT_ASSIGNED_CONTEXT((#45522,#45521,#45520))
REPRESENTATION_CONTEXT('screw_cover','COMPONENT_PART')
);
#45484=(
GEOMETRIC_REPRESENTATION_CONTEXT(3)
GLOBAL_UNCERTAINTY_ASSIGNED_CONTEXT((#45512))
GLOBAL_UNIT_ASSIGNED_CONTEXT((#45522,#45521,#45520))
REPRESENTATION_CONTEXT('refill+port_air_seal','COMPONENT_PART')
);
#45485=(
GEOMETRIC_REPRESENTATION_CONTEXT(3)
GLOBAL_UNCERTAINTY_ASSIGNED_CONTEXT((#45513))
GLOBAL_UNIT_ASSIGNED_CONTEXT((#45522,#45521,#45520))
REPRESENTATION_CONTEXT('Bottle','COMPONENT_PART')
);
#45486=(
GEOMETRIC_REPRESENTATION_CONTEXT(3)
GLOBAL_UNCERTAINTY_ASSIGNED_CONTEXT((#45514))
GLOBAL_UNIT_ASSIGNED_CONTEXT((#45522,#45521,#45520))
REPRESENTATION_CONTEXT('bottle_premium_cover','COMPONENT_PART')
);
#45487=(
GEOMETRIC_REPRESENTATION_CONTEXT(3)
GLOBAL_UNCERTAINTY_ASSIGNED_CONTEXT((#45515))
GLOBAL_UNIT_ASSIGNED_CONTEXT((#45522,#45521,#45520))
REPRESENTATION_CONTEXT('refill_screw','COMPONENT_PART')
);
#45488=(
GEOMETRIC_REPRESENTATION_CONTEXT(3)
GLOBAL_UNCERTAINTY_ASSIGNED_CONTEXT((#45516))
GLOBAL_UNIT_ASSIGNED_CONTEXT((#45522,#45521,#45520))
REPRESENTATION_CONTEXT('refill_port','COMPONENT_PART')
);
#45489=(
GEOMETRIC_REPRESENTATION_CONTEXT(3)
GLOBAL_UNCERTAINTY_ASSIGNED_CONTEXT((#45517))
GLOBAL_UNIT_ASSIGNED_CONTEXT((#45522,#45521,#45520))
REPRESENTATION_CONTEXT('ball_retainer','COMPONENT_PART')
);
#45490=(
GEOMETRIC_REPRESENTATION_CONTEXT(3)
GLOBAL_UNCERTAINTY_ASSIGNED_CONTEXT((#45518))
GLOBAL_UNIT_ASSIGNED_CONTEXT((#45522,#45521,#45520))
REPRESENTATION_CONTEXT('Bottle_Cap','COMPONENT_PART')
);
#45491=(
GEOMETRIC_REPRESENTATION_CONTEXT(3)
GLOBAL_UNCERTAINTY_ASSIGNED_CONTEXT((#45519))
GLOBAL_UNIT_ASSIGNED_CONTEXT((#45522,#45521,#45520))
REPRESENTATION_CONTEXT('o_ring','COMPONENT_PART')
);
#45492=UNCERTAINTY_MEASURE_WITH_UNIT(LENGTH_MEASURE(1.E-8),#45522,
'DISTANCE_ACCURACY_VALUE','Maximum Tolerance applied to model');
#45493=UNCERTAINTY_MEASURE_WITH_UNIT(LENGTH_MEASURE(2.E-5),#45522,
'DISTANCE_ACCURACY_VALUE','Maximum Tolerance applied to model');
#45494=UNCERTAINTY_MEASURE_WITH_UNIT(LENGTH_MEASURE(2.E-5),#45522,
'DISTANCE_ACCURACY_VALUE','Maximum Tolerance applied to model');
#45495=UNCERTAINTY_MEASURE_WITH_UNIT(LENGTH_MEASURE(2.E-5),#45522,
'DISTANCE_ACCURACY_VALUE','Maximum Tolerance applied to model');
#45496=UNCERTAINTY_MEASURE_WITH_UNIT(LENGTH_MEASURE(2.E-5),#45522,
'DISTANCE_ACCURACY_VALUE','Maximum Tolerance applied to model');
#45497=UNCERTAINTY_MEASURE_WITH_UNIT(LENGTH_MEASURE(1.E-8),#45522,
'DISTANCE_ACCURACY_VALUE','Maximum Tolerance applied to model');
#45498=UNCERTAINTY_MEASURE_WITH_UNIT(LENGTH_MEASURE(2.E-5),#45522,
'DISTANCE_ACCURACY_VALUE','Maximum Tolerance applied to model');
#45499=UNCERTAINTY_MEASURE_WITH_UNIT(LENGTH_MEASURE(1.E-6),#45522,
'DISTANCE_ACCURACY_VALUE','Maximum Tolerance applied to model');
#45500=UNCERTAINTY_MEASURE_WITH_UNIT(LENGTH_MEASURE(1.E-6),#45522,
'DISTANCE_ACCURACY_VALUE','Maximum Tolerance applied to model');
#45501=UNCERTAINTY_MEASURE_WITH_UNIT(LENGTH_MEASURE(1.E-8),#45522,
'DISTANCE_ACCURACY_VALUE','Maximum Tolerance applied to model');
#45502=UNCERTAINTY_MEASURE_WITH_UNIT(LENGTH_MEASURE(2.E-5),#45522,
'DISTANCE_ACCURACY_VALUE','Maximum Tolerance applied to model');
#45503=UNCERTAINTY_MEASURE_WITH_UNIT(LENGTH_MEASURE(1.E-8),#45522,
'DISTANCE_ACCURACY_VALUE','Maximum Tolerance applied to model');
#45504=UNCERTAINTY_MEASURE_WITH_UNIT(LENGTH_MEASURE(2.E-5),#45522,
'DISTANCE_ACCURACY_VALUE','Maximum Tolerance applied to model');
#45505=UNCERTAINTY_MEASURE_WITH_UNIT(LENGTH_MEASURE(1.E-8),#45522,
'DISTANCE_ACCURACY_VALUE','Maximum Tolerance applied to model');
#45506=UNCERTAINTY_MEASURE_WITH_UNIT(LENGTH_MEASURE(1.E-8),#45522,
'DISTANCE_ACCURACY_VALUE','Maximum Tolerance applied to model');
#45507=UNCERTAINTY_MEASURE_WITH_UNIT(LENGTH_MEASURE(1.E-6),#45522,
'DISTANCE_ACCURACY_VALUE','Maximum Tolerance applied to model');
#45508=UNCERTAINTY_MEASURE_WITH_UNIT(LENGTH_MEASURE(1.E-8),#45522,
'DISTANCE_ACCURACY_VALUE','Maximum Tolerance applied to model');
#45509=UNCERTAINTY_MEASURE_WITH_UNIT(LENGTH_MEASURE(1.E-6),#45522,
'DISTANCE_ACCURACY_VALUE','Maximum Tolerance applied to model');
#45510=UNCERTAINTY_MEASURE_WITH_UNIT(LENGTH_MEASURE(1.E-8),#45522,
'DISTANCE_ACCURACY_VALUE','Maximum Tolerance applied to model');
#45511=UNCERTAINTY_MEASURE_WITH_UNIT(LENGTH_MEASURE(1.E-6),#45522,
'DISTANCE_ACCURACY_VALUE','Maximum Tolerance applied to model');
#45512=UNCERTAINTY_MEASURE_WITH_UNIT(LENGTH_MEASURE(1.E-6),#45522,
'DISTANCE_ACCURACY_VALUE','Maximum Tolerance applied to model');
#45513=UNCERTAINTY_MEASURE_WITH_UNIT(LENGTH_MEASURE(2.E-5),#45522,
'DISTANCE_ACCURACY_VALUE','Maximum Tolerance applied to model');
#45514=UNCERTAINTY_MEASURE_WITH_UNIT(LENGTH_MEASURE(1.E-6),#45522,
'DISTANCE_ACCURACY_VALUE','Maximum Tolerance applied to model');
#45515=UNCERTAINTY_MEASURE_WITH_UNIT(LENGTH_MEASURE(2.E-5),#45522,
'DISTANCE_ACCURACY_VALUE','Maximum Tolerance applied to model');
#45516=UNCERTAINTY_MEASURE_WITH_UNIT(LENGTH_MEASURE(2.E-5),#45522,
'DISTANCE_ACCURACY_VALUE','Maximum Tolerance applied to model');
#45517=UNCERTAINTY_MEASURE_WITH_UNIT(LENGTH_MEASURE(1.E-6),#45522,
'DISTANCE_ACCURACY_VALUE','Maximum Tolerance applied to model');
#45518=UNCERTAINTY_MEASURE_WITH_UNIT(LENGTH_MEASURE(2.E-5),#45522,
'DISTANCE_ACCURACY_VALUE','Maximum Tolerance applied to model');
#45519=UNCERTAINTY_MEASURE_WITH_UNIT(LENGTH_MEASURE(1.E-8),#45522,
'DISTANCE_ACCURACY_VALUE','Maximum Tolerance applied to model');
#45520=(
NAMED_UNIT(*)
SI_UNIT($,.STERADIAN.)
SOLID_ANGLE_UNIT()
);
#45521=(
NAMED_UNIT(*)
PLANE_ANGLE_UNIT()
SI_UNIT($,.RADIAN.)
);
#45522=(
LENGTH_UNIT()
NAMED_UNIT(*)
SI_UNIT($,.METRE.)
);
#45523=PRODUCT_DEFINITION_SHAPE('','',#45585);
#45524=PRODUCT_DEFINITION_SHAPE('','',#45586);
#45525=PRODUCT_DEFINITION_SHAPE(' ','NAUO PRDDFN',#99);
#45526=PRODUCT_DEFINITION_SHAPE('','',#45587);
#45527=PRODUCT_DEFINITION_SHAPE(' ','NAUO PRDDFN',#100);
#45528=PRODUCT_DEFINITION_SHAPE('','',#45588);
#45529=PRODUCT_DEFINITION_SHAPE(' ','NAUO PRDDFN',#101);
#45530=PRODUCT_DEFINITION_SHAPE('','',#45589);
#45531=PRODUCT_DEFINITION_SHAPE(' ','NAUO PRDDFN',#102);
#45532=PRODUCT_DEFINITION_SHAPE('','',#45590);
#45533=PRODUCT_DEFINITION_SHAPE(' ','NAUO PRDDFN',#103);
#45534=PRODUCT_DEFINITION_SHAPE('','',#45591);
#45535=PRODUCT_DEFINITION_SHAPE(' ','NAUO PRDDFN',#104);
#45536=PRODUCT_DEFINITION_SHAPE('','',#45592);
#45537=PRODUCT_DEFINITION_SHAPE(' ','NAUO PRDDFN',#105);
#45538=PRODUCT_DEFINITION_SHAPE(' ','NAUO PRDDFN',#106);
#45539=PRODUCT_DEFINITION_SHAPE('','',#45593);
#45540=PRODUCT_DEFINITION_SHAPE(' ','NAUO PRDDFN',#107);
#45541=PRODUCT_DEFINITION_SHAPE(' ','NAUO PRDDFN',#108);
#45542=PRODUCT_DEFINITION_SHAPE('','',#45594);
#45543=PRODUCT_DEFINITION_SHAPE(' ','NAUO PRDDFN',#109);
#45544=PRODUCT_DEFINITION_SHAPE('','',#45595);
#45545=PRODUCT_DEFINITION_SHAPE(' ','NAUO PRDDFN',#110);
#45546=PRODUCT_DEFINITION_SHAPE('','',#45596);
#45547=PRODUCT_DEFINITION_SHAPE(' ','NAUO PRDDFN',#111);
#45548=PRODUCT_DEFINITION_SHAPE('','',#45597);
#45549=PRODUCT_DEFINITION_SHAPE(' ','NAUO PRDDFN',#112);
#45550=PRODUCT_DEFINITION_SHAPE('','',#45598);
#45551=PRODUCT_DEFINITION_SHAPE(' ','NAUO PRDDFN',#113);
#45552=PRODUCT_DEFINITION_SHAPE('','',#45599);
#45553=PRODUCT_DEFINITION_SHAPE(' ','NAUO PRDDFN',#114);
#45554=PRODUCT_DEFINITION_SHAPE(' ','NAUO PRDDFN',#115);
#45555=PRODUCT_DEFINITION_SHAPE('','',#45600);
#45556=PRODUCT_DEFINITION_SHAPE(' ','NAUO PRDDFN',#116);
#45557=PRODUCT_DEFINITION_SHAPE('','',#45601);
#45558=PRODUCT_DEFINITION_SHAPE(' ','NAUO PRDDFN',#117);
#45559=PRODUCT_DEFINITION_SHAPE('','',#45602);
#45560=PRODUCT_DEFINITION_SHAPE(' ','NAUO PRDDFN',#118);
#45561=PRODUCT_DEFINITION_SHAPE('','',#45603);
#45562=PRODUCT_DEFINITION_SHAPE(' ','NAUO PRDDFN',#119);
#45563=PRODUCT_DEFINITION_SHAPE(' ','NAUO PRDDFN',#120);
#45564=PRODUCT_DEFINITION_SHAPE(' ','NAUO PRDDFN',#121);
#45565=PRODUCT_DEFINITION_SHAPE('','',#45604);
#45566=PRODUCT_DEFINITION_SHAPE(' ','NAUO PRDDFN',#122);
#45567=PRODUCT_DEFINITION_SHAPE('','',#45605);
#45568=PRODUCT_DEFINITION_SHAPE(' ','NAUO PRDDFN',#123);
#45569=PRODUCT_DEFINITION_SHAPE('','',#45606);
#45570=PRODUCT_DEFINITION_SHAPE(' ','NAUO PRDDFN',#124);
#45571=PRODUCT_DEFINITION_SHAPE(' ','NAUO PRDDFN',#125);
#45572=PRODUCT_DEFINITION_SHAPE('','',#45607);
#45573=PRODUCT_DEFINITION_SHAPE(' ','NAUO PRDDFN',#126);
#45574=PRODUCT_DEFINITION_SHAPE('','',#45608);
#45575=PRODUCT_DEFINITION_SHAPE(' ','NAUO PRDDFN',#127);
#45576=PRODUCT_DEFINITION_SHAPE(' ','NAUO PRDDFN',#128);
#45577=PRODUCT_DEFINITION_SHAPE('','',#45609);
#45578=PRODUCT_DEFINITION_SHAPE(' ','NAUO PRDDFN',#129);
#45579=PRODUCT_DEFINITION_SHAPE('','',#45610);
#45580=PRODUCT_DEFINITION_SHAPE(' ','NAUO PRDDFN',#130);
#45581=PRODUCT_DEFINITION_SHAPE('','',#45611);
#45582=PRODUCT_DEFINITION_SHAPE(' ','NAUO PRDDFN',#131);
#45583=PRODUCT_DEFINITION_SHAPE('','',#45612);
#45584=PRODUCT_DEFINITION_SHAPE(' ','NAUO PRDDFN',#132);
#45585=PRODUCT_DEFINITION('','',#45641,#45613);
#45586=PRODUCT_DEFINITION('','',#45642,#45614);
#45587=PRODUCT_DEFINITION('','',#45643,#45615);
#45588=PRODUCT_DEFINITION('','',#45644,#45616);
#45589=PRODUCT_DEFINITION('','',#45645,#45617);
#45590=PRODUCT_DEFINITION('','',#45646,#45618);
#45591=PRODUCT_DEFINITION('','',#45647,#45619);
#45592=PRODUCT_DEFINITION('','',#45648,#45620);
#45593=PRODUCT_DEFINITION('','',#45649,#45621);
#45594=PRODUCT_DEFINITION('','',#45650,#45622);
#45595=PRODUCT_DEFINITION('','',#45651,#45623);
#45596=PRODUCT_DEFINITION('','',#45652,#45624);
#45597=PRODUCT_DEFINITION('','',#45653,#45625);
#45598=PRODUCT_DEFINITION('','',#45654,#45626);
#45599=PRODUCT_DEFINITION('','',#45655,#45627);
#45600=PRODUCT_DEFINITION('','',#45656,#45628);
#45601=PRODUCT_DEFINITION('','',#45657,#45629);
#45602=PRODUCT_DEFINITION('','',#45658,#45630);
#45603=PRODUCT_DEFINITION('','',#45659,#45631);
#45604=PRODUCT_DEFINITION('','',#45660,#45632);
#45605=PRODUCT_DEFINITION('','',#45661,#45633);
#45606=PRODUCT_DEFINITION('','',#45662,#45634);
#45607=PRODUCT_DEFINITION('','',#45663,#45635);
#45608=PRODUCT_DEFINITION('','',#45664,#45636);
#45609=PRODUCT_DEFINITION('','',#45665,#45637);
#45610=PRODUCT_DEFINITION('','',#45666,#45638);
#45611=PRODUCT_DEFINITION('','',#45667,#45639);
#45612=PRODUCT_DEFINITION('','',#45668,#45640);
#45613=PRODUCT_DEFINITION_CONTEXT('',#45782,'design');
#45614=PRODUCT_DEFINITION_CONTEXT('',#45782,'design');
#45615=PRODUCT_DEFINITION_CONTEXT('',#45782,'design');
#45616=PRODUCT_DEFINITION_CONTEXT('',#45782,'design');
#45617=PRODUCT_DEFINITION_CONTEXT('',#45782,'design');
#45618=PRODUCT_DEFINITION_CONTEXT('',#45782,'design');
#45619=PRODUCT_DEFINITION_CONTEXT('',#45782,'design');
#45620=PRODUCT_DEFINITION_CONTEXT('',#45782,'design');
#45621=PRODUCT_DEFINITION_CONTEXT('',#45782,'design');
#45622=PRODUCT_DEFINITION_CONTEXT('',#45782,'design');
#45623=PRODUCT_DEFINITION_CONTEXT('',#45782,'design');
#45624=PRODUCT_DEFINITION_CONTEXT('',#45782,'design');
#45625=PRODUCT_DEFINITION_CONTEXT('',#45782,'design');
#45626=PRODUCT_DEFINITION_CONTEXT('',#45782,'design');
#45627=PRODUCT_DEFINITION_CONTEXT('',#45782,'design');
#45628=PRODUCT_DEFINITION_CONTEXT('',#45782,'design');
#45629=PRODUCT_DEFINITION_CONTEXT('',#45782,'design');
#45630=PRODUCT_DEFINITION_CONTEXT('',#45782,'design');
#45631=PRODUCT_DEFINITION_CONTEXT('',#45782,'design');
#45632=PRODUCT_DEFINITION_CONTEXT('',#45782,'design');
#45633=PRODUCT_DEFINITION_CONTEXT('',#45782,'design');
#45634=PRODUCT_DEFINITION_CONTEXT('',#45782,'design');
#45635=PRODUCT_DEFINITION_CONTEXT('',#45782,'design');
#45636=PRODUCT_DEFINITION_CONTEXT('',#45782,'design');
#45637=PRODUCT_DEFINITION_CONTEXT('',#45782,'design');
#45638=PRODUCT_DEFINITION_CONTEXT('',#45782,'design');
#45639=PRODUCT_DEFINITION_CONTEXT('',#45782,'design');
#45640=PRODUCT_DEFINITION_CONTEXT('',#45782,'design');
#45641=PRODUCT_DEFINITION_FORMATION_WITH_SPECIFIED_SOURCE('','',#45697,
 .NOT_KNOWN.);
#45642=PRODUCT_DEFINITION_FORMATION_WITH_SPECIFIED_SOURCE('','',#45698,
 .NOT_KNOWN.);
#45643=PRODUCT_DEFINITION_FORMATION_WITH_SPECIFIED_SOURCE('','',#45699,
 .NOT_KNOWN.);
#45644=PRODUCT_DEFINITION_FORMATION_WITH_SPECIFIED_SOURCE('','',#45700,
 .NOT_KNOWN.);
#45645=PRODUCT_DEFINITION_FORMATION_WITH_SPECIFIED_SOURCE('','',#45701,
 .NOT_KNOWN.);
#45646=PRODUCT_DEFINITION_FORMATION_WITH_SPECIFIED_SOURCE('','',#45702,
 .NOT_KNOWN.);
#45647=PRODUCT_DEFINITION_FORMATION_WITH_SPECIFIED_SOURCE('','',#45703,
 .NOT_KNOWN.);
#45648=PRODUCT_DEFINITION_FORMATION_WITH_SPECIFIED_SOURCE('','',#45704,
 .NOT_KNOWN.);
#45649=PRODUCT_DEFINITION_FORMATION_WITH_SPECIFIED_SOURCE('','',#45705,
 .NOT_KNOWN.);
#45650=PRODUCT_DEFINITION_FORMATION_WITH_SPECIFIED_SOURCE('','',#45706,
 .NOT_KNOWN.);
#45651=PRODUCT_DEFINITION_FORMATION_WITH_SPECIFIED_SOURCE('','',#45707,
 .NOT_KNOWN.);
#45652=PRODUCT_DEFINITION_FORMATION_WITH_SPECIFIED_SOURCE('','',#45708,
 .NOT_KNOWN.);
#45653=PRODUCT_DEFINITION_FORMATION_WITH_SPECIFIED_SOURCE('','',#45709,
 .NOT_KNOWN.);
#45654=PRODUCT_DEFINITION_FORMATION_WITH_SPECIFIED_SOURCE('','',#45710,
 .NOT_KNOWN.);
#45655=PRODUCT_DEFINITION_FORMATION_WITH_SPECIFIED_SOURCE('','',#45711,
 .NOT_KNOWN.);
#45656=PRODUCT_DEFINITION_FORMATION_WITH_SPECIFIED_SOURCE('','',#45712,
 .NOT_KNOWN.);
#45657=PRODUCT_DEFINITION_FORMATION_WITH_SPECIFIED_SOURCE('','',#45713,
 .NOT_KNOWN.);
#45658=PRODUCT_DEFINITION_FORMATION_WITH_SPECIFIED_SOURCE('','',#45714,
 .NOT_KNOWN.);
#45659=PRODUCT_DEFINITION_FORMATION_WITH_SPECIFIED_SOURCE('','',#45715,
 .NOT_KNOWN.);
#45660=PRODUCT_DEFINITION_FORMATION_WITH_SPECIFIED_SOURCE('','',#45716,
 .NOT_KNOWN.);
#45661=PRODUCT_DEFINITION_FORMATION_WITH_SPECIFIED_SOURCE('','',#45717,
 .NOT_KNOWN.);
#45662=PRODUCT_DEFINITION_FORMATION_WITH_SPECIFIED_SOURCE('','',#45718,
 .NOT_KNOWN.);
#45663=PRODUCT_DEFINITION_FORMATION_WITH_SPECIFIED_SOURCE('','',#45719,
 .NOT_KNOWN.);
#45664=PRODUCT_DEFINITION_FORMATION_WITH_SPECIFIED_SOURCE('','',#45720,
 .NOT_KNOWN.);
#45665=PRODUCT_DEFINITION_FORMATION_WITH_SPECIFIED_SOURCE('','',#45721,
 .NOT_KNOWN.);
#45666=PRODUCT_DEFINITION_FORMATION_WITH_SPECIFIED_SOURCE('','',#45722,
 .NOT_KNOWN.);
#45667=PRODUCT_DEFINITION_FORMATION_WITH_SPECIFIED_SOURCE('','',#45723,
 .NOT_KNOWN.);
#45668=PRODUCT_DEFINITION_FORMATION_WITH_SPECIFIED_SOURCE('','',#45724,
 .NOT_KNOWN.);
#45669=PRODUCT_RELATED_PRODUCT_CATEGORY('','',(#45697));
#45670=PRODUCT_RELATED_PRODUCT_CATEGORY('','',(#45698));
#45671=PRODUCT_RELATED_PRODUCT_CATEGORY('','',(#45699));
#45672=PRODUCT_RELATED_PRODUCT_CATEGORY('','',(#45700));
#45673=PRODUCT_RELATED_PRODUCT_CATEGORY('','',(#45701));
#45674=PRODUCT_RELATED_PRODUCT_CATEGORY('','',(#45702));
#45675=PRODUCT_RELATED_PRODUCT_CATEGORY('','',(#45703));
#45676=PRODUCT_RELATED_PRODUCT_CATEGORY('','',(#45704));
#45677=PRODUCT_RELATED_PRODUCT_CATEGORY('','',(#45705));
#45678=PRODUCT_RELATED_PRODUCT_CATEGORY('','',(#45706));
#45679=PRODUCT_RELATED_PRODUCT_CATEGORY('','',(#45707));
#45680=PRODUCT_RELATED_PRODUCT_CATEGORY('','',(#45708));
#45681=PRODUCT_RELATED_PRODUCT_CATEGORY('','',(#45709));
#45682=PRODUCT_RELATED_PRODUCT_CATEGORY('','',(#45710));
#45683=PRODUCT_RELATED_PRODUCT_CATEGORY('','',(#45711));
#45684=PRODUCT_RELATED_PRODUCT_CATEGORY('','',(#45712));
#45685=PRODUCT_RELATED_PRODUCT_CATEGORY('','',(#45713));
#45686=PRODUCT_RELATED_PRODUCT_CATEGORY('','',(#45714));
#45687=PRODUCT_RELATED_PRODUCT_CATEGORY('','',(#45715));
#45688=PRODUCT_RELATED_PRODUCT_CATEGORY('','',(#45716));
#45689=PRODUCT_RELATED_PRODUCT_CATEGORY('','',(#45717));
#45690=PRODUCT_RELATED_PRODUCT_CATEGORY('','',(#45718));
#45691=PRODUCT_RELATED_PRODUCT_CATEGORY('','',(#45719));
#45692=PRODUCT_RELATED_PRODUCT_CATEGORY('','',(#45720));
#45693=PRODUCT_RELATED_PRODUCT_CATEGORY('','',(#45721));
#45694=PRODUCT_RELATED_PRODUCT_CATEGORY('','',(#45722));
#45695=PRODUCT_RELATED_PRODUCT_CATEGORY('','',(#45723));
#45696=PRODUCT_RELATED_PRODUCT_CATEGORY('','',(#45724));
#45697=PRODUCT('MAS-690','MAS-690','MAS-690',(#45753));
#45698=PRODUCT('Top_acces_nozzle_supporter',
'Top_acces_nozzle_supporter','Top_acces_nozzle_supporter',(#45754));
#45699=PRODUCT('piston','piston','piston',(#45755));
#45700=PRODUCT('75632s_.prt','75632s_.prt','75632s_.prt',(#45756));
#45701=PRODUCT('refill_cap','refill_cap','refill_cap',(#45757));
#45702=PRODUCT('spring','spring','spring',(#45758));
#45703=PRODUCT('floating_ring_bottom_connector',
'floating_ring_bottom_connector','floating_ring_bottom_connector',(#45759));
#45704=PRODUCT('binding head screw_ai_CR-BHMS 0.099-48x0.25x0.25-N',
'binding head screw_ai_CR-BHMS 0.099-48x0.25x0.25-N',
'binding head screw_ai_CR-BHMS 0.099-48x0.25x0.25-N',(#45760));
#45705=PRODUCT('Floating_ring_guide','Floating_ring_guide',
'Floating_ring_guide',(#45761));
#45706=PRODUCT('Bottle_Nech_Seal','Bottle_Nech_Seal','Bottle_Nech_Seal',
(#45762));
#45707=PRODUCT('refill_cap','refill_cap','refill_cap',(#45763));
#45708=PRODUCT('main_housing','main_housing','main_housing',(#45764));
#45709=PRODUCT('Nozzle cap','Nozzle cap','Nozzle cap',(#45765));
#45710=PRODUCT('dip','dip','dip',(#45766));
#45711=PRODUCT('Neck_flat_seal','Neck_flat_seal','Neck_flat_seal',(#45767));
#45712=PRODUCT('refill_port','refill_port','refill_port',(#45768));
#45713=PRODUCT('ball_outlet_valve','ball_outlet_valve',
'ball_outlet_valve',(#45769));
#45714=PRODUCT('Floating_ring','Floating_ring','Floating_ring',(#45770));
#45715=PRODUCT('ball','ball','ball',(#45771));
#45716=PRODUCT('screw_cover','screw_cover','screw_cover',(#45772));
#45717=PRODUCT('refill+port_air_seal','refill+port_air_seal',
'refill+port_air_seal',(#45773));
#45718=PRODUCT('Bottle','Bottle','Bottle',(#45774));
#45719=PRODUCT('bottle_premium_cover','bottle_premium_cover',
'bottle_premium_cover',(#45775));
#45720=PRODUCT('refill_screw','refill_screw','refill_screw',(#45776));
#45721=PRODUCT('refill_port','refill_port','refill_port',(#45777));
#45722=PRODUCT('ball_retainer','ball_retainer','ball_retainer',(#45778));
#45723=PRODUCT('Bottle_Cap','Bottle_Cap','Bottle_Cap',(#45779));
#45724=PRODUCT('o_ring','o_ring','o_ring',(#45780));
#45725=PRODUCT_CATEGORY('','');
#45726=PRODUCT_CATEGORY('','');
#45727=PRODUCT_CATEGORY('','');
#45728=PRODUCT_CATEGORY('','');
#45729=PRODUCT_CATEGORY('','');
#45730=PRODUCT_CATEGORY('','');
#45731=PRODUCT_CATEGORY('','');
#45732=PRODUCT_CATEGORY('','');
#45733=PRODUCT_CATEGORY('','');
#45734=PRODUCT_CATEGORY('','');
#45735=PRODUCT_CATEGORY('','');
#45736=PRODUCT_CATEGORY('','');
#45737=PRODUCT_CATEGORY('','');
#45738=PRODUCT_CATEGORY('','');
#45739=PRODUCT_CATEGORY('','');
#45740=PRODUCT_CATEGORY('','');
#45741=PRODUCT_CATEGORY('','');
#45742=PRODUCT_CATEGORY('','');
#45743=PRODUCT_CATEGORY('','');
#45744=PRODUCT_CATEGORY('','');
#45745=PRODUCT_CATEGORY('','');
#45746=PRODUCT_CATEGORY('','');
#45747=PRODUCT_CATEGORY('','');
#45748=PRODUCT_CATEGORY('','');
#45749=PRODUCT_CATEGORY('','');
#45750=PRODUCT_CATEGORY('','');
#45751=PRODUCT_CATEGORY('','');
#45752=PRODUCT_CATEGORY('','');
#45753=PRODUCT_CONTEXT('',#45782,'mechanical');
#45754=PRODUCT_CONTEXT('',#45782,'mechanical');
#45755=PRODUCT_CONTEXT('',#45782,'mechanical');
#45756=PRODUCT_CONTEXT('',#45782,'mechanical');
#45757=PRODUCT_CONTEXT('',#45782,'mechanical');
#45758=PRODUCT_CONTEXT('',#45782,'mechanical');
#45759=PRODUCT_CONTEXT('',#45782,'mechanical');
#45760=PRODUCT_CONTEXT('',#45782,'mechanical');
#45761=PRODUCT_CONTEXT('',#45782,'mechanical');
#45762=PRODUCT_CONTEXT('',#45782,'mechanical');
#45763=PRODUCT_CONTEXT('',#45782,'mechanical');
#45764=PRODUCT_CONTEXT('',#45782,'mechanical');
#45765=PRODUCT_CONTEXT('',#45782,'mechanical');
#45766=PRODUCT_CONTEXT('',#45782,'mechanical');
#45767=PRODUCT_CONTEXT('',#45782,'mechanical');
#45768=PRODUCT_CONTEXT('',#45782,'mechanical');
#45769=PRODUCT_CONTEXT('',#45782,'mechanical');
#45770=PRODUCT_CONTEXT('',#45782,'mechanical');
#45771=PRODUCT_CONTEXT('',#45782,'mechanical');
#45772=PRODUCT_CONTEXT('',#45782,'mechanical');
#45773=PRODUCT_CONTEXT('',#45782,'mechanical');
#45774=PRODUCT_CONTEXT('',#45782,'mechanical');
#45775=PRODUCT_CONTEXT('',#45782,'mechanical');
#45776=PRODUCT_CONTEXT('',#45782,'mechanical');
#45777=PRODUCT_CONTEXT('',#45782,'mechanical');
#45778=PRODUCT_CONTEXT('',#45782,'mechanical');
#45779=PRODUCT_CONTEXT('',#45782,'mechanical');
#45780=PRODUCT_CONTEXT('',#45782,'mechanical');
#45781=APPLICATION_PROTOCOL_DEFINITION('international standard',
'ap242_managed_model_based_3d_engineering',2020,#45782);
#45782=APPLICATION_CONTEXT('managed model based 3d engineering');
ENDSEC;
END-ISO-10303-21;
